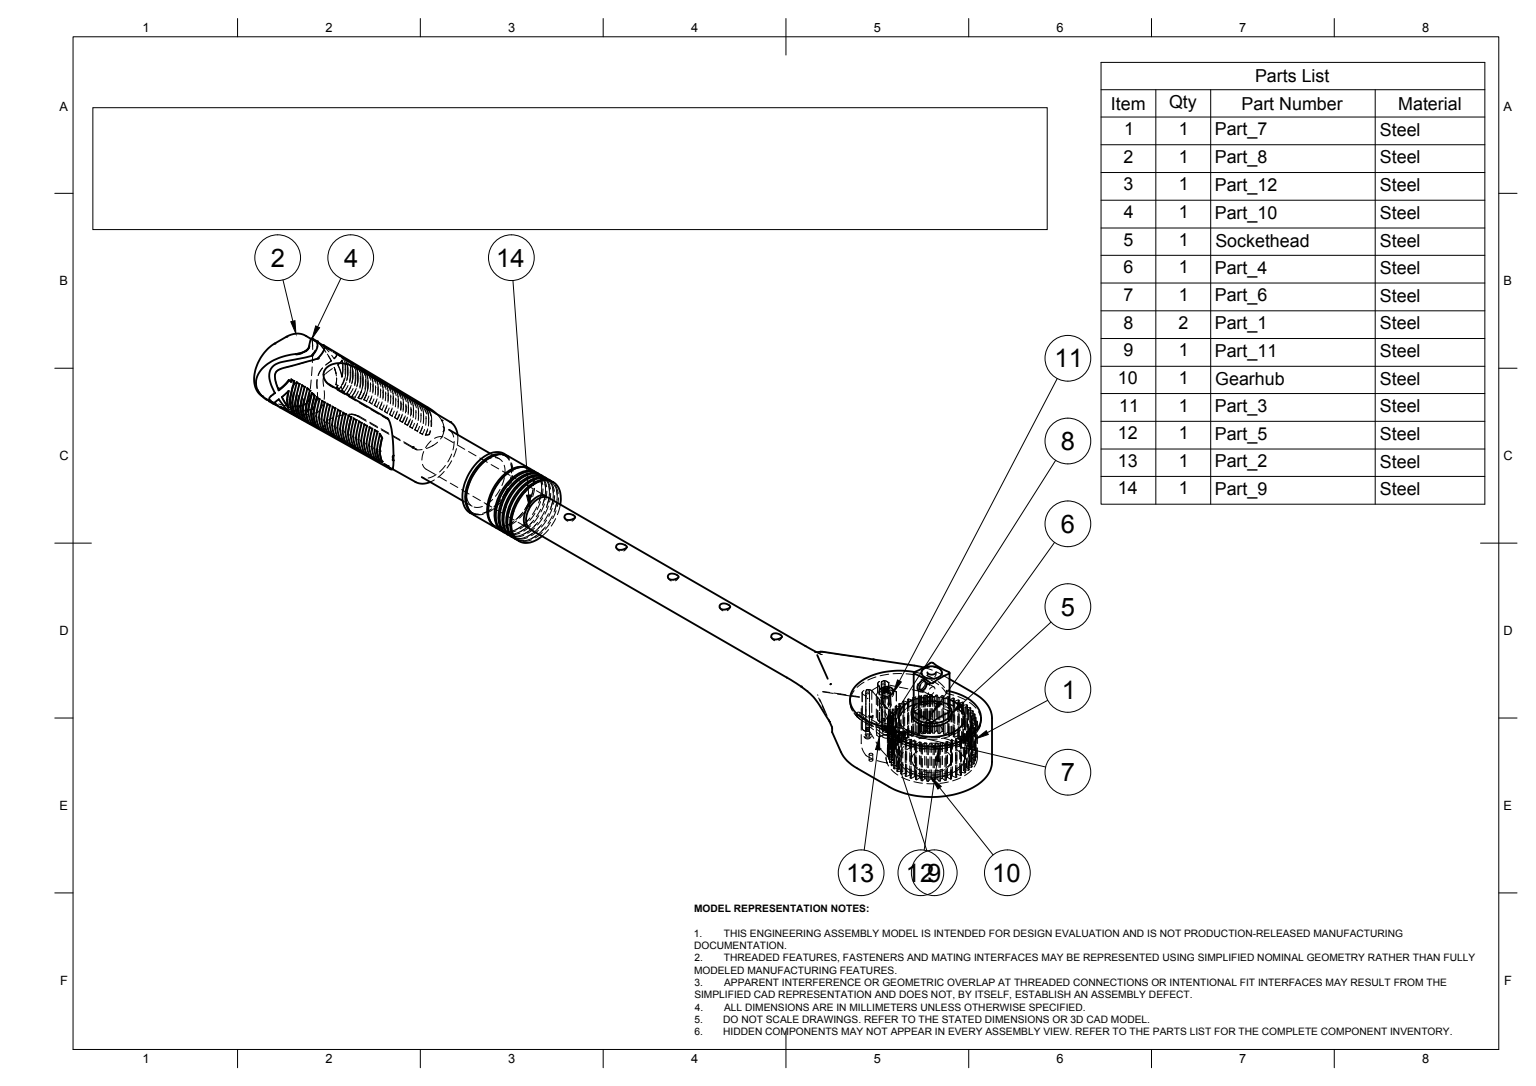
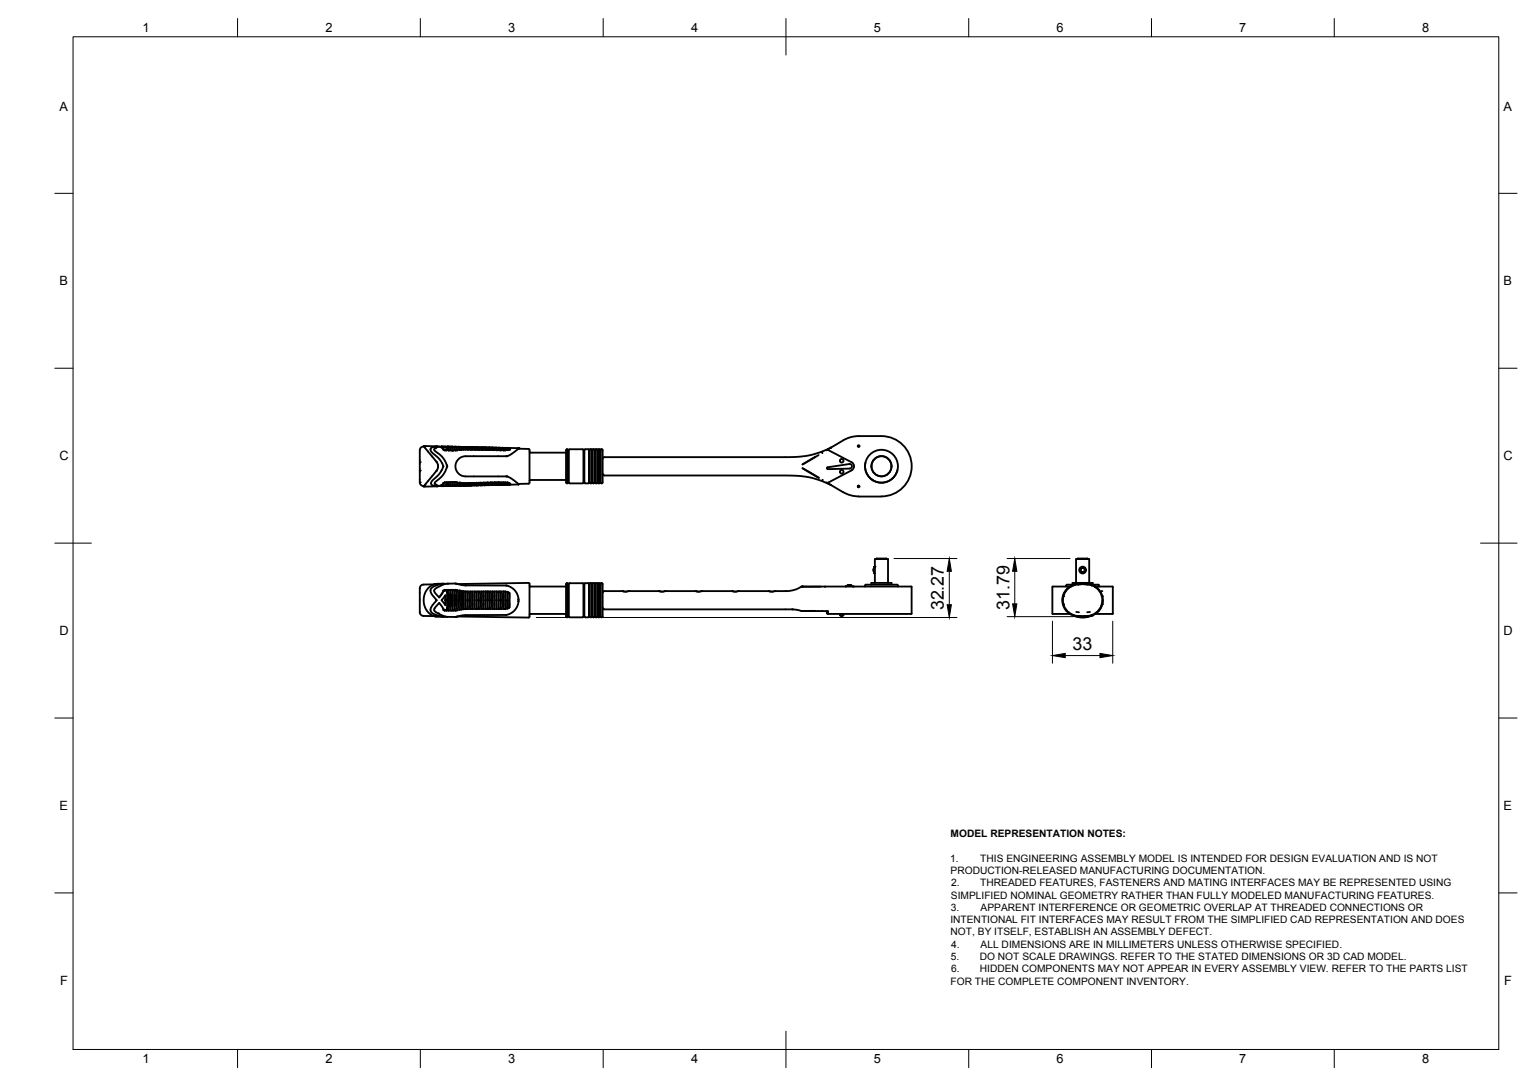
ISO-10303-21;
HEADER;
/* Generated by software containing ST-Developer
 * from STEP Tools, Inc. (www.steptools.com) 
 */

FILE_DESCRIPTION(
/* description */ ('STEP AP242 Edition 2'),
/* implementation_level */ '2;1');

FILE_NAME(
/* name */ 'MAS-615',
/* time_stamp */ '2026-10-06T10:11:12-07:00',
/* author */ (''),
/* organization */ (''),
/* preprocessor_version */ 'ST-DEVELOPER v20.2',
/* originating_system */ 'Autodesk Translation Framework v15.15.0.0',
/* authorisation */ '');

FILE_SCHEMA (('AUTOMOTIVE_DESIGN { 1 0 10303 214 3 1 1 }'));
ENDSEC;

DATA;
#10=MECHANICAL_DESIGN_GEOMETRIC_PRESENTATION_REPRESENTATION('',(#1771,#1772,
#1773,#1774,#1775,#1776,#1777,#1778,#1779,#1780,#1781,#1782,#1783,#1784,
#1785,#1786,#1787,#1788,#1789,#1790,#1791,#1792,#1793,#1794,#1795,#1796,
#1797,#1798,#1799,#1800),#54580);
#11=ITEM_DEFINED_TRANSFORMATION($,$,#17836,#19586);
#12=ITEM_DEFINED_TRANSFORMATION($,$,#18394,#19587);
#13=ITEM_DEFINED_TRANSFORMATION($,$,#18517,#19588);
#14=ITEM_DEFINED_TRANSFORMATION($,$,#18520,#19589);
#15=ITEM_DEFINED_TRANSFORMATION($,$,#18747,#19590);
#16=ITEM_DEFINED_TRANSFORMATION($,$,#18812,#19591);
#17=ITEM_DEFINED_TRANSFORMATION($,$,#18922,#19592);
#18=ITEM_DEFINED_TRANSFORMATION($,$,#19577,#19593);
#19=ITEM_DEFINED_TRANSFORMATION($,$,#19048,#19594);
#20=ITEM_DEFINED_TRANSFORMATION($,$,#19063,#19595);
#21=ITEM_DEFINED_TRANSFORMATION($,$,#19079,#19596);
#22=ITEM_DEFINED_TRANSFORMATION($,$,#19138,#19597);
#23=ITEM_DEFINED_TRANSFORMATION($,$,#19199,#19598);
#24=ITEM_DEFINED_TRANSFORMATION($,$,#19293,#19599);
#25=ITEM_DEFINED_TRANSFORMATION($,$,#19577,#19600);
#26=(
REPRESENTATION_RELATIONSHIP($,$,#54630,#54629)
REPRESENTATION_RELATIONSHIP_WITH_TRANSFORMATION(#11)
SHAPE_REPRESENTATION_RELATIONSHIP()
);
#27=(
REPRESENTATION_RELATIONSHIP($,$,#54631,#54629)
REPRESENTATION_RELATIONSHIP_WITH_TRANSFORMATION(#12)
SHAPE_REPRESENTATION_RELATIONSHIP()
);
#28=(
REPRESENTATION_RELATIONSHIP($,$,#54632,#54629)
REPRESENTATION_RELATIONSHIP_WITH_TRANSFORMATION(#13)
SHAPE_REPRESENTATION_RELATIONSHIP()
);
#29=(
REPRESENTATION_RELATIONSHIP($,$,#54633,#54629)
REPRESENTATION_RELATIONSHIP_WITH_TRANSFORMATION(#14)
SHAPE_REPRESENTATION_RELATIONSHIP()
);
#30=(
REPRESENTATION_RELATIONSHIP($,$,#54634,#54629)
REPRESENTATION_RELATIONSHIP_WITH_TRANSFORMATION(#15)
SHAPE_REPRESENTATION_RELATIONSHIP()
);
#31=(
REPRESENTATION_RELATIONSHIP($,$,#54635,#54629)
REPRESENTATION_RELATIONSHIP_WITH_TRANSFORMATION(#16)
SHAPE_REPRESENTATION_RELATIONSHIP()
);
#32=(
REPRESENTATION_RELATIONSHIP($,$,#54636,#54629)
REPRESENTATION_RELATIONSHIP_WITH_TRANSFORMATION(#17)
SHAPE_REPRESENTATION_RELATIONSHIP()
);
#33=(
REPRESENTATION_RELATIONSHIP($,$,#54643,#54629)
REPRESENTATION_RELATIONSHIP_WITH_TRANSFORMATION(#18)
SHAPE_REPRESENTATION_RELATIONSHIP()
);
#34=(
REPRESENTATION_RELATIONSHIP($,$,#54637,#54629)
REPRESENTATION_RELATIONSHIP_WITH_TRANSFORMATION(#19)
SHAPE_REPRESENTATION_RELATIONSHIP()
);
#35=(
REPRESENTATION_RELATIONSHIP($,$,#54638,#54629)
REPRESENTATION_RELATIONSHIP_WITH_TRANSFORMATION(#20)
SHAPE_REPRESENTATION_RELATIONSHIP()
);
#36=(
REPRESENTATION_RELATIONSHIP($,$,#54639,#54629)
REPRESENTATION_RELATIONSHIP_WITH_TRANSFORMATION(#21)
SHAPE_REPRESENTATION_RELATIONSHIP()
);
#37=(
REPRESENTATION_RELATIONSHIP($,$,#54640,#54629)
REPRESENTATION_RELATIONSHIP_WITH_TRANSFORMATION(#22)
SHAPE_REPRESENTATION_RELATIONSHIP()
);
#38=(
REPRESENTATION_RELATIONSHIP($,$,#54641,#54629)
REPRESENTATION_RELATIONSHIP_WITH_TRANSFORMATION(#23)
SHAPE_REPRESENTATION_RELATIONSHIP()
);
#39=(
REPRESENTATION_RELATIONSHIP($,$,#54642,#54629)
REPRESENTATION_RELATIONSHIP_WITH_TRANSFORMATION(#24)
SHAPE_REPRESENTATION_RELATIONSHIP()
);
#40=(
REPRESENTATION_RELATIONSHIP($,$,#54643,#54629)
REPRESENTATION_RELATIONSHIP_WITH_TRANSFORMATION(#25)
SHAPE_REPRESENTATION_RELATIONSHIP()
);
#41=CONTEXT_DEPENDENT_SHAPE_REPRESENTATION(#26,#54614);
#42=CONTEXT_DEPENDENT_SHAPE_REPRESENTATION(#27,#54615);
#43=CONTEXT_DEPENDENT_SHAPE_REPRESENTATION(#28,#54616);
#44=CONTEXT_DEPENDENT_SHAPE_REPRESENTATION(#29,#54617);
#45=CONTEXT_DEPENDENT_SHAPE_REPRESENTATION(#30,#54618);
#46=CONTEXT_DEPENDENT_SHAPE_REPRESENTATION(#31,#54619);
#47=CONTEXT_DEPENDENT_SHAPE_REPRESENTATION(#32,#54620);
#48=CONTEXT_DEPENDENT_SHAPE_REPRESENTATION(#33,#54621);
#49=CONTEXT_DEPENDENT_SHAPE_REPRESENTATION(#34,#54622);
#50=CONTEXT_DEPENDENT_SHAPE_REPRESENTATION(#35,#54623);
#51=CONTEXT_DEPENDENT_SHAPE_REPRESENTATION(#36,#54624);
#52=CONTEXT_DEPENDENT_SHAPE_REPRESENTATION(#37,#54625);
#53=CONTEXT_DEPENDENT_SHAPE_REPRESENTATION(#38,#54626);
#54=CONTEXT_DEPENDENT_SHAPE_REPRESENTATION(#39,#54627);
#55=CONTEXT_DEPENDENT_SHAPE_REPRESENTATION(#40,#54628);
#56=NEXT_ASSEMBLY_USAGE_OCCURRENCE('Part_7:1','Part_7:1','Part_7:1',#54645,
#54646,'Part_7:1');
#57=NEXT_ASSEMBLY_USAGE_OCCURRENCE('Part_8:1','Part_8:1','Part_8:1',#54645,
#54647,'Part_8:1');
#58=NEXT_ASSEMBLY_USAGE_OCCURRENCE('Part_12:1','Part_12:1','Part_12:1',
#54645,#54648,'Part_12:1');
#59=NEXT_ASSEMBLY_USAGE_OCCURRENCE('Part_10:1','Part_10:1','Part_10:1',
#54645,#54649,'Part_10:1');
#60=NEXT_ASSEMBLY_USAGE_OCCURRENCE('Sockethead:1','Sockethead:1',
'Sockethead:1',#54645,#54650,'Sockethead:1');
#61=NEXT_ASSEMBLY_USAGE_OCCURRENCE('Part_4:1','Part_4:1','Part_4:1',#54645,
#54651,'Part_4:1');
#62=NEXT_ASSEMBLY_USAGE_OCCURRENCE('Part_6:1','Part_6:1','Part_6:1',#54645,
#54652,'Part_6:1');
#63=NEXT_ASSEMBLY_USAGE_OCCURRENCE('Part_1:1','Part_1:1','Part_1:1',#54645,
#54659,'Part_1:1');
#64=NEXT_ASSEMBLY_USAGE_OCCURRENCE('Part_11:1','Part_11:1','Part_11:1',
#54645,#54653,'Part_11:1');
#65=NEXT_ASSEMBLY_USAGE_OCCURRENCE('Gearhub:1','Gearhub:1','Gearhub:1',
#54645,#54654,'Gearhub:1');
#66=NEXT_ASSEMBLY_USAGE_OCCURRENCE('Part_3:1','Part_3:1','Part_3:1',#54645,
#54655,'Part_3:1');
#67=NEXT_ASSEMBLY_USAGE_OCCURRENCE('Part_5:1','Part_5:1','Part_5:1',#54645,
#54656,'Part_5:1');
#68=NEXT_ASSEMBLY_USAGE_OCCURRENCE('Part_2:1','Part_2:1','Part_2:1',#54645,
#54657,'Part_2:1');
#69=NEXT_ASSEMBLY_USAGE_OCCURRENCE('Part_9:1','Part_9:1','Part_9:1',#54645,
#54658,'Part_9:1');
#70=NEXT_ASSEMBLY_USAGE_OCCURRENCE('Part_1:2','Part_1:2','Part_1:2',#54645,
#54659,'Part_1:2');
#71=ELLIPSE('',#18547,0.0043287679400298,0.000195921240702569);
#72=ELLIPSE('',#18845,0.000117970312899575,0.0001);
#73=ELLIPSE('',#18846,0.000120617936713865,0.0001);
#74=ELLIPSE('',#18848,0.000120617936713866,0.0001);
#75=ELLIPSE('',#18850,0.000120617936713866,0.0001);
#76=ELLIPSE('',#18851,0.000120617936713865,0.0001);
#77=ELLIPSE('',#18853,0.000117970312899575,0.0001);
#78=ELLIPSE('',#18855,0.000117970312899575,0.0001);
#79=ELLIPSE('',#18857,0.000117970312899574,0.0001);
#80=ELLIPSE('',#18859,0.000117970312899574,0.0001);
#81=ELLIPSE('',#18861,0.000117970312899575,0.0001);
#82=ELLIPSE('',#18863,0.000120617936713865,0.0001);
#83=ELLIPSE('',#18865,0.000117970312899575,0.0001);
#84=ELLIPSE('',#18867,0.000117970312899575,0.0001);
#85=ELLIPSE('',#18869,0.000120617936713865,0.0001);
#86=ELLIPSE('',#18871,0.000120617936713865,0.0001);
#87=ELLIPSE('',#18873,0.000136567519156022,0.0001);
#88=ELLIPSE('',#18875,0.000136567519156022,0.0001);
#89=ELLIPSE('',#18877,0.000120617936713865,0.0001);
#90=ELLIPSE('',#18879,0.000117970312899574,0.0001);
#91=ELLIPSE('',#18881,0.000100268099705458,0.0001);
#92=ELLIPSE('',#18883,0.000100268099705458,0.0001);
#93=ELLIPSE('',#18885,0.000117970312899574,0.0001);
#94=ELLIPSE('',#18887,0.000117970312899575,0.0001);
#95=ELLIPSE('',#18896,0.000117970312899575,0.0001);
#96=ELLIPSE('',#18898,0.000101375812252276,0.0001);
#97=ELLIPSE('',#18904,0.000101375812252276,0.0001);
#98=ELLIPSE('',#18957,0.000117970312899575,0.0001);
#99=ELLIPSE('',#18958,0.000120617936713865,0.0001);
#100=ELLIPSE('',#18960,0.000120617936713866,0.0001);
#101=ELLIPSE('',#18962,0.000120617936713866,0.0001);
#102=ELLIPSE('',#18963,0.000120617936713865,0.0001);
#103=ELLIPSE('',#18965,0.000117970312899575,0.0001);
#104=ELLIPSE('',#18967,0.000117970312899575,0.0001);
#105=ELLIPSE('',#18969,0.000117970312899574,0.0001);
#106=ELLIPSE('',#18971,0.000117970312899574,0.0001);
#107=ELLIPSE('',#18973,0.000117970312899575,0.0001);
#108=ELLIPSE('',#18975,0.000120617936713865,0.0001);
#109=ELLIPSE('',#18977,0.000117970312899575,0.0001);
#110=ELLIPSE('',#18979,0.000117970312899575,0.0001);
#111=ELLIPSE('',#18981,0.000120617936713865,0.0001);
#112=ELLIPSE('',#18983,0.000120617936713865,0.0001);
#113=ELLIPSE('',#18985,0.000136567519156022,0.0001);
#114=ELLIPSE('',#18987,0.000136567519156022,0.0001);
#115=ELLIPSE('',#18989,0.000120617936713865,0.0001);
#116=ELLIPSE('',#18991,0.000117970312899574,0.0001);
#117=ELLIPSE('',#19000,0.000117970312899574,0.0001);
#118=ELLIPSE('',#19002,0.000117970312899575,0.0001);
#119=ELLIPSE('',#19008,0.000117970312899575,0.0001);
#120=ELLIPSE('',#19218,0.0715418505295819,0.0129149243677278);
#121=ELLIPSE('',#19219,0.0715418505295819,0.0129149243677278);
#122=ELLIPSE('',#19224,0.0715418505290961,0.0129149243676839);
#123=ELLIPSE('',#19225,0.0715418505290961,0.0129149243676839);
#124=ELLIPSE('',#19386,0.00047049920898836,0.0004);
#125=ELLIPSE('',#19388,0.00047049920898836,0.0004);
#126=ELLIPSE('',#19445,0.000286242347628646,0.000206247332886668);
#127=ELLIPSE('',#19470,0.000318385781181688,0.0002);
#128=ELLIPSE('',#19492,0.000318385781181688,0.0002);
#129=ELLIPSE('',#19548,0.00200013961276074,0.00200000211919392);
#130=ELLIPSE('',#19569,0.00200131676890062,0.00200065811979615);
#131=CONICAL_SURFACE('',#18530,0.00265391324380841,1.37712278252772);
#132=CONICAL_SURFACE('',#18588,3.48610109958525E-5,0.141830950521549);
#133=CONICAL_SURFACE('',#18589,3.48394090574724E-5,0.141829837312193);
#134=CONICAL_SURFACE('',#18592,3.48609373749775E-5,0.141830787231043);
#135=CONICAL_SURFACE('',#18599,3.48393253777631E-5,0.141829687868949);
#136=CONICAL_SURFACE('',#18616,0.0026288792428795,1.38153808164484);
#137=CONICAL_SURFACE('',#18636,0.00265359345896356,1.37715118560564);
#138=CONICAL_SURFACE('',#18637,0.00263026865692114,1.38147192931234);
#139=CONICAL_SURFACE('',#18655,0.00614051900660571,0.733182632957209);
#140=CONICAL_SURFACE('',#18656,0.00592688725800199,0.772003379135275);
#141=CONICAL_SURFACE('',#19114,0.001,0.5235987755983);
#142=SPHERICAL_SURFACE('',#18518,0.0012);
#143=SPHERICAL_SURFACE('',#18577,0.0001);
#144=SPHERICAL_SURFACE('',#18591,0.0001);
#145=SPHERICAL_SURFACE('',#18594,0.0001);
#146=SPHERICAL_SURFACE('',#18598,0.0001);
#147=SPHERICAL_SURFACE('',#18605,0.0001);
#148=SPHERICAL_SURFACE('',#18609,0.0001);
#149=SPHERICAL_SURFACE('',#19003,0.0001);
#150=SPHERICAL_SURFACE('',#19005,0.0001);
#151=SPHERICAL_SURFACE('',#19080,0.0032);
#152=SPHERICAL_SURFACE('',#19236,0.0001);
#153=SPHERICAL_SURFACE('',#19238,0.0001);
#154=SPHERICAL_SURFACE('',#19251,0.0001);
#155=SPHERICAL_SURFACE('',#19256,0.0001);
#156=SPHERICAL_SURFACE('',#19270,0.0001);
#157=SPHERICAL_SURFACE('',#19273,0.0001);
#158=SPHERICAL_SURFACE('',#19284,0.0001);
#159=SPHERICAL_SURFACE('',#19286,0.0001);
#160=SPHERICAL_SURFACE('',#19391,0.0015);
#161=SPHERICAL_SURFACE('',#19392,0.0015);
#162=SPHERICAL_SURFACE('',#19393,0.0015);
#163=SPHERICAL_SURFACE('',#19394,0.0015);
#164=SPHERICAL_SURFACE('',#19395,0.0015);
#165=SPHERICAL_SURFACE('',#19475,0.0002);
#166=SPHERICAL_SURFACE('',#19500,0.0002);
#167=SPHERICAL_SURFACE('',#19532,0.0002);
#168=SPHERICAL_SURFACE('',#19537,0.0002);
#169=SPHERICAL_SURFACE('',#19539,0.0002);
#170=SPHERICAL_SURFACE('',#19578,0.00102870127000254);
#171=TOROIDAL_SURFACE('',#18476,0.00656151574957875,0.00199999992126171);
#172=TOROIDAL_SURFACE('',#18477,0.0065615157495791,0.00199999992126177);
#173=TOROIDAL_SURFACE('',#18479,0.0079756477610481,0.0005);
#174=TOROIDAL_SURFACE('',#18481,0.0045,0.0005);
#175=TOROIDAL_SURFACE('',#18483,0.0055,0.0005);
#176=TOROIDAL_SURFACE('',#18485,0.00882888901198444,0.0005);
#177=TOROIDAL_SURFACE('',#18487,0.00882888901198444,0.0005);
#178=TOROIDAL_SURFACE('',#18489,0.00882888901198444,0.0005);
#179=TOROIDAL_SURFACE('',#18491,0.00882888901198444,0.0005);
#180=TOROIDAL_SURFACE('',#18493,0.00882888901198444,0.0005);
#181=TOROIDAL_SURFACE('',#18495,0.00882888901198444,0.0005);
#182=TOROIDAL_SURFACE('',#18497,0.00882888901198444,0.0005);
#183=TOROIDAL_SURFACE('',#18499,0.00882888901198444,0.0005);
#184=TOROIDAL_SURFACE('',#18501,0.00882888901198444,0.0005);
#185=TOROIDAL_SURFACE('',#18503,0.00882888901198444,0.0005);
#186=TOROIDAL_SURFACE('',#18505,0.00882888901198444,0.0005);
#187=TOROIDAL_SURFACE('',#18507,0.00882888901198444,0.0005);
#188=TOROIDAL_SURFACE('',#18509,0.00882888901198444,0.0005);
#189=TOROIDAL_SURFACE('',#18511,0.00882888901198444,0.0005);
#190=TOROIDAL_SURFACE('',#18513,0.00882888901198444,0.0005);
#191=TOROIDAL_SURFACE('',#18515,0.00882888901198444,0.0005);
#192=TOROIDAL_SURFACE('',#18561,43.0172655815845,43.0171612476028);
#193=TOROIDAL_SURFACE('',#18562,43.0192266270189,43.0191222943202);
#194=TOROIDAL_SURFACE('',#18565,0.00931146593211752,9.99931797011151E-5);
#195=TOROIDAL_SURFACE('',#18566,0.00931142924739271,9.99898356076873E-5);
#196=TOROIDAL_SURFACE('',#18569,43.0172619393224,43.0171576053291);
#197=TOROIDAL_SURFACE('',#18572,43.0192273884314,43.0191230557219);
#198=TOROIDAL_SURFACE('',#18575,0.00408904168337188,9.99937992667749E-5);
#199=TOROIDAL_SURFACE('',#18576,0.00408904168282665,9.99937992622037E-5);
#200=TOROIDAL_SURFACE('',#18579,0.00806904972011834,0.0001);
#201=TOROIDAL_SURFACE('',#18596,0.00806904972011834,0.0001);
#202=TOROIDAL_SURFACE('',#18607,0.00806904972011834,0.0001);
#203=TOROIDAL_SURFACE('',#18610,0.00408913544960028,0.000100040268464404);
#204=TOROIDAL_SURFACE('',#18615,0.0040891354500689,0.000100040268460989);
#205=TOROIDAL_SURFACE('',#18659,0.00836123117893049,0.00010366855176599);
#206=TOROIDAL_SURFACE('',#18684,0.00815612470458011,0.000103667398436053);
#207=TOROIDAL_SURFACE('',#18687,0.00871025103595541,0.000103662944645038);
#208=TOROIDAL_SURFACE('',#18688,0.00850695260093233,0.000103538344715324);
#209=TOROIDAL_SURFACE('',#18689,0.00871017740815006,0.000103662875721332);
#210=TOROIDAL_SURFACE('',#18690,0.00836086459677531,0.00010366849218277);
#211=TOROIDAL_SURFACE('',#18717,0.00815633290592581,0.00010366728866353);
#212=TOROIDAL_SURFACE('',#18720,0.00864670349933223,0.000103665652215068);
#213=TOROIDAL_SURFACE('',#18721,0.00850751186664759,0.00010353842958418);
#214=TOROIDAL_SURFACE('',#18722,0.00867809676383051,0.000103667225081647);
#215=TOROIDAL_SURFACE('',#18723,0.000528332315378602,0.000103512489509189);
#216=TOROIDAL_SURFACE('',#18724,0.00917182682012945,9.99999869507318E-5);
#217=TOROIDAL_SURFACE('',#18725,0.0040475617622906,9.99881997863187E-5);
#218=TOROIDAL_SURFACE('',#18727,0.00904061800886142,0.000100004225353136);
#219=TOROIDAL_SURFACE('',#18728,0.00360779826836622,9.99961776029768E-5);
#220=TOROIDAL_SURFACE('',#18729,0.0052330922254768,9.99920638411154E-5);
#221=TOROIDAL_SURFACE('',#18730,0.000732704479508413,0.000103581963632023);
#222=TOROIDAL_SURFACE('',#18731,0.0091590450963941,9.99999843261172E-5);
#223=TOROIDAL_SURFACE('',#18733,0.00915567105502713,9.99999896646458E-5);
#224=TOROIDAL_SURFACE('',#18734,0.00389212279884052,9.99966861379351E-5);
#225=TOROIDAL_SURFACE('',#18735,0.00357438694091518,9.99963100583166E-5);
#226=TOROIDAL_SURFACE('',#18736,0.00915654585560002,9.9999989426787E-5);
#227=TOROIDAL_SURFACE('',#18738,0.009161034600788,9.9999985180343E-5);
#228=TOROIDAL_SURFACE('',#18739,0.000584574123278554,0.000103503607413102);
#229=TOROIDAL_SURFACE('',#18740,0.00392317197798013,9.99876820615925E-5);
#230=TOROIDAL_SURFACE('',#18741,0.00339615673268595,9.99957943856544E-5);
#231=TOROIDAL_SURFACE('',#18742,0.00916833013124114,9.99999895548281E-5);
#232=TOROIDAL_SURFACE('',#18744,0.00475797702577389,9.99904037368119E-5);
#233=TOROIDAL_SURFACE('',#18745,0.00917126548676907,9.99999867155255E-5);
#234=TOROIDAL_SURFACE('',#18746,0.00060192390944549,0.000103561614538704);
#235=TOROIDAL_SURFACE('',#18788,0.00268445714771808,0.0001);
#236=TOROIDAL_SURFACE('',#18804,0.00144581322131978,0.000100021493280238);
#237=TOROIDAL_SURFACE('',#18806,0.00106635989804114,0.0001);
#238=TOROIDAL_SURFACE('',#18808,0.00126635989804114,0.0001);
#239=TOROIDAL_SURFACE('',#18810,0.0045,0.001);
#240=TOROIDAL_SURFACE('',#18899,0.0002,0.0001);
#241=TOROIDAL_SURFACE('',#18901,0.0002,0.0001);
#242=TOROIDAL_SURFACE('',#18907,0.0014,0.0001);
#243=TOROIDAL_SURFACE('',#18909,0.0014,0.0001);
#244=TOROIDAL_SURFACE('',#18913,0.0002,0.0001);
#245=TOROIDAL_SURFACE('',#18915,0.0002,0.0001);
#246=TOROIDAL_SURFACE('',#18918,0.0006,0.0001);
#247=TOROIDAL_SURFACE('',#18920,0.0006,0.0001);
#248=TOROIDAL_SURFACE('',#19023,0.0002,0.0001);
#249=TOROIDAL_SURFACE('',#19025,0.0002,0.0001);
#250=TOROIDAL_SURFACE('',#19027,0.0002,0.0001);
#251=TOROIDAL_SURFACE('',#19029,0.0002,0.0001);
#252=TOROIDAL_SURFACE('',#19033,0.0014,0.0001);
#253=TOROIDAL_SURFACE('',#19035,0.0014,0.0001);
#254=TOROIDAL_SURFACE('',#19039,0.0002,0.0001);
#255=TOROIDAL_SURFACE('',#19041,0.0002,0.0001);
#256=TOROIDAL_SURFACE('',#19044,0.0006,0.0001);
#257=TOROIDAL_SURFACE('',#19046,0.0006,0.0001);
#258=TOROIDAL_SURFACE('',#19075,0.0085,0.0005);
#259=TOROIDAL_SURFACE('',#19077,0.0085,0.0005);
#260=TOROIDAL_SURFACE('',#19136,0.0011,0.0001);
#261=TOROIDAL_SURFACE('',#19179,0.0134,0.0001);
#262=TOROIDAL_SURFACE('',#19180,0.0134,0.0001);
#263=TOROIDAL_SURFACE('',#19181,0.0091,0.0001);
#264=TOROIDAL_SURFACE('',#19183,0.0013,0.0001);
#265=TOROIDAL_SURFACE('',#19185,0.0006,0.0001);
#266=TOROIDAL_SURFACE('',#19187,0.0006,0.0001);
#267=TOROIDAL_SURFACE('',#19189,0.0134,0.0001);
#268=TOROIDAL_SURFACE('',#19190,0.0134,0.0001);
#269=TOROIDAL_SURFACE('',#19191,0.0091,0.0001);
#270=TOROIDAL_SURFACE('',#19193,0.0013,0.0001);
#271=TOROIDAL_SURFACE('',#19195,0.0006,0.0001);
#272=TOROIDAL_SURFACE('',#19197,0.0006,0.0001);
#273=TOROIDAL_SURFACE('',#19243,0.0024677376190381,9.99991913251056E-5);
#274=TOROIDAL_SURFACE('',#19252,0.00160789487802693,0.0001);
#275=TOROIDAL_SURFACE('',#19254,0.00255162305984738,0.0001);
#276=TOROIDAL_SURFACE('',#19258,0.00246775438595658,9.99991912004813E-5);
#277=TOROIDAL_SURFACE('',#19259,0.00246775438598435,9.99991912004831E-5);
#278=TOROIDAL_SURFACE('',#19268,0.00160789487802693,0.0001);
#279=TOROIDAL_SURFACE('',#19275,0.00255162305984738,0.0001);
#280=TOROIDAL_SURFACE('',#19277,0.00246773761894624,9.99991913251039E-5);
#281=TOROIDAL_SURFACE('',#19289,0.0011,0.0001);
#282=TOROIDAL_SURFACE('',#19291,0.0011,0.0001);
#283=TOROIDAL_SURFACE('',#19417,0.0723798046062635,0.0693846505577955);
#284=TOROIDAL_SURFACE('',#19418,0.0725493479148083,0.0695588361081736);
#285=TOROIDAL_SURFACE('',#19419,0.0729629625245639,0.0699799856940105);
#286=TOROIDAL_SURFACE('',#19420,0.0719744531392773,0.0689794249020661);
#287=TOROIDAL_SURFACE('',#19421,0.0127,0.0002);
#288=TOROIDAL_SURFACE('',#19424,0.0004,0.0002);
#289=TOROIDAL_SURFACE('',#19429,0.0134323601801219,0.0002);
#290=TOROIDAL_SURFACE('',#19430,0.0130323601801219,0.0002);
#291=TOROIDAL_SURFACE('',#19435,0.0004,0.0002);
#292=TOROIDAL_SURFACE('',#19437,0.0013,0.0002);
#293=TOROIDAL_SURFACE('',#19438,0.0130323601801219,0.0002);
#294=TOROIDAL_SURFACE('',#19439,0.0013,0.0002);
#295=TOROIDAL_SURFACE('',#19441,0.0004,0.0002);
#296=TOROIDAL_SURFACE('',#19444,0.0130323601801219,0.0002);
#297=TOROIDAL_SURFACE('',#19449,0.0134323601801219,0.0002);
#298=TOROIDAL_SURFACE('',#19451,0.0004,0.0002);
#299=TOROIDAL_SURFACE('',#19453,0.0127,0.0002);
#300=TOROIDAL_SURFACE('',#19456,0.0163,0.0002);
#301=TOROIDAL_SURFACE('',#19461,1.2311209928723,1.23094461923187);
#302=TOROIDAL_SURFACE('',#19471,0.00114036081014246,0.000200479570708582);
#303=TOROIDAL_SURFACE('',#19473,0.0163,0.0002);
#304=TOROIDAL_SURFACE('',#19479,1.19654575499128,1.19636811754444);
#305=TOROIDAL_SURFACE('',#19485,0.0023,0.0002);
#306=TOROIDAL_SURFACE('',#19487,0.0163,0.0002);
#307=TOROIDAL_SURFACE('',#19489,0.0027,0.0002);
#308=TOROIDAL_SURFACE('',#19503,0.0123,0.0002);
#309=TOROIDAL_SURFACE('',#19506,0.0092,0.0002);
#310=TOROIDAL_SURFACE('',#19512,0.0163,0.0002);
#311=TOROIDAL_SURFACE('',#19514,0.00109148741098655,0.000200226016163471);
#312=TOROIDAL_SURFACE('',#19519,0.0163,0.0002);
#313=TOROIDAL_SURFACE('',#19525,0.0163,0.0002);
#314=TOROIDAL_SURFACE('',#19526,0.0137,0.0002);
#315=TOROIDAL_SURFACE('',#19527,0.0137,0.0002);
#316=TOROIDAL_SURFACE('',#19528,0.0092,0.0002);
#317=TOROIDAL_SURFACE('',#19530,0.0012,0.0002);
#318=TOROIDAL_SURFACE('',#19534,0.0127,0.0002);
#319=TOROIDAL_SURFACE('',#19543,0.0123,0.0002);
#320=TOROIDAL_SURFACE('',#19546,0.0127,0.0002);
#321=TOROIDAL_SURFACE('',#19547,0.0021940391762114,0.00199286501744214);
#322=TOROIDAL_SURFACE('',#19575,0.004,0.001);
#323=B_SPLINE_SURFACE_WITH_KNOTS('',3,1,((#25149,#25150),(#25151,#25152),
(#25153,#25154),(#25155,#25156),(#25157,#25158),(#25159,#25160),(#25161,
#25162),(#25163,#25164),(#25165,#25166),(#25167,#25168),(#25169,#25170),
(#25171,#25172),(#25173,#25174),(#25175,#25176),(#25177,#25178),(#25179,
#25180),(#25181,#25182),(#25183,#25184),(#25185,#25186),(#25187,#25188),
(#25189,#25190),(#25191,#25192),(#25193,#25194),(#25195,#25196),(#25197,
#25198),(#25199,#25200),(#25201,#25202),(#25203,#25204),(#25205,#25206),
(#25207,#25208)),.UNSPECIFIED.,.T.,.F.,.F.,(4,1,1,1,1,1,1,1,2,1,1,1,2,1,
1,1,1,1,1,1,2,1,1,1,4),(2,2),(-1.,-0.94727121518274,-0.894542430365479,
-0.841813645548218,-0.789084860730959,-0.736356075913698,-0.683627291096437,
-0.630898506279177,-0.578169721461916,-0.558627291096437,-0.539084860730958,
-0.519542430365479,-0.5,-0.447271215182739,-0.394542430365479,-0.341813645548219,
-0.289084860730958,-0.236356075913698,-0.183627291096437,-0.130898506279177,
-0.078169721461917,-0.0586272910964371,-0.039084860730958,-0.019542430365479,
0.),(0.0270596808612465,0.997611167870436),.UNSPECIFIED.);
#324=B_SPLINE_SURFACE_WITH_KNOTS('',3,1,((#25444,#25445),(#25446,#25447),
(#25448,#25449),(#25450,#25451),(#25452,#25453),(#25454,#25455),(#25456,
#25457),(#25458,#25459),(#25460,#25461),(#25462,#25463),(#25464,#25465),
(#25466,#25467),(#25468,#25469),(#25470,#25471),(#25472,#25473),(#25474,
#25475),(#25476,#25477),(#25478,#25479),(#25480,#25481),(#25482,#25483),
(#25484,#25485),(#25486,#25487),(#25488,#25489),(#25490,#25491),(#25492,
#25493),(#25494,#25495),(#25496,#25497),(#25498,#25499),(#25500,#25501),
(#25502,#25503)),.UNSPECIFIED.,.T.,.F.,.F.,(4,1,1,1,1,1,1,1,2,1,1,1,2,1,
1,1,1,1,1,1,2,1,1,1,4),(2,2),(0.,0.0527287848172604,0.105457569634521,0.158186354451782,
0.210915139269041,0.263643924086302,0.316372708903563,0.369101493720823,
0.421830278538084,0.441372708903563,0.460915139269042,0.480457569634521,
0.5,0.552728784817261,0.605457569634521,0.658186354451781,0.710915139269042,
0.763643924086302,0.816372708903563,0.869101493720823,0.921830278538083,
0.941372708903563,0.960915139269042,0.980457569634521,1.),(0.0270596808612465,
0.997611167870436),.UNSPECIFIED.);
#325=B_SPLINE_SURFACE_WITH_KNOTS('',3,3,((#25845,#25846,#25847,#25848),
(#25849,#25850,#25851,#25852),(#25853,#25854,#25855,#25856),(#25857,#25858,
#25859,#25860),(#25861,#25862,#25863,#25864),(#25865,#25866,#25867,#25868),
(#25869,#25870,#25871,#25872),(#25873,#25874,#25875,#25876),(#25877,#25878,
#25879,#25880),(#25881,#25882,#25883,#25884),(#25885,#25886,#25887,#25888),
(#25889,#25890,#25891,#25892),(#25893,#25894,#25895,#25896),(#25897,#25898,
#25899,#25900),(#25901,#25902,#25903,#25904),(#25905,#25906,#25907,#25908),
(#25909,#25910,#25911,#25912),(#25913,#25914,#25915,#25916),(#25917,#25918,
#25919,#25920),(#25921,#25922,#25923,#25924),(#25925,#25926,#25927,#25928),
(#25929,#25930,#25931,#25932),(#25933,#25934,#25935,#25936),(#25937,#25938,
#25939,#25940),(#25941,#25942,#25943,#25944),(#25945,#25946,#25947,#25948),
(#25949,#25950,#25951,#25952),(#25953,#25954,#25955,#25956),(#25957,#25958,
#25959,#25960),(#25961,#25962,#25963,#25964),(#25965,#25966,#25967,#25968),
(#25969,#25970,#25971,#25972),(#25973,#25974,#25975,#25976),(#25977,#25978,
#25979,#25980),(#25981,#25982,#25983,#25984),(#25985,#25986,#25987,#25988),
(#25989,#25990,#25991,#25992),(#25993,#25994,#25995,#25996),(#25997,#25998,
#25999,#26000)),.UNSPECIFIED.,.T.,.F.,.F.,(4,1,1,1,1,1,1,1,1,1,1,1,1,1,
1,1,1,1,1,1,1,1,1,1,1,1,1,1,1,1,1,1,1,1,1,1,4),(4,4),(-1.,-0.9921875,-0.984375,
-0.96875,-0.9375,-0.921875,-0.90625,-0.875,-0.84375,-0.8125,-0.78125,-0.75,
-0.6875,-0.625,-0.59375,-0.5625,-0.53125,-0.515625,-0.5,-0.4921875,-0.484375,
-0.46875,-0.4375,-0.421875,-0.40625,-0.375,-0.34375,-0.3125,-0.28125,-0.25,
-0.1875,-0.125,-0.09375,-0.0625,-0.03125,-0.015625,0.),(0.0970446199077052,
0.967246564070376),.UNSPECIFIED.);
#326=B_SPLINE_SURFACE_WITH_KNOTS('',3,1,((#26093,#26094),(#26095,#26096),
(#26097,#26098),(#26099,#26100),(#26101,#26102),(#26103,#26104),(#26105,
#26106),(#26107,#26108),(#26109,#26110),(#26111,#26112),(#26113,#26114),
(#26115,#26116),(#26117,#26118),(#26119,#26120),(#26121,#26122),(#26123,
#26124),(#26125,#26126),(#26127,#26128),(#26129,#26130),(#26131,#26132),
(#26133,#26134),(#26135,#26136),(#26137,#26138),(#26139,#26140),(#26141,
#26142),(#26143,#26144),(#26145,#26146),(#26147,#26148),(#26149,#26150),
(#26151,#26152),(#26153,#26154),(#26155,#26156)),.UNSPECIFIED.,.T.,.F.,
 .F.,(4,1,2,1,1,1,1,1,1,1,2,1,1,1,2,1,1,1,1,1,1,1,3,1,4),(2,2),(-0.962123410396902,
-0.943185115595354,-0.924246820793805,-0.871215968194179,-0.818185115594553,
-0.765154262994927,-0.712123410395301,-0.659092557795675,-0.606061705196049,
-0.553030852596423,-0.499999999996798,-0.481061705196237,-0.462123410395676,
-0.443185115595116,-0.424246820794555,-0.371215968195236,-0.318185115595916,
-0.265154262996597,-0.212123410397278,-0.159092557797958,-0.106061705198639,
-0.0530308525993189,0.,0.0189382948015488,0.0378765896030977),(0.785837404066612,
0.964086943478034),.UNSPECIFIED.);
#327=B_SPLINE_SURFACE_WITH_KNOTS('',3,1,((#26801,#26802),(#26803,#26804),
(#26805,#26806),(#26807,#26808),(#26809,#26810),(#26811,#26812),(#26813,
#26814),(#26815,#26816),(#26817,#26818),(#26819,#26820),(#26821,#26822),
(#26823,#26824),(#26825,#26826),(#26827,#26828),(#26829,#26830),(#26831,
#26832),(#26833,#26834),(#26835,#26836),(#26837,#26838),(#26839,#26840),
(#26841,#26842),(#26843,#26844),(#26845,#26846),(#26847,#26848),(#26849,
#26850),(#26851,#26852),(#26853,#26854),(#26855,#26856),(#26857,#26858),
(#26859,#26860),(#26861,#26862),(#26863,#26864),(#26865,#26866)),
 .UNSPECIFIED.,.T.,.F.,.F.,(4,1,1,1,1,3,1,1,1,2,1,1,1,1,1,1,1,2,1,1,1,2,
1,1,1,4),(2,2),(-0.237377771779514,-0.212123410397278,-0.159092557797958,
-0.106061705198639,-0.0530308525993189,0.,0.0189382948015488,0.0378765896030977,
0.0568148844046463,0.0757531792061952,0.128784031805821,0.181814884405447,
0.234845737005073,0.287876589604699,0.340907442204325,0.393938294803951,
0.446969147403577,0.500000000003202,0.518938294803763,0.537876589604324,
0.556814884404884,0.575753179205445,0.628784031804764,0.681814884404084,
0.734845737003403,0.762622228220486),(0.0953842576150604,0.872111738883991),
 .UNSPECIFIED.);
#328=B_SPLINE_SURFACE_WITH_KNOTS('',3,3,((#29129,#29130,#29131,#29132),
(#29133,#29134,#29135,#29136),(#29137,#29138,#29139,#29140),(#29141,#29142,
#29143,#29144),(#29145,#29146,#29147,#29148),(#29149,#29150,#29151,#29152),
(#29153,#29154,#29155,#29156),(#29157,#29158,#29159,#29160),(#29161,#29162,
#29163,#29164),(#29165,#29166,#29167,#29168),(#29169,#29170,#29171,#29172),
(#29173,#29174,#29175,#29176),(#29177,#29178,#29179,#29180),(#29181,#29182,
#29183,#29184),(#29185,#29186,#29187,#29188),(#29189,#29190,#29191,#29192),
(#29193,#29194,#29195,#29196),(#29197,#29198,#29199,#29200),(#29201,#29202,
#29203,#29204),(#29205,#29206,#29207,#29208),(#29209,#29210,#29211,#29212),
(#29213,#29214,#29215,#29216),(#29217,#29218,#29219,#29220),(#29221,#29222,
#29223,#29224),(#29225,#29226,#29227,#29228),(#29229,#29230,#29231,#29232),
(#29233,#29234,#29235,#29236),(#29237,#29238,#29239,#29240),(#29241,#29242,
#29243,#29244),(#29245,#29246,#29247,#29248),(#29249,#29250,#29251,#29252),
(#29253,#29254,#29255,#29256),(#29257,#29258,#29259,#29260),(#29261,#29262,
#29263,#29264),(#29265,#29266,#29267,#29268)),.UNSPECIFIED.,.T.,.F.,.F.,
(4,1,1,1,1,1,1,1,1,1,1,1,1,1,1,1,1,1,1,1,1,1,1,1,1,1,1,1,1,1,1,1,4),(4,
4),(-1.,-0.984375,-0.96875,-0.9375,-0.921875,-0.90625,-0.875,-0.84375,-0.8125,
-0.75,-0.6875,-0.625,-0.59375,-0.5625,-0.53125,-0.515625,-0.5,-0.484375,
-0.46875,-0.4375,-0.421875,-0.40625,-0.375,-0.34375,-0.3125,-0.25,-0.1875,
-0.125,-0.09375,-0.0625,-0.03125,-0.015625,0.),(0.748401658952503,0.903433079647334),
 .UNSPECIFIED.);
#329=B_SPLINE_SURFACE_WITH_KNOTS('',3,3,((#30017,#30018,#30019,#30020),
(#30021,#30022,#30023,#30024),(#30025,#30026,#30027,#30028),(#30029,#30030,
#30031,#30032),(#30033,#30034,#30035,#30036),(#30037,#30038,#30039,#30040),
(#30041,#30042,#30043,#30044),(#30045,#30046,#30047,#30048),(#30049,#30050,
#30051,#30052),(#30053,#30054,#30055,#30056),(#30057,#30058,#30059,#30060),
(#30061,#30062,#30063,#30064),(#30065,#30066,#30067,#30068),(#30069,#30070,
#30071,#30072),(#30073,#30074,#30075,#30076),(#30077,#30078,#30079,#30080),
(#30081,#30082,#30083,#30084),(#30085,#30086,#30087,#30088),(#30089,#30090,
#30091,#30092),(#30093,#30094,#30095,#30096),(#30097,#30098,#30099,#30100),
(#30101,#30102,#30103,#30104),(#30105,#30106,#30107,#30108),(#30109,#30110,
#30111,#30112),(#30113,#30114,#30115,#30116),(#30117,#30118,#30119,#30120),
(#30121,#30122,#30123,#30124),(#30125,#30126,#30127,#30128),(#30129,#30130,
#30131,#30132),(#30133,#30134,#30135,#30136),(#30137,#30138,#30139,#30140),
(#30141,#30142,#30143,#30144),(#30145,#30146,#30147,#30148),(#30149,#30150,
#30151,#30152),(#30153,#30154,#30155,#30156)),.UNSPECIFIED.,.T.,.F.,.F.,
(4,1,1,1,1,1,1,1,1,1,1,1,1,1,1,1,1,1,1,1,1,1,1,1,1,1,1,1,1,1,1,1,4),(4,
4),(1.,1.015625,1.03125,1.0625,1.078125,1.09375,1.125,1.15625,1.1875,1.25,
1.3125,1.375,1.40625,1.4375,1.46875,1.484375,1.5,1.515625,1.53125,1.5625,
1.578125,1.59375,1.625,1.65625,1.6875,1.75,1.8125,1.875,1.90625,1.9375,
1.96875,1.984375,2.),(0.748401658952503,0.903433079647334),
 .UNSPECIFIED.);
#330=B_SPLINE_SURFACE_WITH_KNOTS('',3,1,((#30336,#30337),(#30338,#30339),
(#30340,#30341),(#30342,#30343),(#30344,#30345),(#30346,#30347),(#30348,
#30349),(#30350,#30351),(#30352,#30353),(#30354,#30355),(#30356,#30357),
(#30358,#30359),(#30360,#30361),(#30362,#30363),(#30364,#30365),(#30366,
#30367),(#30368,#30369),(#30370,#30371),(#30372,#30373),(#30374,#30375),
(#30376,#30377),(#30378,#30379),(#30380,#30381),(#30382,#30383),(#30384,
#30385),(#30386,#30387),(#30388,#30389),(#30390,#30391),(#30392,#30393),
(#30394,#30395)),.UNSPECIFIED.,.T.,.F.,.F.,(4,1,1,1,2,1,1,1,1,1,1,1,2,1,
1,1,2,1,1,1,1,1,1,1,4),(2,2),(1.,1.01893829480155,1.0378765896031,1.05681488440465,
1.0757531792062,1.12878403180582,1.18181488440545,1.23484573700507,1.2878765896047,
1.34090744220433,1.39393829480395,1.44696914740358,1.5000000000032,1.51893829480376,
1.53787658960432,1.55681488440488,1.57575317920544,1.62878403180476,1.68181488440408,
1.7348457370034,1.78787658960272,1.84090744220204,1.89393829480136,1.94696914740068,
2.),(0.0953842576150604,0.872111738883991),.UNSPECIFIED.);
#331=B_SPLINE_SURFACE_WITH_KNOTS('',3,1,((#34950,#34951),(#34952,#34953),
(#34954,#34955),(#34956,#34957),(#34958,#34959),(#34960,#34961),(#34962,
#34963),(#34964,#34965),(#34966,#34967),(#34968,#34969),(#34970,#34971),
(#34972,#34973),(#34974,#34975),(#34976,#34977),(#34978,#34979),(#34980,
#34981),(#34982,#34983),(#34984,#34985),(#34986,#34987),(#34988,#34989),
(#34990,#34991),(#34992,#34993),(#34994,#34995),(#34996,#34997),(#34998,
#34999),(#35000,#35001),(#35002,#35003),(#35004,#35005),(#35006,#35007),
(#35008,#35009)),.UNSPECIFIED.,.T.,.F.,.F.,(4,1,1,1,2,1,1,1,1,1,1,1,2,1,
1,1,2,1,1,1,1,1,1,1,4),(2,2),(1.,1.01893829480155,1.0378765896031,1.05681488440465,
1.0757531792062,1.12878403180582,1.18181488440545,1.23484573700507,1.2878765896047,
1.34090744220433,1.39393829480395,1.44696914740358,1.5000000000032,1.51893829480376,
1.53787658960432,1.55681488440488,1.57575317920544,1.62878403180476,1.68181488440408,
1.7348457370034,1.78787658960272,1.84090744220204,1.89393829480136,1.94696914740068,
2.),(0.785837404066612,0.964086943478034),.UNSPECIFIED.);
#332=B_SPLINE_SURFACE_WITH_KNOTS('',1,3,((#35025,#35026,#35027,#35028,#35029,
#35030,#35031,#35032,#35033,#35034,#35035,#35036,#35037,#35038,#35039,#35040,
#35041,#35042,#35043,#35044),(#35045,#35046,#35047,#35048,#35049,#35050,
#35051,#35052,#35053,#35054,#35055,#35056,#35057,#35058,#35059,#35060,#35061,
#35062,#35063,#35064),(#35065,#35066,#35067,#35068,#35069,#35070,#35071,
#35072,#35073,#35074,#35075,#35076,#35077,#35078,#35079,#35080,#35081,#35082,
#35083,#35084)),.UNSPECIFIED.,.F.,.F.,.F.,(2,1,2),(4,2,2,2,2,2,2,2,2,4),
(0.,1.,1.005),(0.999268187708551,0.99938964839267,0.999511718705164,0.999633789017659,
0.999694824173906,0.999755859330153,0.999877929642648,0.999908447220771,
0.999938964798895,0.999999999955142),.UNSPECIFIED.);
#333=B_SPLINE_SURFACE_WITH_KNOTS('',3,3,((#35229,#35230,#35231,#35232),
(#35233,#35234,#35235,#35236),(#35237,#35238,#35239,#35240),(#35241,#35242,
#35243,#35244),(#35245,#35246,#35247,#35248),(#35249,#35250,#35251,#35252),
(#35253,#35254,#35255,#35256),(#35257,#35258,#35259,#35260),(#35261,#35262,
#35263,#35264),(#35265,#35266,#35267,#35268),(#35269,#35270,#35271,#35272),
(#35273,#35274,#35275,#35276),(#35277,#35278,#35279,#35280),(#35281,#35282,
#35283,#35284),(#35285,#35286,#35287,#35288),(#35289,#35290,#35291,#35292),
(#35293,#35294,#35295,#35296),(#35297,#35298,#35299,#35300),(#35301,#35302,
#35303,#35304),(#35305,#35306,#35307,#35308),(#35309,#35310,#35311,#35312),
(#35313,#35314,#35315,#35316),(#35317,#35318,#35319,#35320),(#35321,#35322,
#35323,#35324),(#35325,#35326,#35327,#35328),(#35329,#35330,#35331,#35332),
(#35333,#35334,#35335,#35336),(#35337,#35338,#35339,#35340),(#35341,#35342,
#35343,#35344),(#35345,#35346,#35347,#35348),(#35349,#35350,#35351,#35352),
(#35353,#35354,#35355,#35356),(#35357,#35358,#35359,#35360),(#35361,#35362,
#35363,#35364),(#35365,#35366,#35367,#35368),(#35369,#35370,#35371,#35372),
(#35373,#35374,#35375,#35376),(#35377,#35378,#35379,#35380),(#35381,#35382,
#35383,#35384)),.UNSPECIFIED.,.T.,.F.,.F.,(4,1,1,1,1,1,1,1,1,1,1,1,1,1,
1,1,1,1,1,1,1,1,1,1,1,1,1,1,1,1,1,1,1,1,1,1,4),(4,4),(0.,0.0078125,0.015625,
0.03125,0.0625,0.078125,0.09375,0.125,0.15625,0.1875,0.21875,0.25,0.3125,
0.375,0.40625,0.4375,0.46875,0.484375,0.5,0.5078125,0.515625,0.53125,0.5625,
0.578125,0.59375,0.625,0.65625,0.6875,0.71875,0.75,0.8125,0.875,0.90625,
0.9375,0.96875,0.984375,1.),(0.0970446199077052,0.967246564070376),
 .UNSPECIFIED.);
#334=B_SPLINE_SURFACE_WITH_KNOTS('',3,3,((#37152,#37153,#37154,#37155),
(#37156,#37157,#37158,#37159),(#37160,#37161,#37162,#37163),(#37164,#37165,
#37166,#37167),(#37168,#37169,#37170,#37171),(#37172,#37173,#37174,#37175),
(#37176,#37177,#37178,#37179),(#37180,#37181,#37182,#37183),(#37184,#37185,
#37186,#37187),(#37188,#37189,#37190,#37191),(#37192,#37193,#37194,#37195),
(#37196,#37197,#37198,#37199),(#37200,#37201,#37202,#37203),(#37204,#37205,
#37206,#37207),(#37208,#37209,#37210,#37211),(#37212,#37213,#37214,#37215),
(#37216,#37217,#37218,#37219),(#37220,#37221,#37222,#37223),(#37224,#37225,
#37226,#37227),(#37228,#37229,#37230,#37231),(#37232,#37233,#37234,#37235),
(#37236,#37237,#37238,#37239),(#37240,#37241,#37242,#37243),(#37244,#37245,
#37246,#37247),(#37248,#37249,#37250,#37251),(#37252,#37253,#37254,#37255),
(#37256,#37257,#37258,#37259),(#37260,#37261,#37262,#37263),(#37264,#37265,
#37266,#37267),(#37268,#37269,#37270,#37271),(#37272,#37273,#37274,#37275),
(#37276,#37277,#37278,#37279),(#37280,#37281,#37282,#37283),(#37284,#37285,
#37286,#37287),(#37288,#37289,#37290,#37291)),.UNSPECIFIED.,.T.,.F.,.F.,
(4,1,1,1,1,1,1,1,1,1,1,1,1,1,1,1,1,1,1,1,1,1,1,1,1,1,1,1,1,1,1,1,4),(4,
4),(0.,0.015625,0.03125,0.0625,0.078125,0.09375,0.125,0.15625,0.1875,0.25,
0.3125,0.375,0.40625,0.4375,0.46875,0.484375,0.5,0.515625,0.53125,0.5625,
0.578125,0.59375,0.625,0.65625,0.6875,0.75,0.8125,0.875,0.90625,0.9375,
0.96875,0.984375,1.),(0.748401658952503,0.903433079647334),
 .UNSPECIFIED.);
#335=B_SPLINE_SURFACE_WITH_KNOTS('',3,3,((#44797,#44798,#44799,#44800,#44801),
(#44802,#44803,#44804,#44805,#44806),(#44807,#44808,#44809,#44810,#44811),
(#44812,#44813,#44814,#44815,#44816),(#44817,#44818,#44819,#44820,#44821),
(#44822,#44823,#44824,#44825,#44826),(#44827,#44828,#44829,#44830,#44831),
(#44832,#44833,#44834,#44835,#44836),(#44837,#44838,#44839,#44840,#44841)),
 .UNSPECIFIED.,.F.,.F.,.F.,(4,1,1,1,1,1,4),(4,1,4),(0.00214678110273797,
0.00328311417485291,0.00393151580676355,0.00522831907058484,0.00652512233440613,
0.00717352396631677,0.00830134515056596),(-0.00760700162757571,0.496196499186212,
1.0043667759093),.UNSPECIFIED.);
#336=B_SPLINE_SURFACE_WITH_KNOTS('',3,3,((#44958,#44959,#44960,#44961,#44962),
(#44963,#44964,#44965,#44966,#44967),(#44968,#44969,#44970,#44971,#44972),
(#44973,#44974,#44975,#44976,#44977),(#44978,#44979,#44980,#44981,#44982),
(#44983,#44984,#44985,#44986,#44987),(#44988,#44989,#44990,#44991,#44992),
(#44993,#44994,#44995,#44996,#44997),(#44998,#44999,#45000,#45001,#45002)),
 .UNSPECIFIED.,.F.,.F.,.F.,(4,1,1,1,1,1,4),(4,1,4),(0.0021509040335451,
0.00328755319845632,0.00393613508633228,0.0052332988620842,0.00653046263783612,
0.00717904452571208,0.0083071902285716),(-0.00767667710147584,0.496161661449262,
1.00435471660804),.UNSPECIFIED.);
#337=B_SPLINE_SURFACE_WITH_KNOTS('',3,3,((#50042,#50043,#50044,#50045),
(#50046,#50047,#50048,#50049),(#50050,#50051,#50052,#50053),(#50054,#50055,
#50056,#50057),(#50058,#50059,#50060,#50061),(#50062,#50063,#50064,#50065),
(#50066,#50067,#50068,#50069)),.UNSPECIFIED.,.F.,.F.,.F.,(4,1,1,1,4),(4,
4),(0.581678330580955,0.66570223965942,0.749726148737884,0.833750057816349,
0.917773966894813),(0.,0.272096154167828),.UNSPECIFIED.);
#338=B_SPLINE_SURFACE_WITH_KNOTS('',3,3,((#50328,#50329,#50330,#50331),
(#50332,#50333,#50334,#50335),(#50336,#50337,#50338,#50339),(#50340,#50341,
#50342,#50343),(#50344,#50345,#50346,#50347),(#50348,#50349,#50350,#50351),
(#50352,#50353,#50354,#50355)),.UNSPECIFIED.,.F.,.F.,.F.,(4,1,1,1,4),(4,
4),(0.082398587787618,0.16607539724211,0.249752206696602,0.333429016151093,
0.417105825605585),(0.,0.340678729399104),.UNSPECIFIED.);
#339=B_SPLINE_SURFACE_WITH_KNOTS('',3,3,((#50620,#50621,#50622,#50623),
(#50624,#50625,#50626,#50627),(#50628,#50629,#50630,#50631),(#50632,#50633,
#50634,#50635),(#50636,#50637,#50638,#50639),(#50640,#50641,#50642,#50643),
(#50644,#50645,#50646,#50647),(#50648,#50649,#50650,#50651),(#50652,#50653,
#50654,#50655),(#50656,#50657,#50658,#50659)),.UNSPECIFIED.,.F.,.F.,.F.,
(4,3,1,1,1,4),(4,4),(0.88386669972742,0.917773966894813,0.93833047517111,
0.958886983447406,0.979443491723703,1.),(0.,1.),.UNSPECIFIED.);
#340=B_SPLINE_SURFACE_WITH_KNOTS('',3,3,((#50859,#50860,#50861,#50862),
(#50863,#50864,#50865,#50866),(#50867,#50868,#50869,#50870),(#50871,#50872,
#50873,#50874),(#50875,#50876,#50877,#50878),(#50879,#50880,#50881,#50882),
(#50883,#50884,#50885,#50886),(#50887,#50888,#50889,#50890),(#50891,#50892,
#50893,#50894),(#50895,#50896,#50897,#50898),(#50899,#50900,#50901,#50902),
(#50903,#50904,#50905,#50906),(#50907,#50908,#50909,#50910),(#50911,#50912,
#50913,#50914),(#50915,#50916,#50917,#50918),(#50919,#50920,#50921,#50922),
(#50923,#50924,#50925,#50926),(#50927,#50928,#50929,#50930)),
 .UNSPECIFIED.,.F.,.F.,.F.,(4,3,1,1,1,2,1,1,1,3,4),(4,4),(0.414454525410024,
0.417105825605585,0.437698866011632,0.45829190641768,0.478884946823728,
0.499477987229775,0.52002807306757,0.540578158905365,0.56112824474316,0.581678330580955,
0.616449456714453),(0.,1.),.UNSPECIFIED.);
#341=B_SPLINE_SURFACE_WITH_KNOTS('',3,3,((#51085,#51086,#51087,#51088),
(#51089,#51090,#51091,#51092),(#51093,#51094,#51095,#51096),(#51097,#51098,
#51099,#51100),(#51101,#51102,#51103,#51104),(#51105,#51106,#51107,#51108),
(#51109,#51110,#51111,#51112),(#51113,#51114,#51115,#51116),(#51117,#51118,
#51119,#51120),(#51121,#51122,#51123,#51124)),.UNSPECIFIED.,.F.,.F.,.F.,
(4,1,1,1,3,4),(4,4),(0.,0.0205996469469045,0.041199293893809,0.0617989408407135,
0.082398587787618,0.082892979314345),(0.,1.),.UNSPECIFIED.);
#342=B_SPLINE_SURFACE_WITH_KNOTS('',3,3,((#53343,#53344,#53345,#53346),
(#53347,#53348,#53349,#53350),(#53351,#53352,#53353,#53354),(#53355,#53356,
#53357,#53358),(#53359,#53360,#53361,#53362),(#53363,#53364,#53365,#53366),
(#53367,#53368,#53369,#53370),(#53371,#53372,#53373,#53374),(#53375,#53376,
#53377,#53378),(#53379,#53380,#53381,#53382),(#53383,#53384,#53385,#53386)),
 .UNSPECIFIED.,.F.,.F.,.F.,(4,1,1,1,1,1,1,1,4),(4,4),(-0.00100716856165045,
0.00254911418953192,0.00509822837906388,0.00764734256859584,0.0101964567581278,
0.0127455709476598,0.0152946851371917,0.0178437993267237,0.0213314374719094),
(0.,1.00749523383058),.UNSPECIFIED.);
#343=B_SPLINE_CURVE_WITH_KNOTS('',3,(#24904,#24905,#24906,#24907,#24908,
#24909,#24910,#24911,#24912,#24913,#24914,#24915,#24916,#24917,#24918,#24919,
#24920,#24921,#24922,#24923,#24924,#24925,#24926,#24927,#24928,#24929,#24930,
#24931,#24932,#24933,#24934,#24935,#24936,#24937,#24938,#24939,#24940,#24941,
#24942,#24943,#24944,#24945,#24946,#24947,#24948,#24949,#24950,#24951,#24952,
#24953,#24954,#24955,#24956,#24957,#24958,#24959,#24960,#24961,#24962,#24963,
#24964,#24965,#24966,#24967,#24968,#24969,#24970,#24971,#24972,#24973,#24974,
#24975,#24976,#24977,#24978,#24979,#24980,#24981,#24982,#24983,#24984,#24985,
#24986,#24987,#24988,#24989,#24990,#24991,#24992,#24993,#24994,#24995,#24996,
#24997,#24998,#24999,#25000,#25001,#25002,#25003,#25004,#25005,#25006,#25007,
#25008,#25009,#25010,#25011,#25012,#25013,#25014,#25015,#25016,#25017,#25018,
#25019,#25020,#25021,#25022,#25023,#25024,#25025,#25026,#25027,#25028,#25029,
#25030,#25031,#25032,#25033,#25034,#25035,#25036,#25037,#25038,#25039,#25040,
#25041,#25042,#25043,#25044,#25045),.UNSPECIFIED.,.F.,.F.,(4,3,3,3,3,3,
3,3,3,3,3,3,3,3,3,3,3,3,3,3,3,3,3,3,3,3,3,3,3,3,3,3,3,3,3,3,3,3,3,3,3,3,
3,3,3,3,3,4),(1.65573441350565E-7,0.00176667375437257,0.00259221926243185,
0.00265001063155886,0.00353334750874515,0.00441668438593144,0.00612523623771844,
0.0070666950174903,0.00965970053988215,0.0106000425262354,0.0114833794034217,
0.0131911273471506,0.0141333900349806,0.0150167269121669,0.0167215202745876,
0.0176667375437257,0.018550074420912,0.0202567299474385,0.0212000850524709,
0.0220834219296572,0.0237972002706092,0.024733432561216,0.0265001063155886,
0.0273265094643739,0.0273834431927749,0.0282667800699612,0.0291501169471475,
0.0308585741103488,0.0318001275787063,0.0326834644558926,0.0343965954050026,
0.0353334750874515,0.0379347075752174,0.0388668225961966,0.0397501594733829,
0.0414708448549527,0.0424001701049418,0.0432835069821281,0.0450045160112871,
0.0459335176136869,0.0468168544908732,0.0485354593167441,0.0494668651224321,
0.0503502019996184,0.052066506161832,0.0530002126311772,0.0538835495083635,
0.0555994356637866),.UNSPECIFIED.);
#344=B_SPLINE_CURVE_WITH_KNOTS('',3,(#25051,#25052,#25053,#25054,#25055,
#25056,#25057,#25058,#25059,#25060,#25061,#25062,#25063,#25064,#25065,#25066,
#25067,#25068,#25069,#25070,#25071,#25072,#25073,#25074,#25075,#25076,#25077,
#25078,#25079,#25080,#25081,#25082,#25083,#25084,#25085,#25086,#25087,#25088,
#25089,#25090,#25091,#25092,#25093,#25094,#25095,#25096,#25097,#25098,#25099,
#25100,#25101,#25102,#25103,#25104,#25105,#25106,#25107,#25108,#25109,#25110,
#25111,#25112,#25113,#25114,#25115,#25116,#25117),.UNSPECIFIED.,.F.,.F.,
(4,3,3,3,3,3,3,3,3,3,3,3,3,3,3,3,3,3,3,3,3,3,4),(0.0193063570369876,0.0197413378854143,
0.0225007291837996,0.0234952979646733,0.0262508507144329,0.0272500609140882,
0.0300009722450662,0.0309993547899246,0.0337510937756994,0.0347455027219703,
0.0375012153063327,0.0385033658381765,0.041251336836966,0.0422556599874251,
0.0450014583675992,0.0460030914440076,0.0487515798982325,0.0497511536421023,
0.0525017014288658,0.053501189887995,0.0562518229594991,0.057250590934481,
0.0600019444901323),.UNSPECIFIED.);
#345=B_SPLINE_CURVE_WITH_KNOTS('',3,(#25118,#25119,#25120,#25121,#25122,
#25123,#25124,#25125,#25126,#25127,#25128,#25129,#25130,#25131,#25132,#25133,
#25134,#25135,#25136,#25137,#25138,#25139,#25140,#25141,#25142,#25143,#25144,
#25145,#25146,#25147,#25148),.UNSPECIFIED.,.F.,.F.,(4,3,3,3,3,3,3,3,3,3,
4),(0.000991839717425502,0.00375012153063327,0.00474188317058086,0.00750024306126654,
0.00848950942012792,0.0112503645918998,0.0122372989824959,0.0150004861225331,
0.0159882081557064,0.0187506076531663,0.0193063570369876),.UNSPECIFIED.);
#346=B_SPLINE_CURVE_WITH_KNOTS('',1,(#25210,#25211),.UNSPECIFIED.,.F.,.F.,
(2,2),(-0.991582441935872,-0.0329929514257554),.UNSPECIFIED.);
#347=B_SPLINE_CURVE_WITH_KNOTS('',1,(#25213,#25214),.UNSPECIFIED.,.F.,.F.,
(2,2),(-0.991765438998876,-0.0337011078849239),.UNSPECIFIED.);
#348=B_SPLINE_CURVE_WITH_KNOTS('',3,(#25216,#25217,#25218,#25219,#25220,
#25221,#25222,#25223),.UNSPECIFIED.,.F.,.F.,(4,1,1,1,1,4),(0.,0.0625,0.125,
0.15625,0.1875,0.214595707386903),.UNSPECIFIED.);
#349=B_SPLINE_CURVE_WITH_KNOTS('',3,(#25225,#25226,#25227,#25228,#25229,
#25230,#25231,#25232,#25233,#25234,#25235,#25236,#25237,#25238,#25239,#25240,
#25241,#25242,#25243),.UNSPECIFIED.,.F.,.F.,(4,3,3,3,3,3,4),(1.18815451677939E-5,
0.00305752378009468,0.257254477967242,0.499999999995986,0.742745522020828,
0.996942476194294,0.99998811883621),.UNSPECIFIED.);
#350=B_SPLINE_CURVE_WITH_KNOTS('',3,(#25245,#25246,#25247,#25248,#25249,
#25250,#25251,#25252,#25253,#25254,#25255,#25256,#25257,#25258,#25259,#25260,
#25261,#25262,#25263,#25264,#25265,#25266,#25267,#25268,#25269,#25270,#25271,
#25272,#25273,#25274,#25275,#25276,#25277,#25278,#25279),.UNSPECIFIED.,
 .F.,.F.,(4,1,1,1,1,1,1,1,1,1,1,1,1,1,1,1,1,1,1,1,1,1,1,1,1,1,1,1,1,1,1,
1,4),(0.,0.0625,0.125,0.15625,0.1875,0.21875,0.234375,0.2421875,0.25,0.2578125,
0.265625,0.28125,0.3125,0.34375,0.375,0.4375,0.5,0.5625,0.625,0.65625,0.6875,
0.71875,0.734375,0.7421875,0.75,0.7578125,0.765625,0.78125,0.8125,0.84375,
0.875,0.9375,1.),.UNSPECIFIED.);
#351=B_SPLINE_CURVE_WITH_KNOTS('',3,(#25280,#25281,#25282,#25283,#25284,
#25285,#25286,#25287,#25288,#25289,#25290,#25291,#25292,#25293,#25294,#25295),
 .UNSPECIFIED.,.F.,.F.,(4,3,3,3,3,4),(0.00305752354988625,0.25725447786239,
0.499999999961484,0.742745522020858,0.996942476194068,0.999988118836217),
 .UNSPECIFIED.);
#352=B_SPLINE_CURVE_WITH_KNOTS('',3,(#25505,#25506,#25507,#25508),
 .UNSPECIFIED.,.F.,.F.,(4,4),(1.18815450203416E-5,0.00305752354988625),
 .UNSPECIFIED.);
#353=B_SPLINE_CURVE_WITH_KNOTS('',3,(#25509,#25510,#25511,#25512,#25513,
#25514,#25515,#25516,#25517,#25518,#25519,#25520,#25521,#25522,#25523,#25524,
#25525,#25526,#25527,#25528,#25529,#25530,#25531,#25532,#25533,#25534,#25535,
#25536,#25537,#25538,#25539),.UNSPECIFIED.,.F.,.F.,(4,1,1,1,1,1,1,1,1,1,
1,1,1,1,1,1,1,1,1,1,1,1,1,1,1,1,1,1,4),(0.214595707386903,0.21875,0.234375,
0.2421875,0.25,0.2578125,0.265625,0.28125,0.3125,0.34375,0.375,0.4375,0.5,
0.5625,0.625,0.65625,0.6875,0.71875,0.734375,0.7421875,0.75,0.7578125,0.765625,
0.78125,0.8125,0.84375,0.875,0.9375,1.),.UNSPECIFIED.);
#354=B_SPLINE_CURVE_WITH_KNOTS('',3,(#25540,#25541,#25542,#25543),
 .UNSPECIFIED.,.F.,.F.,(4,4),(0.,0.000991839717425502),.UNSPECIFIED.);
#355=B_SPLINE_CURVE_WITH_KNOTS('',3,(#25546,#25547,#25548,#25549),
 .UNSPECIFIED.,.F.,.F.,(4,4),(0.,1.65573441350565E-7),.UNSPECIFIED.);
#356=B_SPLINE_CURVE_WITH_KNOTS('',3,(#25550,#25551,#25552,#25553),
 .UNSPECIFIED.,.F.,.F.,(4,4),(0.0555994356637866,0.0565335601399224),
 .UNSPECIFIED.);
#357=B_SPLINE_CURVE_WITH_KNOTS('',3,(#25562,#25563,#25564,#25565,#25566,
#25567,#25568,#25569,#25570,#25571,#25572,#25573,#25574,#25575,#25576,#25577,
#25578,#25579,#25580,#25581,#25582,#25583,#25584,#25585,#25586),
 .UNSPECIFIED.,.F.,.F.,(4,3,3,3,3,3,3,3,4),(0.,0.144356336537315,0.25,0.395552475785214,
0.5,0.64383331940147,0.75,0.898848831223356,1.),.UNSPECIFIED.);
#358=B_SPLINE_CURVE_WITH_KNOTS('',3,(#25588,#25589,#25590,#25591,#25592,
#25593,#25594,#25595,#25596,#25597,#25598,#25599,#25600,#25601,#25602,#25603,
#25604,#25605,#25606,#25607,#25608,#25609,#25610,#25611,#25612,#25613,#25614,
#25615,#25616,#25617,#25618,#25619,#25620,#25621,#25622,#25623,#25624),
 .UNSPECIFIED.,.F.,.F.,(4,3,3,3,3,3,3,3,3,3,3,3,4),(0.,0.125,0.1875,0.25,
0.3125,0.375,0.5,0.625,0.6875,0.75,0.8125,0.875,1.),.UNSPECIFIED.);
#359=B_SPLINE_CURVE_WITH_KNOTS('',3,(#25626,#25627,#25628,#25629,#25630,
#25631,#25632,#25633,#25634,#25635,#25636,#25637,#25638,#25639,#25640,#25641,
#25642,#25643,#25644,#25645,#25646,#25647,#25648,#25649,#25650),
 .UNSPECIFIED.,.F.,.F.,(4,3,3,3,3,3,3,3,4),(0.,0.144356336542805,0.25,0.395552475791052,
0.5,0.643833319408362,0.75,0.898848831228882,1.),.UNSPECIFIED.);
#360=B_SPLINE_CURVE_WITH_KNOTS('',3,(#25651,#25652,#25653,#25654,#25655,
#25656,#25657,#25658,#25659,#25660,#25661,#25662,#25663,#25664,#25665,#25666,
#25667,#25668,#25669,#25670,#25671,#25672,#25673,#25674,#25675,#25676,#25677,
#25678,#25679,#25680,#25681,#25682,#25683,#25684,#25685,#25686,#25687),
 .UNSPECIFIED.,.F.,.F.,(4,3,3,3,3,3,3,3,3,3,3,3,4),(0.,0.125,0.1875,0.25,
0.3125,0.375,0.5,0.625,0.6875,0.75,0.8125,0.875,1.),.UNSPECIFIED.);
#361=B_SPLINE_CURVE_WITH_KNOTS('',3,(#25689,#25690,#25691,#25692,#25693,
#25694,#25695,#25696,#25697,#25698,#25699,#25700,#25701),.UNSPECIFIED.,
 .F.,.F.,(4,3,3,3,4),(0.,0.393665259181331,0.5,0.894848401742748,0.999999577588646),
 .UNSPECIFIED.);
#362=B_SPLINE_CURVE_WITH_KNOTS('',3,(#25702,#25703,#25704,#25705,#25706,
#25707,#25708,#25709,#25710,#25711,#25712,#25713,#25714),.UNSPECIFIED.,
 .F.,.F.,(4,3,3,3,4),(4.22403003312878E-7,0.394848747914453,0.5,0.89366522956997,
1.),.UNSPECIFIED.);
#363=B_SPLINE_CURVE_WITH_KNOTS('',3,(#25716,#25717,#25718,#25719,#25720,
#25721,#25722,#25723,#25724,#25725,#25726,#25727,#25728),.UNSPECIFIED.,
 .F.,.F.,(4,3,3,3,4),(0.,0.39366525918135,0.5,0.894848401747474,0.999999577588569),
 .UNSPECIFIED.);
#364=B_SPLINE_CURVE_WITH_KNOTS('',3,(#25730,#25731,#25732,#25733,#25734,
#25735,#25736,#25737,#25738,#25739,#25740,#25741,#25742),.UNSPECIFIED.,
 .F.,.F.,(4,3,3,3,4),(4.22402912852314E-7,0.394848747910699,0.5,0.893665229570505,
1.),.UNSPECIFIED.);
#365=B_SPLINE_CURVE_WITH_KNOTS('',3,(#26003,#26004,#26005,#26006),
 .UNSPECIFIED.,.F.,.F.,(4,4),(0.668250521172189,0.843615509259931),
 .UNSPECIFIED.);
#366=B_SPLINE_CURVE_WITH_KNOTS('',3,(#26008,#26009,#26010,#26011,#26012,
#26013,#26014,#26015,#26016,#26017,#26018,#26019,#26020,#26021,#26022,#26023,
#26024,#26025,#26026),.UNSPECIFIED.,.F.,.F.,(4,3,3,3,3,3,4),(0.0111833063008374,
0.0121008630969431,0.0122880406507484,0.0132009415603016,0.0135642406067081,
0.0154010984870185,0.0176012552434354),.UNSPECIFIED.);
#367=B_SPLINE_CURVE_WITH_KNOTS('',3,(#26028,#26029,#26030,#26031,#26032,
#26033,#26034,#26035,#26036,#26037,#26038,#26039,#26040,#26041,#26042,#26043,
#26044,#26045,#26046,#26047,#26048,#26049,#26050,#26051,#26052,#26053,#26054,
#26055),.UNSPECIFIED.,.F.,.F.,(4,3,3,3,3,3,3,3,3,4),(1.06517613933674E-8,
0.0625,0.125,0.15625,0.1875,0.25,0.375,0.5,0.75,0.99999998854857),
 .UNSPECIFIED.);
#368=B_SPLINE_CURVE_WITH_KNOTS('',3,(#26057,#26058,#26059,#26060,#26061,
#26062,#26063),.UNSPECIFIED.,.F.,.F.,(4,1,1,1,4),(2.92983445734476E-17,
0.00266695458268161,0.00533390916536319,0.00800086374804478,0.0106678183307264),
 .UNSPECIFIED.);
#369=B_SPLINE_CURVE_WITH_KNOTS('',3,(#26065,#26066,#26067,#26068),
 .UNSPECIFIED.,.F.,.F.,(4,4),(0.102324395314902,0.960851822466372),
 .UNSPECIFIED.);
#370=B_SPLINE_CURVE_WITH_KNOTS('',3,(#26070,#26071,#26072,#26073,#26074,
#26075,#26076,#26077,#26078,#26079,#26080,#26081,#26082,#26083,#26084,#26085,
#26086,#26087,#26088,#26089,#26090,#26091),.UNSPECIFIED.,.F.,.F.,(4,3,3,
3,3,3,3,4),(0.0158713903754465,0.0168306242499723,0.0187006936110803,0.0205707629721883,
0.0224303222343527,0.0224408323332963,0.0261809710555123,0.0299211047587188),
 .UNSPECIFIED.);
#371=B_SPLINE_CURVE_WITH_KNOTS('',1,(#26159,#26160),.UNSPECIFIED.,.F.,.F.,
(2,2),(-0.843561641779046,-0.803664345351663),.UNSPECIFIED.);
#372=B_SPLINE_CURVE_WITH_KNOTS('',3,(#26162,#26163,#26164,#26165),
 .UNSPECIFIED.,.F.,.F.,(4,4),(0.,0.0677982128913682),.UNSPECIFIED.);
#373=B_SPLINE_CURVE_WITH_KNOTS('',3,(#26167,#26168,#26169,#26170,#26171,
#26172,#26173,#26174,#26175,#26176,#26177,#26178,#26179,#26180,#26181,#26182,
#26183,#26184,#26185,#26186,#26187,#26188,#26189,#26190,#26191,#26192,#26193,
#26194,#26195,#26196,#26197,#26198,#26199,#26200,#26201,#26202,#26203,#26204,
#26205,#26206,#26207,#26208,#26209,#26210,#26211,#26212,#26213,#26214,#26215,
#26216,#26217,#26218,#26219,#26220,#26221,#26222,#26223,#26224,#26225,#26226,
#26227,#26228,#26229,#26230,#26231,#26232,#26233,#26234,#26235,#26236,#26237,
#26238,#26239,#26240,#26241,#26242,#26243,#26244,#26245,#26246,#26247,#26248,
#26249,#26250,#26251,#26252,#26253,#26254,#26255,#26256,#26257,#26258,#26259,
#26260,#26261,#26262,#26263,#26264,#26265,#26266,#26267,#26268,#26269,#26270,
#26271,#26272,#26273,#26274,#26275,#26276,#26277,#26278,#26279,#26280,#26281,
#26282,#26283,#26284,#26285,#26286,#26287,#26288,#26289,#26290,#26291,#26292,
#26293,#26294,#26295,#26296,#26297,#26298,#26299,#26300,#26301,#26302,#26303,
#26304,#26305,#26306,#26307,#26308,#26309,#26310,#26311,#26312,#26313,#26314,
#26315,#26316,#26317,#26318,#26319,#26320,#26321,#26322,#26323,#26324,#26325,
#26326,#26327,#26328,#26329,#26330,#26331,#26332,#26333,#26334,#26335,#26336,
#26337,#26338,#26339,#26340,#26341,#26342,#26343,#26344,#26345,#26346,#26347,
#26348,#26349,#26350),.UNSPECIFIED.,.F.,.F.,(4,3,3,3,3,3,3,3,3,3,3,3,3,
3,3,3,3,3,3,3,3,3,3,3,3,3,3,3,3,3,3,3,3,3,3,3,3,3,3,3,3,3,3,3,3,3,3,3,3,
3,3,3,3,3,3,3,3,3,3,3,3,4),(2.23112281381123E-7,0.03125,0.046875,0.0546875,
0.0625,0.0703125,0.078125,0.09375,0.109375,0.125,0.128101322996236,0.140625,
0.15625,0.171875,0.1875,0.203125,0.21875,0.234375,0.25,0.261882944458568,
0.265625,0.28125,0.3125,0.34375,0.359375,0.375,0.385783882951856,0.390625,
0.40625,0.4375,0.5,0.50039038538168,0.5625,0.59375,0.609375,0.614591279201434,
0.625,0.640625,0.65625,0.6875,0.71875,0.734375,0.73855596574661,0.75,0.765625,
0.78125,0.796875,0.8125,0.828125,0.84375,0.859375,0.872372445270951,0.875,
0.890625,0.90625,0.921875,0.9296875,0.9375,0.9453125,0.953125,0.96875,0.999999779165919),
 .UNSPECIFIED.);
#374=B_SPLINE_CURVE_WITH_KNOTS('',3,(#26352,#26353,#26354,#26355,#26356),
 .UNSPECIFIED.,.F.,.F.,(4,1,4),(0.,0.5,1.),.UNSPECIFIED.);
#375=B_SPLINE_CURVE_WITH_KNOTS('',3,(#26358,#26359,#26360,#26361,#26362,
#26363,#26364,#26365,#26366,#26367,#26368,#26369,#26370,#26371,#26372,#26373,
#26374,#26375,#26376,#26377,#26378,#26379,#26380,#26381,#26382,#26383,#26384,
#26385,#26386,#26387,#26388,#26389,#26390,#26391,#26392,#26393,#26394,#26395,
#26396,#26397,#26398,#26399,#26400,#26401,#26402,#26403,#26404,#26405,#26406,
#26407,#26408,#26409,#26410,#26411,#26412,#26413,#26414,#26415,#26416,#26417,
#26418,#26419,#26420,#26421,#26422,#26423,#26424,#26425,#26426,#26427,#26428,
#26429,#26430,#26431,#26432,#26433,#26434,#26435,#26436,#26437,#26438,#26439,
#26440,#26441,#26442,#26443,#26444,#26445,#26446,#26447,#26448,#26449,#26450,
#26451,#26452,#26453,#26454,#26455,#26456,#26457,#26458,#26459,#26460,#26461,
#26462,#26463,#26464,#26465,#26466,#26467,#26468,#26469,#26470,#26471,#26472,
#26473,#26474,#26475,#26476,#26477,#26478,#26479,#26480,#26481,#26482,#26483,
#26484,#26485,#26486,#26487,#26488,#26489,#26490,#26491,#26492,#26493,#26494,
#26495,#26496,#26497,#26498,#26499,#26500,#26501,#26502,#26503,#26504,#26505,
#26506,#26507,#26508,#26509,#26510,#26511,#26512,#26513,#26514,#26515,#26516,
#26517,#26518,#26519,#26520,#26521,#26522,#26523,#26524,#26525,#26526,#26527,
#26528,#26529,#26530,#26531,#26532,#26533,#26534,#26535,#26536,#26537,#26538,
#26539,#26540,#26541),.UNSPECIFIED.,.F.,.F.,(4,3,3,3,3,3,3,3,3,3,3,3,3,
3,3,3,3,3,3,3,3,3,3,3,3,3,3,3,3,3,3,3,3,3,3,3,3,3,3,3,3,3,3,3,3,3,3,3,3,
3,3,3,3,3,3,3,3,3,3,3,3,4),(2.23106010072049E-7,0.03125,0.046875,0.0546875,
0.0625,0.0703125,0.078125,0.09375,0.109375,0.125,0.128101110916128,0.140625,
0.15625,0.171875,0.1875,0.203125,0.21875,0.234375,0.25,0.261882369249052,
0.265625,0.28125,0.3125,0.34375,0.359375,0.375,0.385783798958653,0.390625,
0.40625,0.4375,0.5,0.500390522344446,0.5625,0.59375,0.609375,0.614591477860909,
0.625,0.640625,0.65625,0.6875,0.71875,0.734375,0.738556592284746,0.75,0.765625,
0.78125,0.796875,0.8125,0.828125,0.84375,0.859375,0.872372659350468,0.875,
0.890625,0.90625,0.921875,0.9296875,0.9375,0.9453125,0.953125,0.96875,0.999999779172077),
 .UNSPECIFIED.);
#376=B_SPLINE_CURVE_WITH_KNOTS('',3,(#26543,#26544,#26545,#26546),
 .UNSPECIFIED.,.F.,.F.,(4,4),(0.499948130219197,1.),.UNSPECIFIED.);
#377=B_SPLINE_CURVE_WITH_KNOTS('',1,(#26548,#26549),.UNSPECIFIED.,.F.,.F.,
(2,2),(-0.831634677873798,-0.786894219517676),.UNSPECIFIED.);
#378=B_SPLINE_CURVE_WITH_KNOTS('',3,(#26551,#26552,#26553,#26554,#26555,
#26556,#26557,#26558,#26559,#26560,#26561,#26562,#26563,#26564,#26565,#26566,
#26567,#26568,#26569,#26570,#26571,#26572,#26573,#26574,#26575,#26576,#26577,
#26578,#26579,#26580,#26581,#26582,#26583,#26584,#26585,#26586,#26587,#26588,
#26589),.UNSPECIFIED.,.F.,.F.,(4,1,1,1,1,1,1,1,1,1,1,1,1,1,1,1,1,1,1,1,
1,1,1,1,1,1,1,1,1,1,1,1,1,1,1,1,4),(0.,0.015625,0.03125,0.046875,0.0625,
0.09375,0.125,0.15625,0.1875,0.25,0.28125,0.296875,0.3125,0.328125,0.34375,
0.359375,0.3671875,0.37109375,0.375,0.37890625,0.3828125,0.390625,0.3984375,
0.40625,0.4140625,0.421875,0.4296875,0.4375,0.4453125,0.453125,0.46875,
0.484375,0.5,0.515625,0.53125,0.5625,0.625),.UNSPECIFIED.);
#379=B_SPLINE_CURVE_WITH_KNOTS('',3,(#26591,#26592,#26593,#26594,#26595,
#26596,#26597,#26598,#26599,#26600,#26601,#26602,#26603,#26604,#26605,#26606,
#26607,#26608,#26609,#26610,#26611,#26612),.UNSPECIFIED.,.F.,.F.,(4,1,1,
1,1,1,1,1,1,1,1,1,1,1,1,1,1,1,1,4),(0.625,0.6875,0.71875,0.75,0.78125,0.796875,
0.8125,0.828125,0.84375,0.859375,0.875,0.890625,0.90625,0.921875,0.9296875,
0.9375,0.9453125,0.953125,0.96875,1.),.UNSPECIFIED.);
#380=B_SPLINE_CURVE_WITH_KNOTS('',3,(#26614,#26615,#26616,#26617,#26618,
#26619,#26620,#26621,#26622,#26623,#26624,#26625,#26626,#26627,#26628,#26629,
#26630,#26631,#26632,#26633,#26634,#26635,#26636,#26637,#26638,#26639,#26640,
#26641,#26642,#26643,#26644,#26645,#26646,#26647,#26648,#26649,#26650,#26651,
#26652,#26653,#26654,#26655,#26656,#26657,#26658,#26659,#26660,#26661,#26662,
#26663,#26664,#26665,#26666,#26667,#26668,#26669,#26670,#26671,#26672,#26673,
#26674,#26675,#26676,#26677),.UNSPECIFIED.,.F.,.F.,(4,1,1,1,1,1,1,1,1,1,
1,1,1,1,1,1,1,1,1,1,1,1,1,1,1,1,1,1,1,1,1,1,1,1,1,1,1,1,1,1,1,1,1,1,1,1,
1,1,1,1,1,1,1,1,1,1,1,1,1,1,1,4),(1.77187976368624E-6,0.03125,0.046875,
0.0546875,0.0625,0.0703125,0.078125,0.09375,0.109375,0.125,0.140625,0.15625,
0.171875,0.1875,0.203125,0.21875,0.234375,0.25,0.265625,0.28125,0.3125,
0.375,0.40625,0.4375,0.46875,0.484375,0.5,0.515625,0.53125,0.546875,0.5546875,
0.5625,0.5703125,0.578125,0.59375,0.6015625,0.609375,0.6171875,0.62109375,
0.625,0.62890625,0.6328125,0.640625,0.65625,0.671875,0.6875,0.703125,0.71875,
0.75,0.8125,0.84375,0.859375,0.875,0.90625,0.921875,0.9375,0.953125,0.9609375,
0.96875,0.9765625,0.984375,0.999999998713145),.UNSPECIFIED.);
#381=B_SPLINE_CURVE_WITH_KNOTS('',3,(#26679,#26680,#26681,#26682,#26683,
#26684,#26685,#26686,#26687,#26688,#26689,#26690),.UNSPECIFIED.,.F.,.F.,
(4,1,1,1,1,1,1,1,1,4),(0.,0.015625,0.0234375,0.03125,0.0390625,0.046875,
0.0625,0.078125,0.09375,0.124710011167853),.UNSPECIFIED.);
#382=B_SPLINE_CURVE_WITH_KNOTS('',3,(#26692,#26693,#26694,#26695,#26696,
#26697,#26698,#26699,#26700,#26701,#26702,#26703,#26704,#26705,#26706,#26707,
#26708,#26709,#26710,#26711,#26712,#26713,#26714,#26715,#26716,#26717,#26718,
#26719,#26720,#26721,#26722,#26723,#26724,#26725,#26726,#26727,#26728,#26729,
#26730,#26731),.UNSPECIFIED.,.F.,.F.,(4,1,1,1,1,1,1,1,1,1,1,1,1,1,1,1,1,
1,1,1,1,1,1,1,1,1,1,1,1,1,1,1,1,1,1,1,1,4),(0.124710011167853,0.125,0.15625,
0.1875,0.21875,0.25,0.28125,0.296875,0.3125,0.328125,0.34375,0.359375,0.3671875,
0.375,0.3828125,0.390625,0.40625,0.4140625,0.421875,0.4296875,0.43359375,
0.4375,0.44140625,0.4453125,0.453125,0.4609375,0.46875,0.484375,0.5,0.515625,
0.53125,0.5625,0.59375,0.625,0.6875,0.71875,0.75,0.756387532860041),
 .UNSPECIFIED.);
#383=B_SPLINE_CURVE_WITH_KNOTS('',3,(#26733,#26734,#26735,#26736,#26737,
#26738,#26739,#26740,#26741,#26742,#26743,#26744,#26745,#26746,#26747,#26748,
#26749,#26750,#26751),.UNSPECIFIED.,.F.,.F.,(4,1,1,1,1,1,1,1,1,1,1,1,1,
1,1,1,4),(0.756387532860041,0.78125,0.796875,0.8125,0.828125,0.84375,0.859375,
0.875,0.890625,0.90625,0.921875,0.9296875,0.9375,0.9453125,0.953125,0.96875,
1.),.UNSPECIFIED.);
#384=B_SPLINE_CURVE_WITH_KNOTS('',3,(#26752,#26753,#26754,#26755,#26756,
#26757,#26758,#26759,#26760,#26761,#26762,#26763,#26764,#26765,#26766,#26767,
#26768,#26769,#26770,#26771,#26772,#26773,#26774,#26775,#26776,#26777,#26778,
#26779,#26780,#26781,#26782,#26783,#26784,#26785,#26786,#26787,#26788,#26789,
#26790,#26791,#26792,#26793,#26794,#26795,#26796,#26797,#26798,#26799,#26800),
 .UNSPECIFIED.,.F.,.F.,(4,1,1,1,1,1,1,1,1,1,1,1,1,1,1,1,1,1,1,1,1,1,1,1,
1,1,1,1,1,1,1,1,1,1,1,1,1,1,1,1,1,1,1,1,1,1,4),(5.26782351439448E-6,0.03125,
0.0625,0.09375,0.109375,0.125,0.140625,0.15625,0.171875,0.1875,0.203125,
0.21875,0.25,0.28125,0.3125,0.375,0.40625,0.4375,0.46875,0.484375,0.5,0.515625,
0.5234375,0.53125,0.5390625,0.546875,0.5546875,0.55859375,0.5625,0.56640625,
0.5703125,0.578125,0.5859375,0.59375,0.609375,0.6171875,0.625,0.6328125,
0.640625,0.65625,0.671875,0.6875,0.703125,0.71875,0.75,0.8125,0.867768400737492),
 .UNSPECIFIED.);
#385=B_SPLINE_CURVE_WITH_KNOTS('',1,(#26869,#26870),.UNSPECIFIED.,.F.,.F.,
(2,2),(-0.762686810518316,-0.668179912465779),.UNSPECIFIED.);
#386=B_SPLINE_CURVE_WITH_KNOTS('',3,(#26872,#26873,#26874,#26875,#26876,
#26877,#26878,#26879,#26880,#26881,#26882,#26883,#26884,#26885,#26886,#26887,
#26888,#26889,#26890,#26891,#26892,#26893,#26894,#26895,#26896,#26897,#26898,
#26899,#26900,#26901,#26902,#26903,#26904,#26905,#26906,#26907,#26908,#26909,
#26910,#26911,#26912,#26913),.UNSPECIFIED.,.F.,.F.,(4,1,1,1,1,1,1,1,1,1,
1,1,1,1,1,1,1,1,1,1,1,1,1,1,1,1,1,1,1,1,1,1,1,1,1,1,1,1,1,4),(0.142413158676735,
0.1875,0.25,0.3125,0.34375,0.375,0.40625,0.4375,0.46875,0.484375,0.5,0.515625,
0.53125,0.5625,0.578125,0.59375,0.609375,0.625,0.640625,0.65625,0.671875,
0.6875,0.703125,0.71875,0.75,0.765625,0.78125,0.796875,0.8125,0.828125,
0.84375,0.859375,0.875,0.890625,0.90625,0.921875,0.9375,0.953125,0.96875,
1.),.UNSPECIFIED.);
#387=B_SPLINE_CURVE_WITH_KNOTS('',3,(#26915,#26916,#26917,#26918,#26919,
#26920,#26921,#26922,#26923,#26924,#26925,#26926,#26927,#26928,#26929,#26930,
#26931,#26932,#26933,#26934,#26935,#26936,#26937,#26938,#26939,#26940,#26941,
#26942),.UNSPECIFIED.,.F.,.F.,(4,3,3,3,3,3,3,3,3,4),(0.,0.0625,0.125,0.1875,
0.25,0.3125,0.375,0.4375,0.475532550545482,0.483433722321772),
 .UNSPECIFIED.);
#388=B_SPLINE_CURVE_WITH_KNOTS('',3,(#26944,#26945,#26946,#26947,#26948,
#26949,#26950,#26951,#26952,#26953,#26954,#26955,#26956,#26957,#26958,#26959,
#26960,#26961,#26962,#26963,#26964,#26965,#26966,#26967,#26968,#26969,#26970,
#26971,#26972,#26973,#26974,#26975,#26976,#26977),.UNSPECIFIED.,.F.,.F.,
(4,3,3,3,3,3,3,3,3,3,3,4),(0.483433722321772,0.5,0.5625,0.625,0.6875,0.75,
0.8125,0.84375,0.875,0.90625,0.9375,0.999990394166022),.UNSPECIFIED.);
#389=B_SPLINE_CURVE_WITH_KNOTS('',3,(#26979,#26980,#26981,#26982,#26983,
#26984,#26985,#26986,#26987,#26988,#26989,#26990,#26991,#26992,#26993,#26994,
#26995,#26996,#26997,#26998,#26999,#27000,#27001,#27002,#27003),
 .UNSPECIFIED.,.F.,.F.,(4,3,3,3,3,3,3,3,4),(3.51665398735729E-9,0.125,0.25,
0.375,0.5,0.5625,0.625,0.75,0.99894251312119),.UNSPECIFIED.);
#390=B_SPLINE_CURVE_WITH_KNOTS('',3,(#27009,#27010,#27011,#27012,#27013,
#27014,#27015,#27016,#27017,#27018),.UNSPECIFIED.,.F.,.F.,(4,3,3,4),(0.,
0.25,0.5,1.),.UNSPECIFIED.);
#391=B_SPLINE_CURVE_WITH_KNOTS('',3,(#27020,#27021,#27022,#27023,#27024,
#27025,#27026),.UNSPECIFIED.,.F.,.F.,(4,3,4),(0.0269518367147259,0.5,1.),
 .UNSPECIFIED.);
#392=B_SPLINE_CURVE_WITH_KNOTS('',3,(#27028,#27029,#27030,#27031),
 .UNSPECIFIED.,.F.,.F.,(4,4),(0.,0.0269518367147259),.UNSPECIFIED.);
#393=B_SPLINE_CURVE_WITH_KNOTS('',3,(#27033,#27034,#27035,#27036,#27037,
#27038,#27039,#27040,#27041,#27042,#27043,#27044,#27045,#27046,#27047,#27048,
#27049,#27050,#27051,#27052,#27053,#27054,#27055,#27056,#27057,#27058,#27059,
#27060),.UNSPECIFIED.,.F.,.F.,(4,3,3,3,3,3,3,3,3,4),(0.,0.25,0.375,0.5,
0.5625,0.625,0.6875,0.75,0.875,1.),.UNSPECIFIED.);
#394=B_SPLINE_CURVE_WITH_KNOTS('',3,(#27062,#27063,#27064,#27065,#27066,
#27067,#27068,#27069,#27070,#27071,#27072,#27073,#27074),.UNSPECIFIED.,
 .F.,.F.,(4,3,3,3,4),(0.,0.125,0.25,0.270263701077272,0.364903448065341),
 .UNSPECIFIED.);
#395=B_SPLINE_CURVE_WITH_KNOTS('',3,(#27076,#27077,#27078,#27079,#27080,
#27081,#27082,#27083,#27084,#27085,#27086,#27087,#27088,#27089,#27090,#27091,
#27092,#27093,#27094,#27095,#27096,#27097),.UNSPECIFIED.,.F.,.F.,(4,3,3,
3,3,3,3,4),(0.364903448065341,0.5,0.625,0.6875,0.75,0.8125,0.875,1.),
 .UNSPECIFIED.);
#396=B_SPLINE_CURVE_WITH_KNOTS('',3,(#27099,#27100,#27101,#27102,#27103,
#27104,#27105,#27106,#27107,#27108,#27109,#27110,#27111,#27112,#27113,#27114),
 .UNSPECIFIED.,.F.,.F.,(4,3,3,3,3,4),(8.50485119671489E-5,0.125,0.1875,
0.25,0.3125,0.339613136872108),.UNSPECIFIED.);
#397=B_SPLINE_CURVE_WITH_KNOTS('',1,(#27116,#27117),.UNSPECIFIED.,.F.,.F.,
(2,2),(-0.747935545358406,-0.734608691980728),.UNSPECIFIED.);
#398=B_SPLINE_CURVE_WITH_KNOTS('',3,(#27119,#27120,#27121,#27122,#27123,
#27124,#27125,#27126,#27127,#27128),.UNSPECIFIED.,.F.,.F.,(4,1,1,1,1,1,
1,4),(0.742143863244383,0.75,0.8125,0.84375,0.875,0.90625,0.9375,1.),
 .UNSPECIFIED.);
#399=B_SPLINE_CURVE_WITH_KNOTS('',3,(#27130,#27131,#27132,#27133,#27134,
#27135,#27136,#27137,#27138,#27139,#27140),.UNSPECIFIED.,.F.,.F.,(4,1,1,
1,1,1,1,1,4),(2.19745662600075E-7,0.0625,0.09375,0.125,0.15625,0.1875,0.25,
0.375,0.499885453205276),.UNSPECIFIED.);
#400=B_SPLINE_CURVE_WITH_KNOTS('',3,(#27142,#27143,#27144,#27145,#27146,
#27147,#27148,#27149,#27150,#27151,#27152,#27153),.UNSPECIFIED.,.F.,.F.,
(4,1,1,1,1,1,1,1,1,4),(0.5,0.625,0.6875,0.75,0.8125,0.84375,0.875,0.90625,
0.9375,0.999977328601928),.UNSPECIFIED.);
#401=B_SPLINE_CURVE_WITH_KNOTS('',3,(#27157,#27158,#27159,#27160,#27161,
#27162,#27163,#27164,#27165,#27166,#27167,#27168),.UNSPECIFIED.,.F.,.F.,
(4,1,1,1,1,1,1,1,1,4),(0.,0.0625,0.09375,0.125,0.15625,0.1875,0.25,0.3125,
0.375,0.5),.UNSPECIFIED.);
#402=B_SPLINE_CURVE_WITH_KNOTS('',3,(#27170,#27171,#27172,#27173,#27174,
#27175,#27176,#27177,#27178,#27179,#27180),.UNSPECIFIED.,.F.,.F.,(4,1,1,
1,1,1,1,1,4),(0.5,0.625,0.75,0.8125,0.84375,0.875,0.90625,0.9375,1.),
 .UNSPECIFIED.);
#403=B_SPLINE_CURVE_WITH_KNOTS('',3,(#27182,#27183,#27184,#27185,#27186,
#27187,#27188,#27189,#27190,#27191),.UNSPECIFIED.,.F.,.F.,(4,1,1,1,1,1,
1,4),(7.21673521508086E-6,0.0625,0.09375,0.125,0.15625,0.1875,0.25,0.257506245398161),
 .UNSPECIFIED.);
#404=B_SPLINE_CURVE_WITH_KNOTS('',1,(#27193,#27194),.UNSPECIFIED.,.F.,.F.,
(2,2),(-0.714609893047583,-0.701287175823169),.UNSPECIFIED.);
#405=B_SPLINE_CURVE_WITH_KNOTS('',3,(#27196,#27197,#27198,#27199,#27200,
#27201,#27202,#27203,#27204,#27205),.UNSPECIFIED.,.F.,.F.,(4,1,1,1,1,1,
1,4),(0.742719765959379,0.75,0.8125,0.84375,0.875,0.90625,0.9375,1.),
 .UNSPECIFIED.);
#406=B_SPLINE_CURVE_WITH_KNOTS('',3,(#27207,#27208,#27209,#27210,#27211,
#27212,#27213,#27214,#27215,#27216,#27217),.UNSPECIFIED.,.F.,.F.,(4,1,1,
1,1,1,1,1,4),(2.44735148634498E-7,0.0625,0.09375,0.125,0.15625,0.1875,0.25,
0.375,0.499888365983082),.UNSPECIFIED.);
#407=B_SPLINE_CURVE_WITH_KNOTS('',3,(#27219,#27220,#27221,#27222,#27223,
#27224,#27225,#27226,#27227,#27228,#27229,#27230),.UNSPECIFIED.,.F.,.F.,
(4,1,1,1,1,1,1,1,1,4),(0.5,0.625,0.6875,0.75,0.8125,0.84375,0.875,0.90625,
0.9375,1.),.UNSPECIFIED.);
#408=B_SPLINE_CURVE_WITH_KNOTS('',3,(#27234,#27235,#27236,#27237,#27238,
#27239,#27240,#27241,#27242,#27243,#27244,#27245),.UNSPECIFIED.,.F.,.F.,
(4,1,1,1,1,1,1,1,1,4),(0.,0.0625,0.09375,0.125,0.15625,0.1875,0.25,0.3125,
0.375,0.5),.UNSPECIFIED.);
#409=B_SPLINE_CURVE_WITH_KNOTS('',3,(#27247,#27248,#27249,#27250,#27251,
#27252,#27253,#27254,#27255,#27256,#27257),.UNSPECIFIED.,.F.,.F.,(4,1,1,
1,1,1,1,1,4),(0.5,0.625,0.75,0.8125,0.84375,0.875,0.90625,0.9375,1.),
 .UNSPECIFIED.);
#410=B_SPLINE_CURVE_WITH_KNOTS('',3,(#27259,#27260,#27261,#27262,#27263,
#27264,#27265,#27266,#27267,#27268),.UNSPECIFIED.,.F.,.F.,(4,1,1,1,1,1,
1,4),(6.46805633295331E-6,0.0625,0.09375,0.125,0.15625,0.1875,0.25,0.256944255797255),
 .UNSPECIFIED.);
#411=B_SPLINE_CURVE_WITH_KNOTS('',1,(#27270,#27271),.UNSPECIFIED.,.F.,.F.,
(2,2),(-0.681288387796028,-0.667963314640389),.UNSPECIFIED.);
#412=B_SPLINE_CURVE_WITH_KNOTS('',3,(#27273,#27274,#27275,#27276,#27277,
#27278,#27279,#27280,#27281,#27282),.UNSPECIFIED.,.F.,.F.,(4,1,1,1,1,1,
1,4),(0.743178274051315,0.75,0.8125,0.84375,0.875,0.90625,0.9375,1.),
 .UNSPECIFIED.);
#413=B_SPLINE_CURVE_WITH_KNOTS('',3,(#27284,#27285,#27286,#27287,#27288,
#27289,#27290,#27291,#27292,#27293,#27294),.UNSPECIFIED.,.F.,.F.,(4,1,1,
1,1,1,1,1,4),(1.8821041512382E-7,0.0625,0.09375,0.125,0.15625,0.1875,0.25,
0.375,0.499902076873613),.UNSPECIFIED.);
#414=B_SPLINE_CURVE_WITH_KNOTS('',3,(#27296,#27297,#27298,#27299,#27300,
#27301,#27302,#27303,#27304,#27305,#27306,#27307),.UNSPECIFIED.,.F.,.F.,
(4,1,1,1,1,1,1,1,1,4),(0.5,0.625,0.6875,0.75,0.8125,0.84375,0.875,0.90625,
0.9375,1.),.UNSPECIFIED.);
#415=B_SPLINE_CURVE_WITH_KNOTS('',3,(#27309,#27310,#27311,#27312,#27313,
#27314,#27315,#27316,#27317,#27318,#27319,#27320,#27321,#27322,#27323,#27324,
#27325,#27326,#27327,#27328,#27329,#27330,#27331,#27332,#27333,#27334,#27335,
#27336,#27337,#27338,#27339),.UNSPECIFIED.,.F.,.F.,(4,3,3,3,3,3,3,3,3,3,
4),(0.000195514036727322,0.0625,0.125,0.1875,0.25,0.375,0.5,0.625,0.75,
0.875,0.999997646068875),.UNSPECIFIED.);
#416=B_SPLINE_CURVE_WITH_KNOTS('',3,(#27341,#27342,#27343,#27344,#27345,
#27346,#27347,#27348,#27349,#27350,#27351,#27352,#27353),.UNSPECIFIED.,
 .F.,.F.,(4,1,1,1,1,1,1,1,1,1,4),(0.,0.0625,0.09375,0.125,0.15625,0.1875,
0.25,0.3125,0.375,0.5,0.500672802403104),.UNSPECIFIED.);
#417=B_SPLINE_CURVE_WITH_KNOTS('',3,(#27355,#27356,#27357,#27358,#27359,
#27360,#27361,#27362,#27363,#27364,#27365),.UNSPECIFIED.,.F.,.F.,(4,1,1,
1,1,1,1,1,4),(0.500672802403104,0.625,0.75,0.8125,0.84375,0.875,0.90625,
0.9375,0.999999779246756),.UNSPECIFIED.);
#418=B_SPLINE_CURVE_WITH_KNOTS('',3,(#27367,#27368,#27369,#27370,#27371,
#27372,#27373,#27374,#27375,#27376),.UNSPECIFIED.,.F.,.F.,(4,1,1,1,1,1,
1,4),(0.,0.0625,0.09375,0.125,0.15625,0.1875,0.25,0.271066582727647),
 .UNSPECIFIED.);
#419=B_SPLINE_CURVE_WITH_KNOTS('',1,(#27378,#27379),.UNSPECIFIED.,.F.,.F.,
(2,2),(-0.647962203600483,-0.634635368538325),.UNSPECIFIED.);
#420=B_SPLINE_CURVE_WITH_KNOTS('',3,(#27381,#27382,#27383,#27384,#27385,
#27386,#27387,#27388,#27389,#27390),.UNSPECIFIED.,.F.,.F.,(4,1,1,1,1,1,
1,4),(0.71355566892686,0.75,0.8125,0.84375,0.875,0.90625,0.9375,1.),
 .UNSPECIFIED.);
#421=B_SPLINE_CURVE_WITH_KNOTS('',3,(#27392,#27393,#27394,#27395),
 .UNSPECIFIED.,.F.,.F.,(4,4),(0.951039109725656,0.999996744713042),
 .UNSPECIFIED.);
#422=B_SPLINE_CURVE_WITH_KNOTS('',3,(#27397,#27398,#27399,#27400,#27401,
#27402,#27403,#27404,#27405,#27406,#27407,#27408,#27409,#27410,#27411,#27412,
#27413,#27414,#27415,#27416,#27417,#27418,#27419,#27420,#27421,#27422,#27423,
#27424),.UNSPECIFIED.,.F.,.F.,(4,3,3,3,3,3,3,3,3,4),(0.584078652551858,
0.59375,0.625,0.6875,0.71875,0.75,0.78125,0.8125,0.875,0.951039109725656),
 .UNSPECIFIED.);
#423=B_SPLINE_CURVE_WITH_KNOTS('',3,(#27426,#27427,#27428,#27429,#27430,
#27431,#27432,#27433,#27434,#27435,#27436,#27437,#27438,#27439,#27440,#27441,
#27442,#27443,#27444,#27445,#27446,#27447,#27448,#27449,#27450,#27451,#27452,
#27453,#27454,#27455,#27456,#27457,#27458,#27459,#27460,#27461,#27462,#27463,
#27464,#27465,#27466,#27467,#27468,#27469,#27470,#27471,#27472,#27473,#27474),
 .UNSPECIFIED.,.F.,.F.,(4,3,3,3,3,3,3,3,3,3,3,3,3,3,3,3,4),(0.125,0.15625,
0.1875,0.21875,0.25,0.3125,0.375,0.40625,0.434649092523259,0.4375,0.46875,
0.484375,0.5,0.515625,0.53125,0.5625,0.584078652551858),.UNSPECIFIED.);
#424=B_SPLINE_CURVE_WITH_KNOTS('',3,(#27476,#27477,#27478,#27479,#27480,
#27481,#27482),.UNSPECIFIED.,.F.,.F.,(4,3,4),(1.0214071444072E-5,0.0625,
0.125),.UNSPECIFIED.);
#425=B_SPLINE_CURVE_WITH_KNOTS('',3,(#27484,#27485,#27486,#27487,#27488,
#27489,#27490,#27491),.UNSPECIFIED.,.F.,.F.,(4,1,1,1,1,4),(7.73334121881107E-5,
0.0625,0.125,0.25,0.375,0.499602040488809),.UNSPECIFIED.);
#426=B_SPLINE_CURVE_WITH_KNOTS('',3,(#27493,#27494,#27495,#27496,#27497,
#27498,#27499),.UNSPECIFIED.,.F.,.F.,(4,1,1,1,4),(0.5,0.625,0.75,0.875,
0.999994675291189),.UNSPECIFIED.);
#427=B_SPLINE_CURVE_WITH_KNOTS('',3,(#27501,#27502,#27503,#27504,#27505,
#27506,#27507,#27508,#27509,#27510,#27511,#27512,#27513,#27514,#27515,#27516,
#27517,#27518,#27519,#27520,#27521,#27522,#27523,#27524,#27525,#27526,#27527,
#27528),.UNSPECIFIED.,.F.,.F.,(4,3,3,3,3,3,3,3,3,4),(0.,0.0625,0.09375,
0.125,0.15625,0.1875,0.25,0.375,0.5,0.500630475285163),.UNSPECIFIED.);
#428=B_SPLINE_CURVE_WITH_KNOTS('',3,(#27530,#27531,#27532,#27533,#27534,
#27535,#27536,#27537,#27538,#27539,#27540,#27541,#27542,#27543,#27544,#27545,
#27546,#27547,#27548,#27549,#27550,#27551,#27552,#27553,#27554),
 .UNSPECIFIED.,.F.,.F.,(4,3,3,3,3,3,3,3,4),(0.500630475285163,0.625,0.6875,
0.71875,0.75,0.78125,0.8125,0.875,0.999999745637335),.UNSPECIFIED.);
#429=B_SPLINE_CURVE_WITH_KNOTS('',3,(#27556,#27557,#27558,#27559,#27560,
#27561,#27562,#27563,#27564,#27565,#27566,#27567,#27568,#27569,#27570,#27571,
#27572,#27573,#27574),.UNSPECIFIED.,.F.,.F.,(4,3,3,3,3,3,4),(0.,0.125,0.1875,
0.21875,0.25,0.28125,0.295540353636982),.UNSPECIFIED.);
#430=B_SPLINE_CURVE_WITH_KNOTS('',1,(#27576,#27577),.UNSPECIFIED.,.F.,.F.,
(2,2),(-0.614701012907286,-0.601354554659112),.UNSPECIFIED.);
#431=B_SPLINE_CURVE_WITH_KNOTS('',3,(#27579,#27580,#27581,#27582,#27583,
#27584,#27585,#27586,#27587,#27588,#27589,#27590,#27591,#27592,#27593,#27594,
#27595,#27596,#27597),.UNSPECIFIED.,.F.,.F.,(4,3,3,3,3,3,4),(0.699974107082008,
0.71875,0.75,0.78125,0.8125,0.875,0.999999882359552),.UNSPECIFIED.);
#432=B_SPLINE_CURVE_WITH_KNOTS('',3,(#27599,#27600,#27601,#27602,#27603,
#27604,#27605,#27606,#27607,#27608,#27609,#27610,#27611,#27612,#27613,#27614,
#27615,#27616,#27617,#27618,#27619,#27620,#27621,#27622,#27623),
 .UNSPECIFIED.,.F.,.F.,(4,3,3,3,3,3,3,3,4),(0.,0.125,0.1875,0.21875,0.25,
0.28125,0.3125,0.375,0.5),.UNSPECIFIED.);
#433=B_SPLINE_CURVE_WITH_KNOTS('',3,(#27625,#27626,#27627,#27628,#27629,
#27630,#27631,#27632,#27633,#27634,#27635,#27636,#27637,#27638,#27639,#27640,
#27641,#27642,#27643,#27644,#27645,#27646,#27647,#27648,#27649,#27650,#27651,
#27652),.UNSPECIFIED.,.F.,.F.,(4,3,3,3,3,3,3,3,3,4),(0.5,0.625,0.636099191630217,
0.75,0.8125,0.84375,0.875,0.90625,0.9375,1.),.UNSPECIFIED.);
#434=B_SPLINE_CURVE_WITH_KNOTS('',3,(#27656,#27657,#27658,#27659,#27660,
#27661,#27662,#27663,#27664,#27665,#27666,#27667,#27668,#27669,#27670,#27671,
#27672,#27673,#27674),.UNSPECIFIED.,.F.,.F.,(4,1,1,1,1,1,1,1,1,1,1,1,1,
1,1,1,4),(0.,0.0625,0.09375,0.125,0.15625,0.1875,0.25,0.375,0.5,0.625,0.6875,
0.71875,0.75,0.78125,0.8125,0.875,0.9999997812994),.UNSPECIFIED.);
#435=B_SPLINE_CURVE_WITH_KNOTS('',3,(#27676,#27677,#27678,#27679,#27680,
#27681,#27682,#27683,#27684),.UNSPECIFIED.,.F.,.F.,(4,1,1,1,1,1,4),(0.,
0.125,0.1875,0.21875,0.25,0.28125,0.302671489156909),.UNSPECIFIED.);
#436=B_SPLINE_CURVE_WITH_KNOTS('',1,(#27686,#27687),.UNSPECIFIED.,.F.,.F.,
(2,2),(-0.581356766185651,-0.567943718980148),.UNSPECIFIED.);
#437=B_SPLINE_CURVE_WITH_KNOTS('',3,(#27689,#27690,#27691,#27692,#27693,
#27694,#27695,#27696,#27697,#27698,#27699,#27700,#27701,#27702,#27703,#27704,
#27705,#27706,#27707,#27708,#27709,#27710),.UNSPECIFIED.,.F.,.F.,(4,3,3,
3,3,3,3,4),(0.690961556714303,0.75,0.8125,0.84375,0.875,0.90625,0.9375,
1.),.UNSPECIFIED.);
#438=B_SPLINE_CURVE_WITH_KNOTS('',3,(#27712,#27713,#27714,#27715,#27716,
#27717,#27718,#27719,#27720,#27721,#27722,#27723,#27724,#27725,#27726,#27727,
#27728,#27729,#27730,#27731,#27732,#27733,#27734,#27735,#27736,#27737,#27738,
#27739,#27740,#27741,#27742,#27743,#27744,#27745,#27746,#27747,#27748,#27749,
#27750,#27751,#27752,#27753,#27754,#27755,#27756,#27757,#27758,#27759,#27760,
#27761,#27762,#27763,#27764,#27765,#27766,#27767,#27768,#27769),
 .UNSPECIFIED.,.F.,.F.,(4,3,3,3,3,3,3,3,3,3,3,3,3,3,3,3,3,3,3,4),(8.74756603760378E-8,
0.0625,0.09375,0.125,0.15625,0.1875,0.25,0.3125,0.375,0.5,0.625,0.653701494884754,
0.6875,0.75,0.8125,0.84375,0.875,0.90625,0.9375,0.999999836811042),
 .UNSPECIFIED.);
#439=B_SPLINE_CURVE_WITH_KNOTS('',3,(#27773,#27774,#27775,#27776,#27777,
#27778,#27779,#27780,#27781,#27782,#27783,#27784,#27785,#27786,#27787,#27788,
#27789,#27790,#27791,#27792,#27793),.UNSPECIFIED.,.F.,.F.,(4,1,1,1,1,1,
1,1,1,1,1,1,1,1,1,1,1,1,4),(2.76904502469975E-7,0.0625,0.09375,0.125,0.15625,
0.1875,0.25,0.3125,0.375,0.5,0.625,0.6875,0.75,0.8125,0.84375,0.875,0.90625,
0.9375,0.999999617215634),.UNSPECIFIED.);
#440=B_SPLINE_CURVE_WITH_KNOTS('',3,(#27795,#27796,#27797,#27798,#27799,
#27800,#27801,#27802,#27803,#27804),.UNSPECIFIED.,.F.,.F.,(4,1,1,1,1,1,
1,4),(0.,0.0625,0.09375,0.125,0.15625,0.1875,0.25,0.308404661026527),
 .UNSPECIFIED.);
#441=B_SPLINE_CURVE_WITH_KNOTS('',1,(#27806,#27807),.UNSPECIFIED.,.F.,.F.,
(2,2),(-0.547952025403732,-0.534632217745046),.UNSPECIFIED.);
#442=B_SPLINE_CURVE_WITH_KNOTS('',3,(#27809,#27810,#27811,#27812,#27813,
#27814,#27815,#27816,#27817,#27818,#27819,#27820,#27821,#27822,#27823,#27824,
#27825,#27826,#27827,#27828,#27829,#27830),.UNSPECIFIED.,.F.,.F.,(4,3,3,
3,3,3,3,4),(0.691764098829342,0.75,0.8125,0.84375,0.875,0.90625,0.9375,
1.),.UNSPECIFIED.);
#443=B_SPLINE_CURVE_WITH_KNOTS('',3,(#27832,#27833,#27834,#27835,#27836,
#27837,#27838,#27839,#27840,#27841,#27842,#27843,#27844,#27845,#27846,#27847,
#27848,#27849,#27850,#27851,#27852,#27853,#27854,#27855,#27856,#27857,#27858,
#27859,#27860,#27861,#27862,#27863,#27864,#27865,#27866,#27867,#27868,#27869,
#27870,#27871,#27872,#27873,#27874,#27875,#27876,#27877,#27878,#27879,#27880,
#27881,#27882,#27883,#27884,#27885,#27886,#27887,#27888,#27889),
 .UNSPECIFIED.,.F.,.F.,(4,3,3,3,3,3,3,3,3,3,3,3,3,3,3,3,3,3,3,4),(6.60130104707959E-8,
0.0625,0.09375,0.125,0.15625,0.1875,0.25,0.3125,0.375,0.5,0.625,0.651822706730315,
0.6875,0.75,0.8125,0.84375,0.875,0.90625,0.9375,0.999999831175229),
 .UNSPECIFIED.);
#444=B_SPLINE_CURVE_WITH_KNOTS('',3,(#27893,#27894,#27895,#27896,#27897,
#27898,#27899,#27900,#27901,#27902,#27903,#27904,#27905,#27906,#27907,#27908,
#27909,#27910,#27911,#27912,#27913),.UNSPECIFIED.,.F.,.F.,(4,1,1,1,1,1,
1,1,1,1,1,1,1,1,1,1,1,1,4),(2.85246569633639E-7,0.0625,0.09375,0.125,0.15625,
0.1875,0.25,0.3125,0.375,0.5,0.625,0.6875,0.75,0.8125,0.84375,0.875,0.90625,
0.9375,0.999999654885251),.UNSPECIFIED.);
#445=B_SPLINE_CURVE_WITH_KNOTS('',3,(#27915,#27916,#27917,#27918,#27919,
#27920,#27921,#27922,#27923,#27924),.UNSPECIFIED.,.F.,.F.,(4,1,1,1,1,1,
1,4),(0.,0.0625,0.09375,0.125,0.15625,0.1875,0.25,0.307485444826301),
 .UNSPECIFIED.);
#446=B_SPLINE_CURVE_WITH_KNOTS('',1,(#27926,#27927),.UNSPECIFIED.,.F.,.F.,
(2,2),(-0.514641034236103,-0.501321659607129),.UNSPECIFIED.);
#447=B_SPLINE_CURVE_WITH_KNOTS('',3,(#27929,#27930,#27931,#27932,#27933,
#27934,#27935,#27936,#27937,#27938),.UNSPECIFIED.,.F.,.F.,(4,1,1,1,1,1,
1,4),(0.692733007429323,0.75,0.8125,0.84375,0.875,0.90625,0.9375,1.),
 .UNSPECIFIED.);
#448=B_SPLINE_CURVE_WITH_KNOTS('',3,(#27940,#27941,#27942,#27943,#27944,
#27945,#27946,#27947,#27948,#27949,#27950,#27951,#27952,#27953,#27954,#27955,
#27956,#27957,#27958,#27959,#27960,#27961,#27962,#27963,#27964,#27965,#27966,
#27967,#27968,#27969,#27970,#27971,#27972,#27973,#27974,#27975,#27976,#27977,
#27978,#27979,#27980,#27981,#27982,#27983,#27984,#27985,#27986,#27987,#27988,
#27989,#27990,#27991,#27992,#27993,#27994,#27995,#27996,#27997),
 .UNSPECIFIED.,.F.,.F.,(4,3,3,3,3,3,3,3,3,3,3,3,3,3,3,3,3,3,3,4),(3.79295315668372E-8,
0.0625,0.09375,0.125,0.15625,0.1875,0.25,0.3125,0.375,0.5,0.625,0.64975298249665,
0.6875,0.75,0.8125,0.84375,0.875,0.90625,0.9375,0.999999823692408),
 .UNSPECIFIED.);
#449=B_SPLINE_CURVE_WITH_KNOTS('',3,(#28001,#28002,#28003,#28004,#28005,
#28006,#28007,#28008,#28009,#28010,#28011,#28012,#28013,#28014,#28015,#28016,
#28017,#28018,#28019,#28020,#28021),.UNSPECIFIED.,.F.,.F.,(4,1,1,1,1,1,
1,1,1,1,1,1,1,1,1,1,1,1,4),(2.85268618544073E-7,0.0625,0.09375,0.125,0.15625,
0.1875,0.25,0.3125,0.375,0.5,0.625,0.6875,0.75,0.8125,0.84375,0.875,0.90625,
0.9375,0.999999714317637),.UNSPECIFIED.);
#450=B_SPLINE_CURVE_WITH_KNOTS('',3,(#28023,#28024,#28025,#28026,#28027,
#28028,#28029,#28030,#28031,#28032),.UNSPECIFIED.,.F.,.F.,(4,1,1,1,1,1,
1,4),(0.,0.0625,0.09375,0.125,0.15625,0.1875,0.25,0.306675627321796),
 .UNSPECIFIED.);
#451=B_SPLINE_CURVE_WITH_KNOTS('',1,(#28034,#28035),.UNSPECIFIED.,.F.,.F.,
(2,2),(-0.481330907823224,-0.468014532967897),.UNSPECIFIED.);
#452=B_SPLINE_CURVE_WITH_KNOTS('',3,(#28037,#28038,#28039,#28040,#28041,
#28042,#28043,#28044,#28045,#28046),.UNSPECIFIED.,.F.,.F.,(4,1,1,1,1,1,
1,4),(0.693739351488113,0.75,0.8125,0.84375,0.875,0.90625,0.9375,1.),
 .UNSPECIFIED.);
#453=B_SPLINE_CURVE_WITH_KNOTS('',3,(#28048,#28049,#28050,#28051,#28052,
#28053,#28054,#28055,#28056,#28057,#28058,#28059,#28060,#28061,#28062,#28063,
#28064,#28065,#28066,#28067,#28068,#28069,#28070,#28071,#28072,#28073,#28074,
#28075,#28076,#28077,#28078,#28079,#28080,#28081,#28082,#28083,#28084,#28085,
#28086,#28087,#28088,#28089,#28090,#28091,#28092,#28093,#28094,#28095,#28096,
#28097,#28098,#28099,#28100,#28101,#28102,#28103,#28104,#28105),
 .UNSPECIFIED.,.F.,.F.,(4,3,3,3,3,3,3,3,3,3,3,3,3,3,3,3,3,3,3,4),(2.59941942783721E-8,
0.0625,0.09375,0.125,0.15625,0.1875,0.25,0.3125,0.375,0.5,0.625,0.647786928436969,
0.6875,0.75,0.8125,0.84375,0.875,0.90625,0.9375,0.999999815530093),
 .UNSPECIFIED.);
#454=B_SPLINE_CURVE_WITH_KNOTS('',3,(#28109,#28110,#28111,#28112,#28113,
#28114,#28115,#28116,#28117,#28118,#28119,#28120,#28121,#28122,#28123,#28124,
#28125,#28126,#28127,#28128,#28129),.UNSPECIFIED.,.F.,.F.,(4,1,1,1,1,1,
1,1,1,1,1,1,1,1,1,1,1,1,4),(2.82907565420154E-7,0.0625,0.09375,0.125,0.15625,
0.1875,0.25,0.3125,0.375,0.5,0.625,0.6875,0.75,0.8125,0.84375,0.875,0.90625,
0.9375,0.99999978184527),.UNSPECIFIED.);
#455=B_SPLINE_CURVE_WITH_KNOTS('',3,(#28131,#28132,#28133,#28134,#28135,
#28136,#28137,#28138,#28139,#28140),.UNSPECIFIED.,.F.,.F.,(4,1,1,1,1,1,
1,4),(0.,0.0625,0.09375,0.125,0.15625,0.1875,0.25,0.305513267453618),
 .UNSPECIFIED.);
#456=B_SPLINE_CURVE_WITH_KNOTS('',1,(#28142,#28143),.UNSPECIFIED.,.F.,.F.,
(2,2),(-0.448026172671341,-0.434710029955949),.UNSPECIFIED.);
#457=B_SPLINE_CURVE_WITH_KNOTS('',3,(#28145,#28146,#28147,#28148,#28149,
#28150,#28151,#28152,#28153,#28154),.UNSPECIFIED.,.F.,.F.,(4,1,1,1,1,1,
1,4),(0.69476673108169,0.75,0.8125,0.84375,0.875,0.90625,0.9375,1.),
 .UNSPECIFIED.);
#458=B_SPLINE_CURVE_WITH_KNOTS('',3,(#28156,#28157,#28158,#28159,#28160,
#28161,#28162,#28163,#28164,#28165,#28166,#28167,#28168,#28169,#28170,#28171,
#28172,#28173,#28174,#28175,#28176),.UNSPECIFIED.,.F.,.F.,(4,1,1,1,1,1,
1,1,1,1,1,1,1,1,1,1,1,1,4),(1.10928375193975E-8,0.0625,0.09375,0.125,0.15625,
0.1875,0.25,0.3125,0.375,0.5,0.625,0.6875,0.75,0.8125,0.84375,0.875,0.90625,
0.9375,0.999999806606368),.UNSPECIFIED.);
#459=B_SPLINE_CURVE_WITH_KNOTS('',3,(#28180,#28181,#28182,#28183,#28184,
#28185,#28186,#28187,#28188,#28189,#28190,#28191,#28192,#28193,#28194,#28195,
#28196,#28197,#28198,#28199,#28200),.UNSPECIFIED.,.F.,.F.,(4,1,1,1,1,1,
1,1,1,1,1,1,1,1,1,1,1,1,4),(2.78980747991976E-7,0.0625,0.09375,0.125,0.15625,
0.1875,0.25,0.3125,0.375,0.5,0.625,0.6875,0.75,0.8125,0.84375,0.875,0.90625,
0.9375,0.99999982218199),.UNSPECIFIED.);
#460=B_SPLINE_CURVE_WITH_KNOTS('',3,(#28202,#28203,#28204,#28205,#28206,
#28207,#28208,#28209,#28210,#28211),.UNSPECIFIED.,.F.,.F.,(4,1,1,1,1,1,
1,4),(0.,0.0625,0.09375,0.125,0.15625,0.1875,0.25,0.304441335563685),
 .UNSPECIFIED.);
#461=B_SPLINE_CURVE_WITH_KNOTS('',1,(#28213,#28214),.UNSPECIFIED.,.F.,.F.,
(2,2),(-0.414721936888564,-0.401409886337017),.UNSPECIFIED.);
#462=B_SPLINE_CURVE_WITH_KNOTS('',3,(#28216,#28217,#28218,#28219,#28220,
#28221,#28222,#28223,#28224,#28225,#28226,#28227,#28228,#28229,#28230,#28231),
 .UNSPECIFIED.,.F.,.F.,(4,3,3,3,3,4),(0.694959544378405,0.75,0.8125,0.84375,
0.875,0.999999985529887),.UNSPECIFIED.);
#463=B_SPLINE_CURVE_WITH_KNOTS('',3,(#28233,#28234,#28235,#28236,#28237,
#28238,#28239,#28240,#28241,#28242,#28243,#28244,#28245,#28246,#28247,#28248,
#28249,#28250,#28251,#28252,#28253),.UNSPECIFIED.,.F.,.F.,(4,1,1,1,1,1,
1,1,1,1,1,1,1,1,1,1,1,1,4),(0.,0.0625,0.09375,0.125,0.15625,0.1875,0.25,
0.3125,0.375,0.5,0.625,0.6875,0.75,0.8125,0.84375,0.875,0.90625,0.9375,
0.99999979724297),.UNSPECIFIED.);
#464=B_SPLINE_CURVE_WITH_KNOTS('',3,(#28257,#28258,#28259,#28260,#28261,
#28262),.UNSPECIFIED.,.F.,.F.,(4,2,4),(-0.386843013885963,-0.22816224008248,
-0.000106862707127469),.UNSPECIFIED.);
#465=B_SPLINE_CURVE_WITH_KNOTS('',3,(#28264,#28265,#28266,#28267,#28268,
#28269,#28270,#28271,#28272),.UNSPECIFIED.,.F.,.F.,(4,1,1,1,1,1,4),(0.,
0.125,0.1875,0.21875,0.25,0.28125,0.302853998408664),.UNSPECIFIED.);
#466=B_SPLINE_CURVE_WITH_KNOTS('',1,(#28274,#28275),.UNSPECIFIED.,.F.,.F.,
(2,2),(-0.38141833719901,-0.368114143248423),.UNSPECIFIED.);
#467=B_SPLINE_CURVE_WITH_KNOTS('',3,(#28277,#28278,#28279,#28280,#28281,
#28282,#28283,#28284,#28285,#28286,#28287,#28288,#28289,#28290,#28291,#28292,
#28293,#28294,#28295),.UNSPECIFIED.,.F.,.F.,(4,3,3,3,3,3,4),(0.697655525115426,
0.71875,0.75,0.78125,0.8125,0.875,1.),.UNSPECIFIED.);
#468=B_SPLINE_CURVE_WITH_KNOTS('',3,(#28297,#28298,#28299,#28300,#28301,
#28302,#28303,#28304,#28305,#28306,#28307,#28308,#28309,#28310,#28311,#28312,
#28313,#28314,#28315,#28316,#28317,#28318,#28319,#28320,#28321,#28322,#28323,
#28324,#28325,#28326,#28327,#28328,#28329,#28330,#28331,#28332,#28333,#28334,
#28335,#28336,#28337,#28338,#28339,#28340,#28341,#28342,#28343,#28344,#28345,
#28346,#28347,#28348),.UNSPECIFIED.,.F.,.F.,(4,3,3,3,3,3,3,3,3,3,3,3,3,
3,3,3,3,4),(3.40252582782886E-8,0.125,0.1875,0.21875,0.25,0.28125,0.3125,
0.375,0.5,0.625,0.641085058040362,0.75,0.8125,0.84375,0.875,0.90625,0.9375,
0.999999822300934),.UNSPECIFIED.);
#469=B_SPLINE_CURVE_WITH_KNOTS('',3,(#28352,#28353,#28354,#28355,#28356,
#28357,#28358,#28359,#28360,#28361,#28362,#28363,#28364,#28365,#28366,#28367,
#28368,#28369,#28370,#28371,#28372,#28373,#28374,#28375,#28376,#28377,#28378,
#28379,#28380,#28381,#28382,#28383,#28384,#28385,#28386,#28387,#28388,#28389,
#28390,#28391,#28392,#28393,#28394,#28395,#28396,#28397,#28398,#28399,#28400,
#28401,#28402,#28403),.UNSPECIFIED.,.F.,.F.,(4,3,3,3,3,3,3,3,3,3,3,3,3,
3,3,3,3,4),(0.,0.0625,0.09375,0.125,0.15625,0.1875,0.25,0.360119793928473,
0.375,0.5,0.625,0.6875,0.71875,0.75,0.78125,0.8125,0.875,1.),
 .UNSPECIFIED.);
#470=B_SPLINE_CURVE_WITH_KNOTS('',3,(#28405,#28406,#28407,#28408,#28409,
#28410,#28411,#28412,#28413),.UNSPECIFIED.,.F.,.F.,(4,1,1,1,1,1,4),(0.,
0.125,0.1875,0.21875,0.25,0.28125,0.301839172550323),.UNSPECIFIED.);
#471=B_SPLINE_CURVE_WITH_KNOTS('',1,(#28415,#28416),.UNSPECIFIED.,.F.,.F.,
(2,2),(-0.348122442733603,-0.334802618107589),.UNSPECIFIED.);
#472=B_SPLINE_CURVE_WITH_KNOTS('',3,(#28418,#28419,#28420,#28421,#28422,
#28423,#28424,#28425,#28426,#28427,#28428,#28429,#28430,#28431,#28432,#28433,
#28434,#28435,#28436),.UNSPECIFIED.,.F.,.F.,(4,3,3,3,3,3,4),(0.698643471576761,
0.71875,0.75,0.78125,0.8125,0.875,1.),.UNSPECIFIED.);
#473=B_SPLINE_CURVE_WITH_KNOTS('',3,(#28438,#28439,#28440,#28441,#28442,
#28443,#28444,#28445,#28446,#28447,#28448,#28449,#28450,#28451,#28452,#28453,
#28454,#28455,#28456,#28457,#28458,#28459,#28460,#28461,#28462,#28463,#28464,
#28465,#28466,#28467,#28468,#28469,#28470,#28471,#28472,#28473,#28474,#28475,
#28476,#28477,#28478,#28479,#28480,#28481,#28482,#28483,#28484,#28485,#28486,
#28487,#28488,#28489),.UNSPECIFIED.,.F.,.F.,(4,3,3,3,3,3,3,3,3,3,3,3,3,
3,3,3,3,4),(6.90927897239085E-8,0.125,0.1875,0.21875,0.25,0.28125,0.3125,
0.375,0.5,0.625,0.639344739454029,0.75,0.8125,0.84375,0.875,0.90625,0.9375,
0.999999825004712),.UNSPECIFIED.);
#474=B_SPLINE_CURVE_WITH_KNOTS('',3,(#28493,#28494,#28495,#28496,#28497,
#28498,#28499,#28500,#28501,#28502,#28503,#28504,#28505,#28506,#28507,#28508,
#28509,#28510,#28511,#28512,#28513,#28514,#28515,#28516,#28517,#28518,#28519,
#28520,#28521,#28522,#28523,#28524,#28525,#28526,#28527,#28528,#28529,#28530,
#28531,#28532,#28533,#28534,#28535,#28536,#28537,#28538,#28539,#28540,#28541,
#28542,#28543,#28544),.UNSPECIFIED.,.F.,.F.,(4,3,3,3,3,3,3,3,3,3,3,3,3,
3,3,3,3,4),(1.74218079178612E-7,0.0625,0.09375,0.125,0.15625,0.1875,0.25,
0.361910921352633,0.375,0.5,0.625,0.6875,0.71875,0.75,0.78125,0.8125,0.875,
1.),.UNSPECIFIED.);
#475=B_SPLINE_CURVE_WITH_KNOTS('',3,(#28546,#28547,#28548,#28549,#28550,
#28551,#28552,#28553,#28554),.UNSPECIFIED.,.F.,.F.,(4,1,1,1,1,1,4),(0.,
0.125,0.1875,0.21875,0.25,0.28125,0.300810905459472),.UNSPECIFIED.);
#476=B_SPLINE_CURVE_WITH_KNOTS('',1,(#28556,#28557),.UNSPECIFIED.,.F.,.F.,
(2,2),(-0.314810126318466,-0.30149018112365),.UNSPECIFIED.);
#477=B_SPLINE_CURVE_WITH_KNOTS('',3,(#28559,#28560,#28561,#28562,#28563,
#28564,#28565,#28566,#28567,#28568,#28569,#28570,#28571,#28572,#28573,#28574,
#28575,#28576,#28577),.UNSPECIFIED.,.F.,.F.,(4,3,3,3,3,3,4),(0.699678783356034,
0.71875,0.75,0.78125,0.8125,0.875,1.),.UNSPECIFIED.);
#478=B_SPLINE_CURVE_WITH_KNOTS('',3,(#28579,#28580,#28581,#28582,#28583,
#28584,#28585,#28586,#28587,#28588,#28589,#28590,#28591,#28592,#28593,#28594,
#28595,#28596,#28597,#28598,#28599,#28600,#28601,#28602,#28603,#28604,#28605,
#28606,#28607,#28608,#28609,#28610,#28611,#28612,#28613,#28614,#28615,#28616,
#28617,#28618,#28619,#28620,#28621,#28622,#28623,#28624,#28625,#28626,#28627,
#28628,#28629,#28630),.UNSPECIFIED.,.F.,.F.,(4,3,3,3,3,3,3,3,3,3,3,3,3,
3,3,3,3,4),(7.65381569237967E-8,0.125,0.1875,0.21875,0.25,0.28125,0.3125,
0.375,0.5,0.625,0.637564576525894,0.75,0.8125,0.84375,0.875,0.90625,0.9375,
0.999999824573213),.UNSPECIFIED.);
#479=B_SPLINE_CURVE_WITH_KNOTS('',3,(#28634,#28635,#28636,#28637,#28638,
#28639,#28640,#28641,#28642,#28643,#28644,#28645,#28646,#28647,#28648,#28649,
#28650,#28651,#28652),.UNSPECIFIED.,.F.,.F.,(4,1,1,1,1,1,1,1,1,1,1,1,1,
1,1,1,4),(2.68538809727287E-7,0.0625,0.09375,0.125,0.15625,0.1875,0.25,
0.375,0.5,0.625,0.6875,0.71875,0.75,0.78125,0.8125,0.875,1.),
 .UNSPECIFIED.);
#480=B_SPLINE_CURVE_WITH_KNOTS('',3,(#28654,#28655,#28656,#28657,#28658,
#28659,#28660,#28661,#28662),.UNSPECIFIED.,.F.,.F.,(4,1,1,1,1,1,4),(1.72862727219145E-8,
0.125,0.1875,0.21875,0.25,0.28125,0.299787333569703),.UNSPECIFIED.);
#481=B_SPLINE_CURVE_WITH_KNOTS('',1,(#28664,#28665),.UNSPECIFIED.,.F.,.F.,
(2,2),(-0.281497700229318,-0.268175969207313),.UNSPECIFIED.);
#482=B_SPLINE_CURVE_WITH_KNOTS('',3,(#28667,#28668,#28669,#28670,#28671,
#28672,#28673,#28674,#28675,#28676,#28677,#28678,#28679,#28680,#28681,#28682,
#28683,#28684,#28685),.UNSPECIFIED.,.F.,.F.,(4,3,3,3,3,3,4),(0.700679367798627,
0.71875,0.75,0.78125,0.8125,0.875,0.999999976169426),.UNSPECIFIED.);
#483=B_SPLINE_CURVE_WITH_KNOTS('',3,(#28687,#28688,#28689,#28690,#28691,
#28692,#28693,#28694,#28695,#28696,#28697,#28698,#28699,#28700,#28701,#28702,
#28703,#28704,#28705,#28706,#28707,#28708,#28709,#28710,#28711,#28712,#28713,
#28714,#28715,#28716,#28717,#28718,#28719,#28720,#28721,#28722,#28723,#28724,
#28725,#28726,#28727,#28728,#28729,#28730,#28731,#28732,#28733,#28734,#28735,
#28736,#28737,#28738),.UNSPECIFIED.,.F.,.F.,(4,3,3,3,3,3,3,3,3,3,3,3,3,
3,3,3,3,4),(0.,0.125,0.1875,0.21875,0.25,0.28125,0.3125,0.375,0.5,0.625,
0.635605727697318,0.75,0.8125,0.84375,0.875,0.90625,0.9375,0.999999821937738),
 .UNSPECIFIED.);
#484=B_SPLINE_CURVE_WITH_KNOTS('',3,(#28742,#28743,#28744,#28745,#28746,
#28747,#28748,#28749,#28750,#28751,#28752,#28753,#28754,#28755,#28756,#28757,
#28758,#28759,#28760),.UNSPECIFIED.,.F.,.F.,(4,1,1,1,1,1,1,1,1,1,1,1,1,
1,1,1,4),(0.,0.0625,0.09375,0.125,0.15625,0.1875,0.25,0.375,0.5,0.625,0.6875,
0.71875,0.75,0.78125,0.8125,0.875,1.),.UNSPECIFIED.);
#485=B_SPLINE_CURVE_WITH_KNOTS('',3,(#28762,#28763,#28764,#28765,#28766,
#28767,#28768,#28769,#28770),.UNSPECIFIED.,.F.,.F.,(4,1,1,1,1,1,4),(4.65545680163139E-9,
0.125,0.1875,0.21875,0.25,0.28125,0.298831604432797),.UNSPECIFIED.);
#486=B_SPLINE_CURVE_WITH_KNOTS('',1,(#28772,#28773),.UNSPECIFIED.,.F.,.F.,
(2,2),(-0.24818047819294,-0.234857897987038),.UNSPECIFIED.);
#487=B_SPLINE_CURVE_WITH_KNOTS('',3,(#28775,#28776,#28777,#28778,#28779,
#28780,#28781,#28782,#28783,#28784,#28785,#28786,#28787,#28788,#28789,#28790,
#28791,#28792,#28793),.UNSPECIFIED.,.F.,.F.,(4,3,3,3,3,3,4),(0.701590233395244,
0.71875,0.75,0.78125,0.8125,0.875,0.99999997963134),.UNSPECIFIED.);
#488=B_SPLINE_CURVE_WITH_KNOTS('',3,(#28795,#28796,#28797,#28798,#28799,
#28800,#28801,#28802,#28803,#28804,#28805,#28806,#28807,#28808,#28809,#28810,
#28811,#28812,#28813,#28814,#28815,#28816,#28817,#28818,#28819,#28820,#28821,
#28822,#28823,#28824,#28825,#28826,#28827,#28828,#28829,#28830,#28831,#28832,
#28833,#28834,#28835,#28836,#28837,#28838,#28839,#28840,#28841,#28842,#28843,
#28844,#28845,#28846),.UNSPECIFIED.,.F.,.F.,(4,3,3,3,3,3,3,3,3,3,3,3,3,
3,3,3,3,4),(0.,0.125,0.1875,0.21875,0.25,0.28125,0.3125,0.375,0.5,0.625,
0.633652818087256,0.75,0.8125,0.84375,0.875,0.90625,0.9375,0.99999982127163),
 .UNSPECIFIED.);
#489=B_SPLINE_CURVE_WITH_KNOTS('',3,(#28850,#28851,#28852,#28853,#28854,
#28855,#28856,#28857,#28858,#28859,#28860,#28861,#28862,#28863,#28864,#28865,
#28866,#28867,#28868),.UNSPECIFIED.,.F.,.F.,(4,1,1,1,1,1,1,1,1,1,1,1,1,
1,1,1,4),(2.60020861133173E-7,0.0625,0.09375,0.125,0.15625,0.1875,0.25,
0.375,0.5,0.625,0.6875,0.71875,0.75,0.78125,0.8125,0.875,0.999999902697824),
 .UNSPECIFIED.);
#490=B_SPLINE_CURVE_WITH_KNOTS('',3,(#28870,#28871,#28872,#28873,#28874,
#28875,#28876,#28877,#28878),.UNSPECIFIED.,.F.,.F.,(4,1,1,1,1,1,4),(0.,
0.125,0.1875,0.21875,0.25,0.28125,0.298021461655708),.UNSPECIFIED.);
#491=B_SPLINE_CURVE_WITH_KNOTS('',1,(#28880,#28881),.UNSPECIFIED.,.F.,.F.,
(2,2),(-0.214862684454297,-0.201578551331348),.UNSPECIFIED.);
#492=B_SPLINE_CURVE_WITH_KNOTS('',3,(#28883,#28884,#28885,#28886,#28887,
#28888,#28889,#28890,#28891,#28892,#28893,#28894,#28895,#28896,#28897,#28898,
#28899,#28900,#28901),.UNSPECIFIED.,.F.,.F.,(4,3,3,3,3,3,4),(0.0574863041974119,
0.125,0.1875,0.21875,0.25,0.28125,0.293194800091934),.UNSPECIFIED.);
#493=B_SPLINE_CURVE_WITH_KNOTS('',3,(#28903,#28904,#28905,#28906),
 .UNSPECIFIED.,.F.,.F.,(4,4),(6.86640626528075E-6,0.0574863041974119),
 .UNSPECIFIED.);
#494=B_SPLINE_CURVE_WITH_KNOTS('',3,(#28908,#28909,#28910,#28911,#28912,
#28913,#28914,#28915,#28916,#28917,#28918,#28919,#28920,#28921,#28922,#28923,
#28924,#28925,#28926,#28927,#28928,#28929,#28930,#28931,#28932,#28933,#28934,
#28935,#28936,#28937,#28938,#28939,#28940,#28941,#28942,#28943,#28944,#28945,
#28946,#28947,#28948,#28949,#28950,#28951,#28952,#28953,#28954,#28955,#28956,
#28957,#28958,#28959),.UNSPECIFIED.,.F.,.F.,(4,3,3,3,3,3,3,3,3,3,3,3,3,
3,3,3,3,4),(0.,0.125,0.1875,0.21875,0.25,0.28125,0.3125,0.375,0.5,0.625,
0.66804399378711,0.75,0.8125,0.84375,0.875,0.90625,0.9375,0.999999677104164),
 .UNSPECIFIED.);
#495=B_SPLINE_CURVE_WITH_KNOTS('',3,(#28961,#28962,#28963,#28964,#28965,
#28966,#28967,#28968,#28969),.UNSPECIFIED.,.F.,.F.,(4,1,1,1,1,1,4),(0.,
0.125,0.1875,0.25,0.3125,0.375,0.499188038144574),.UNSPECIFIED.);
#496=B_SPLINE_CURVE_WITH_KNOTS('',3,(#28971,#28972,#28973,#28974,#28975,
#28976,#28977,#28978,#28979),.UNSPECIFIED.,.F.,.F.,(4,1,1,1,1,1,4),(0.499188038144574,
0.5,0.625,0.75,0.875,0.9375,0.998196008235996),.UNSPECIFIED.);
#497=B_SPLINE_CURVE_WITH_KNOTS('',3,(#28981,#28982,#28983,#28984,#28985,
#28986,#28987,#28988,#28989,#28990,#28991,#28992,#28993,#28994,#28995,#28996,
#28997,#28998,#28999,#29000,#29001,#29002,#29003,#29004,#29005,#29006,#29007,
#29008,#29009,#29010,#29011,#29012,#29013,#29014,#29015,#29016,#29017,#29018,
#29019,#29020,#29021,#29022,#29023,#29024,#29025,#29026,#29027,#29028,#29029),
 .UNSPECIFIED.,.F.,.F.,(4,3,3,3,3,3,3,3,3,3,3,3,3,3,3,3,4),(0.,0.125,0.1875,
0.21875,0.25,0.28125,0.3125,0.375,0.4375,0.5,0.5625,0.625,0.6875,0.75,0.809462341510482,
0.875,1.),.UNSPECIFIED.);
#498=B_SPLINE_CURVE_WITH_KNOTS('',3,(#29031,#29032,#29033,#29034,#29035,
#29036,#29037,#29038,#29039,#29040,#29041,#29042,#29043,#29044,#29045,#29046,
#29047,#29048,#29049,#29050,#29051,#29052),.UNSPECIFIED.,.F.,.F.,(4,3,3,
3,3,3,3,4),(0.626108993264048,0.6875,0.71875,0.75,0.78125,0.8125,0.875,
0.999993195039302),.UNSPECIFIED.);
#499=B_SPLINE_CURVE_WITH_KNOTS('',1,(#29054,#29055),.UNSPECIFIED.,.F.,.F.,
(2,2),(-0.181505671215862,-0.1040158100396),.UNSPECIFIED.);
#500=B_SPLINE_CURVE_WITH_KNOTS('',3,(#29057,#29058,#29059,#29060),
 .UNSPECIFIED.,.F.,.F.,(4,4),(0.915239918615735,1.),.UNSPECIFIED.);
#501=B_SPLINE_CURVE_WITH_KNOTS('',3,(#29062,#29063,#29064,#29065),
 .UNSPECIFIED.,.F.,.F.,(4,4),(0.75,1.),.UNSPECIFIED.);
#502=B_SPLINE_CURVE_WITH_KNOTS('',3,(#29067,#29068,#29069,#29070,#29071,
#29072,#29073,#29074,#29075,#29076,#29077,#29078,#29079),.UNSPECIFIED.,
 .F.,.F.,(4,3,3,3,4),(6.7281280280231E-5,0.25,0.375,0.5,0.75),
 .UNSPECIFIED.);
#503=B_SPLINE_CURVE_WITH_KNOTS('',3,(#29081,#29082,#29083,#29084),
 .UNSPECIFIED.,.F.,.F.,(4,4),(0.380644930253737,0.999995028027359),
 .UNSPECIFIED.);
#504=B_SPLINE_CURVE_WITH_KNOTS('',3,(#29086,#29087,#29088,#29089),
 .UNSPECIFIED.,.F.,.F.,(4,4),(0.,0.380644930253737),.UNSPECIFIED.);
#505=B_SPLINE_CURVE_WITH_KNOTS('',3,(#29091,#29092,#29093,#29094,#29095,
#29096,#29097,#29098,#29099,#29100,#29101,#29102,#29103,#29104,#29105,#29106,
#29107),.UNSPECIFIED.,.F.,.F.,(4,1,1,1,1,1,1,1,1,1,1,1,1,1,4),(0.,0.125,
0.1875,0.25,0.3125,0.375,0.4375,0.5,0.625,0.6875,0.75,0.8125,0.875,0.9375,
0.999999571178552),.UNSPECIFIED.);
#506=B_SPLINE_CURVE_WITH_KNOTS('',3,(#29109,#29110,#29111,#29112),
 .UNSPECIFIED.,.F.,.F.,(4,4),(0.,1.),.UNSPECIFIED.);
#507=B_SPLINE_CURVE_WITH_KNOTS('',3,(#29113,#29114,#29115,#29116,#29117,
#29118,#29119,#29120,#29121,#29122,#29123,#29124,#29125,#29126,#29127,#29128),
 .UNSPECIFIED.,.F.,.F.,(4,3,3,3,3,4),(0.,0.0575860235571798,0.125,0.25,
0.3125,0.364118167489102),.UNSPECIFIED.);
#508=B_SPLINE_CURVE_WITH_KNOTS('',3,(#29271,#29272,#29273,#29274),
 .UNSPECIFIED.,.F.,.F.,(4,4),(-0.801761649289337,-0.764530975504951),
 .UNSPECIFIED.);
#509=B_SPLINE_CURVE_WITH_KNOTS('',3,(#29276,#29277,#29278,#29279,#29280,
#29281,#29282,#29283,#29284,#29285,#29286,#29287,#29288,#29289,#29290,#29291,
#29292,#29293,#29294,#29295,#29296,#29297,#29298,#29299,#29300,#29301,#29302,
#29303,#29304,#29305,#29306,#29307,#29308,#29309,#29310,#29311,#29312,#29313,
#29314,#29315,#29316,#29317,#29318,#29319,#29320,#29321,#29322,#29323,#29324,
#29325,#29326,#29327,#29328,#29329,#29330),.UNSPECIFIED.,.F.,.F.,(4,3,3,
3,3,3,3,3,3,3,3,3,3,3,3,3,3,3,4),(3.7275728618467E-8,0.00213268712132415,
0.00241015582328363,0.00361523373492544,0.00482031164656725,0.00602538955820906,
0.00666926365661724,0.00723046746985087,0.00843554538149267,0.00883404960601883,
0.00964062329313448,0.0108457012047763,0.0115672277245366,0.0120507791164181,
0.0143099259775042,0.0144609349397017,0.0155427936599299,0.0156660128513435,
0.0167172049195214),.UNSPECIFIED.);
#510=B_SPLINE_CURVE_WITH_KNOTS('',3,(#29332,#29333,#29334,#29335,#29336,
#29337,#29338,#29339,#29340,#29341,#29342,#29343,#29344,#29345,#29346,#29347,
#29348,#29349),.UNSPECIFIED.,.F.,.F.,(4,2,2,2,2,2,2,2,4),(0.,0.125,0.25,
0.375,0.5,0.625,0.75,0.875,1.),.UNSPECIFIED.);
#511=B_SPLINE_CURVE_WITH_KNOTS('',3,(#29351,#29352,#29353,#29354,#29355,
#29356,#29357,#29358,#29359,#29360,#29361,#29362,#29363,#29364,#29365,#29366,
#29367,#29368,#29369,#29370,#29371,#29372,#29373,#29374,#29375,#29376,#29377,
#29378,#29379,#29380,#29381,#29382,#29383,#29384,#29385,#29386,#29387,#29388,
#29389,#29390,#29391,#29392,#29393,#29394,#29395,#29396,#29397,#29398,#29399,
#29400,#29401,#29402,#29403,#29404,#29405,#29406,#29407,#29408,#29409,#29410,
#29411,#29412,#29413,#29414,#29415,#29416,#29417,#29418,#29419,#29420),
 .UNSPECIFIED.,.F.,.F.,(4,3,3,3,3,3,3,3,3,3,3,3,3,3,3,3,3,3,3,3,3,3,3,4),
(1.08058869667645E-7,0.000426646628827551,0.00122648046975059,0.00145211381056247,
0.0024529609387835,0.00255429073838069,0.00367944140781642,0.00374167552846414,
0.00490592187684933,0.0050104433434355,0.00735888281491516,0.0079238714718458,
0.00858536328394808,0.00981184375298099,0.010715819001823,0.0110383242220139,
0.0122648046910468,0.0128618444900144,0.0134912851600797,0.0147177656291127,
0.0159442460981456,0.0171707265671785,0.0174912668652558,0.0196236713267414),
 .UNSPECIFIED.);
#512=B_SPLINE_CURVE_WITH_KNOTS('',3,(#29422,#29423,#29424,#29425,#29426,
#29427,#29428,#29429,#29430,#29431,#29432,#29433,#29434,#29435,#29436,#29437,
#29438,#29439,#29440,#29441,#29442,#29443,#29444,#29445,#29446,#29447,#29448,
#29449,#29450,#29451,#29452,#29453,#29454,#29455,#29456,#29457,#29458,#29459,
#29460,#29461),.UNSPECIFIED.,.F.,.F.,(4,3,3,3,3,3,3,3,3,3,3,3,3,4),(0.0138309084487971,
0.0141209324226746,0.0144279092144626,0.0147348860062506,0.0147783505908347,
0.0153488395898266,0.0158093047775086,0.0158956420001989,0.0159765831464712,
0.0160205263564273,0.0171907003405545,0.0172599467341181,0.0178046539241305,
0.019646491834798),.UNSPECIFIED.);
#513=B_SPLINE_CURVE_WITH_KNOTS('',3,(#29463,#29464,#29465,#29466),
 .UNSPECIFIED.,.F.,.F.,(4,4),(-0.900360708476172,-0.86499516359624),
 .UNSPECIFIED.);
#514=B_SPLINE_CURVE_WITH_KNOTS('',3,(#29468,#29469,#29470,#29471,#29472,
#29473,#29474),.UNSPECIFIED.,.F.,.F.,(4,1,1,1,4),(3.72393009463586E-10,
0.00112032596633615,0.00224065181164156,0.00336097765694698,0.00404745390640756),
 .UNSPECIFIED.);
#515=B_SPLINE_CURVE_WITH_KNOTS('',3,(#29476,#29477,#29478,#29479,#29480,
#29481,#29482,#29483,#29484,#29485,#29486,#29487,#29488,#29489,#29490,#29491,
#29492,#29493,#29494,#29495,#29496,#29497,#29498,#29499,#29500,#29501,#29502,
#29503,#29504,#29505,#29506,#29507,#29508,#29509),.UNSPECIFIED.,.F.,.F.,
(4,3,3,3,3,3,3,3,3,3,3,4),(1.56135529065312E-9,0.000149014693064497,0.000707813936974023,
0.00112691336990617,0.00118870219951449,0.00128407565725572,0.0023842116687026,
0.00241586779852081,0.00298026419553942,0.00357631672237625,0.00364795327462914,
0.00380005432105398),.UNSPECIFIED.);
#516=B_SPLINE_CURVE_WITH_KNOTS('',3,(#29511,#29512,#29513,#29514),
 .UNSPECIFIED.,.F.,.F.,(4,4),(-0.788485824448602,-0.75173722881735),
 .UNSPECIFIED.);
#517=B_SPLINE_CURVE_WITH_KNOTS('',3,(#29516,#29517,#29518,#29519,#29520,
#29521,#29522,#29523,#29524,#29525),.UNSPECIFIED.,.F.,.F.,(4,3,3,4),(3.52393154467455E-8,
0.00220719129062706,0.00226386756700581,0.00462327622956672),
 .UNSPECIFIED.);
#518=B_SPLINE_CURVE_WITH_KNOTS('',3,(#29527,#29528,#29529,#29530,#29531,
#29532,#29533,#29534,#29535,#29536),.UNSPECIFIED.,.F.,.F.,(4,3,3,4),(7.932060984575E-15,
0.00157881831260296,0.00235387237808879,0.00470771557316006),
 .UNSPECIFIED.);
#519=B_SPLINE_CURVE_WITH_KNOTS('',3,(#29538,#29539,#29540,#29541,#29542,
#29543,#29544,#29545),.UNSPECIFIED.,.F.,.F.,(4,2,2,4),(7.02291898378891E-6,
0.0451293601147105,0.0692682469770136,0.0896084138988641),.UNSPECIFIED.);
#520=B_SPLINE_CURVE_WITH_KNOTS('',3,(#29547,#29548,#29549,#29550,#29551,
#29552),.UNSPECIFIED.,.F.,.F.,(4,2,4),(0.00040201242378087,0.0139583175638981,
0.0275208583776574),.UNSPECIFIED.);
#521=B_SPLINE_CURVE_WITH_KNOTS('',3,(#29554,#29555,#29556,#29557,#29558,
#29559),.UNSPECIFIED.,.F.,.F.,(4,2,4),(6.53624102621552E-6,0.0289149570250049,
0.0574752936489782),.UNSPECIFIED.);
#522=B_SPLINE_CURVE_WITH_KNOTS('',3,(#29561,#29562,#29563,#29564,#29565,
#29566),.UNSPECIFIED.,.F.,.F.,(4,2,4),(-0.100164676307967,-0.0501603860011391,
-0.000310269947608522),.UNSPECIFIED.);
#523=B_SPLINE_CURVE_WITH_KNOTS('',3,(#29568,#29569,#29570,#29571,#29572,
#29573),.UNSPECIFIED.,.F.,.F.,(4,2,4),(0.000156968191344601,0.0294034008226515,
0.0586209359117642),.UNSPECIFIED.);
#524=B_SPLINE_CURVE_WITH_KNOTS('',3,(#29575,#29576,#29577,#29578,#29579,
#29580),.UNSPECIFIED.,.F.,.F.,(4,2,4),(5.32014841871761E-5,0.0390048636397492,
0.0777949467112503),.UNSPECIFIED.);
#525=B_SPLINE_CURVE_WITH_KNOTS('',3,(#29582,#29583,#29584,#29585,#29586,
#29587,#29588,#29589,#29590,#29591,#29592,#29593,#29594),.UNSPECIFIED.,
 .F.,.F.,(4,3,3,3,4),(8.67361737988404E-19,7.42016414987991E-5,0.00236271426147704,
0.00354407139221556,0.00472542852295408),.UNSPECIFIED.);
#526=B_SPLINE_CURVE_WITH_KNOTS('',3,(#29596,#29597,#29598,#29599,#29600,
#29601,#29602,#29603,#29604,#29605,#29606,#29607,#29608,#29609,#29610,#29611,
#29612,#29613,#29614,#29615,#29616,#29617,#29618,#29619,#29620,#29621,#29622,
#29623,#29624,#29625,#29626,#29627,#29628,#29629,#29630,#29631,#29632,#29633,
#29634,#29635,#29636,#29637,#29638,#29639,#29640,#29641,#29642,#29643,#29644,
#29645,#29646,#29647,#29648,#29649,#29650,#29651,#29652,#29653,#29654,#29655,
#29656,#29657,#29658,#29659,#29660,#29661,#29662,#29663,#29664,#29665,#29666,
#29667,#29668),.UNSPECIFIED.,.F.,.F.,(4,3,3,3,3,3,3,3,3,3,3,3,3,3,3,3,3,
3,3,3,3,3,3,3,4),(0.,7.75161947677991E-5,0.00111757680617575,0.00223515361235151,
0.00335273041852726,0.00391151882161514,0.00447030722470301,0.00499947827886225,
0.00502909562779089,0.00558788403087876,0.00670546083705452,0.00745503820642138,
0.00782303764323027,0.00894061444940602,0.0104502859150961,0.0111757680617575,
0.0130679753464858,0.013410921674109,0.0142514928999412,0.0145284984802848,
0.0153723205684816,0.0156460752864605,0.0164339145851788,0.0174532669379536,
0.017881228898812),.UNSPECIFIED.);
#527=B_SPLINE_CURVE_WITH_KNOTS('',3,(#29670,#29671,#29672,#29673,#29674,
#29675,#29676,#29677,#29678,#29679,#29680,#29681,#29682,#29683,#29684,#29685,
#29686,#29687,#29688,#29689,#29690,#29691,#29692,#29693,#29694,#29695,#29696,
#29697,#29698,#29699,#29700,#29701,#29702,#29703,#29704,#29705,#29706,#29707,
#29708,#29709,#29710,#29711,#29712,#29713,#29714,#29715,#29716,#29717,#29718,
#29719,#29720,#29721,#29722,#29723,#29724,#29725,#29726,#29727,#29728,#29729,
#29730,#29731,#29732,#29733),.UNSPECIFIED.,.F.,.F.,(4,3,3,3,3,3,3,3,3,3,
3,3,3,3,3,3,3,3,3,3,3,4),(0.,0.00158828845524716,0.0021893200599713,0.00264594734442174,
0.00328398008995695,0.00375597387774578,0.0043786401199426,0.00615520482571866,
0.0065679601799139,0.0087572802398852,0.0088668805883462,0.00985194026987085,
0.0109466002998565,0.011634371002562,0.0120412603298422,0.012588590344835,
0.0131359203598278,0.0142305803898135,0.0153252404197991,0.016220768789973,
0.0164199004497848,0.0175145604797704),.UNSPECIFIED.);
#528=B_SPLINE_CURVE_WITH_KNOTS('',3,(#29735,#29736,#29737,#29738,#29739,
#29740,#29741,#29742,#29743,#29744,#29745,#29746,#29747,#29748,#29749,#29750,
#29751,#29752,#29753,#29754,#29755,#29756,#29757,#29758,#29759,#29760,#29761,
#29762,#29763,#29764,#29765,#29766,#29767,#29768,#29769,#29770,#29771),
 .UNSPECIFIED.,.F.,.F.,(4,3,3,3,3,3,3,3,3,3,3,3,4),(0.,0.000297867429863575,
0.000744668574658938,0.000968069147056619,0.00110064938673372,0.0011914697194543,
0.00178720457918146,0.00193613829411324,0.00234224251489775,0.00238293943890861,
0.00297867429863576,0.00359302587272938,0.00476587887781721),
 .UNSPECIFIED.);
#529=B_SPLINE_CURVE_WITH_KNOTS('',3,(#29773,#29774,#29775,#29776,#29777,
#29778),.UNSPECIFIED.,.F.,.F.,(4,2,4),(0.000112668959181985,0.0394878781786619,
0.0787740170229608),.UNSPECIFIED.);
#530=B_SPLINE_CURVE_WITH_KNOTS('',3,(#29782,#29783,#29784,#29785,#29786,
#29787),.UNSPECIFIED.,.F.,.F.,(4,2,4),(4.69002654761246E-6,0.050001342311006,
0.0999913387878795),.UNSPECIFIED.);
#531=B_SPLINE_CURVE_WITH_KNOTS('',3,(#29791,#29792,#29793,#29794,#29795,
#29796),.UNSPECIFIED.,.F.,.F.,(4,2,4),(0.000695999025172847,0.013935683082129,
0.0269158957041709),.UNSPECIFIED.);
#532=B_SPLINE_CURVE_WITH_KNOTS('',3,(#29798,#29799,#29800,#29801,#29802,
#29803,#29804,#29805),.UNSPECIFIED.,.F.,.F.,(4,2,2,4),(4.60554727665049E-5,
0.0201218316749581,0.0440109401186668,0.0887346835144923),.UNSPECIFIED.);
#533=B_SPLINE_CURVE_WITH_KNOTS('',3,(#29807,#29808,#29809,#29810,#29811,
#29812,#29813),.UNSPECIFIED.,.F.,.F.,(4,3,4),(3.18003771205116E-15,0.0023582377455569,
0.00470691707255086),.UNSPECIFIED.);
#534=B_SPLINE_CURVE_WITH_KNOTS('',3,(#29815,#29816,#29817,#29818,#29819,
#29820,#29821,#29822,#29823,#29824),.UNSPECIFIED.,.F.,.F.,(4,3,3,4),(3.44289573972157E-8,
0.00232495486867497,0.00307076742172914,0.00464990715460391),
 .UNSPECIFIED.);
#535=B_SPLINE_CURVE_WITH_KNOTS('',3,(#29826,#29827,#29828,#29829,#29830,
#29831,#29832,#29833),.UNSPECIFIED.,.F.,.F.,(4,2,2,4),(6.42183317534942E-6,
0.04781967269061,0.0732367945616579,0.0950553531959799),.UNSPECIFIED.);
#536=B_SPLINE_CURVE_WITH_KNOTS('',3,(#29835,#29836,#29837,#29838,#29839,
#29840),.UNSPECIFIED.,.F.,.F.,(4,2,4),(0.000374884371361637,0.0150232472508783,
0.0297168549388432),.UNSPECIFIED.);
#537=B_SPLINE_CURVE_WITH_KNOTS('',3,(#29842,#29843,#29844,#29845,#29846,
#29847),.UNSPECIFIED.,.F.,.F.,(4,2,4),(6.13317120454564E-6,0.0290789797557169,
0.0578659870050568),.UNSPECIFIED.);
#538=B_SPLINE_CURVE_WITH_KNOTS('',3,(#29849,#29850,#29851,#29852,#29853,
#29854),.UNSPECIFIED.,.F.,.F.,(4,2,4),(1.00018224971625E-5,0.0500087821938493,
0.10001293618161),.UNSPECIFIED.);
#539=B_SPLINE_CURVE_WITH_KNOTS('',3,(#29856,#29857,#29858,#29859,#29860,
#29861),.UNSPECIFIED.,.F.,.F.,(4,2,4),(7.53330920655929E-6,0.0293896381172448,
0.0587097736963051),.UNSPECIFIED.);
#540=B_SPLINE_CURVE_WITH_KNOTS('',3,(#29863,#29864,#29865,#29866,#29867,
#29868),.UNSPECIFIED.,.F.,.F.,(4,2,4),(8.20230271009787E-5,0.0377809065926269,
0.0755399468969054),.UNSPECIFIED.);
#541=B_SPLINE_CURVE_WITH_KNOTS('',3,(#29870,#29871,#29872,#29873,#29874,
#29875),.UNSPECIFIED.,.F.,.F.,(4,1,1,4),(0.,0.00119697920627212,0.00239395841254424,
0.00478791682508848),.UNSPECIFIED.);
#542=B_SPLINE_CURVE_WITH_KNOTS('',3,(#29876,#29877,#29878,#29879,#29880,
#29881,#29882,#29883,#29884,#29885,#29886,#29887,#29888,#29889,#29890,#29891),
 .UNSPECIFIED.,.F.,.F.,(4,1,1,1,1,1,1,1,1,1,1,1,1,4),(0.00248265578786311,
0.00329931417081839,0.00439908556096978,0.00659862834127257,0.00879817112157535,
0.00989794251172675,0.0109977139018781,0.0120974852920295,0.0126473709871052,
0.0131972566821809,0.0142970280723323,0.0153967994624837,0.0164965708526351,
0.0175963422427865),.UNSPECIFIED.);
#543=B_SPLINE_CURVE_WITH_KNOTS('',3,(#29894,#29895,#29896,#29897,#29898,
#29899),.UNSPECIFIED.,.F.,.F.,(4,2,4),(-0.351103621180421,-0.184658836618039,
-0.000144336259837594),.UNSPECIFIED.);
#544=B_SPLINE_CURVE_WITH_KNOTS('',3,(#29901,#29902,#29903,#29904,#29905,
#29906,#29907,#29908),.UNSPECIFIED.,.F.,.F.,(4,2,2,4),(0.00013573500535706,
0.152913187988002,0.221936523531357,0.281794792544631),.UNSPECIFIED.);
#545=B_SPLINE_CURVE_WITH_KNOTS('',3,(#29910,#29911,#29912,#29913,#29914,
#29915,#29916,#29917),.UNSPECIFIED.,.F.,.F.,(4,2,2,4),(8.16139213976878E-5,
0.0601010912620195,0.129621118816494,0.284198839020368),.UNSPECIFIED.);
#546=B_SPLINE_CURVE_WITH_KNOTS('',3,(#29918,#29919,#29920,#29921,#29922,
#29923,#29924,#29925,#29926,#29927,#29928,#29929,#29930,#29931,#29932,#29933,
#29934,#29935,#29936,#29937,#29938,#29939,#29940,#29941,#29942,#29943,#29944,
#29945,#29946,#29947,#29948,#29949,#29950,#29951,#29952,#29953,#29954,#29955,
#29956,#29957,#29958,#29959,#29960,#29961,#29962,#29963,#29964,#29965,#29966,
#29967,#29968,#29969,#29970,#29971,#29972,#29973,#29974,#29975,#29976,#29977,
#29978,#29979,#29980,#29981,#29982,#29983,#29984),.UNSPECIFIED.,.F.,.F.,
(4,3,3,3,3,3,3,3,3,3,3,3,3,3,3,3,3,3,3,3,3,3,4),(0.,0.000109920237579343,
0.00061591770973852,0.000934322019424417,0.000985847130789734,0.00103415192269472,
0.00119683823187687,0.00172622571154797,0.00175872380126949,0.0019699967952482,
0.00219840475158686,0.00236328510795588,0.00243542026386732,0.0025030469725343,
0.00272120378944146,0.00286687736586743,0.00301024728753664,0.00304119051135285,
0.00326384744503781,0.00339064752378839,0.00345404756316369,0.00348574758285133,
0.00351744760253898),.UNSPECIFIED.);
#547=B_SPLINE_CURVE_WITH_KNOTS('',3,(#29987,#29988,#29989,#29990,#29991,
#29992,#29993,#29994),.UNSPECIFIED.,.F.,.F.,(4,2,2,4),(0.,0.0594485370103995,
0.128200922849087,0.28027816230381),.UNSPECIFIED.);
#548=B_SPLINE_CURVE_WITH_KNOTS('',3,(#29996,#29997,#29998,#29999,#30000,
#30001),.UNSPECIFIED.,.F.,.F.,(4,2,4),(-0.353460855213146,-0.168401493160792,
0.),.UNSPECIFIED.);
#549=B_SPLINE_CURVE_WITH_KNOTS('',3,(#30003,#30004,#30005,#30006,#30007,
#30008),.UNSPECIFIED.,.F.,.F.,(4,2,4),(-0.35246001194512,-0.169875343850794,
-8.95159592229078E-7),.UNSPECIFIED.);
#550=B_SPLINE_CURVE_WITH_KNOTS('',3,(#30009,#30010,#30011,#30012,#30013,
#30014,#30015,#30016),.UNSPECIFIED.,.F.,.F.,(4,2,2,4),(0.000136900112796742,
0.156887006623476,0.227547774409115,0.288714197538024),.UNSPECIFIED.);
#551=B_SPLINE_CURVE_WITH_KNOTS('',3,(#30158,#30159,#30160,#30161,#30162),
 .UNSPECIFIED.,.F.,.F.,(4,1,4),(3.64204572566108E-13,0.00219954278066699,
0.00248265578786311),.UNSPECIFIED.);
#552=B_SPLINE_CURVE_WITH_KNOTS('',3,(#30163,#30164,#30165,#30166,#30167,
#30168,#30169,#30170,#30171,#30172,#30173,#30174,#30175,#30176),
 .UNSPECIFIED.,.F.,.F.,(4,1,1,1,1,1,1,1,1,1,1,4),(0.00404745390640756,0.00448130350225239,
0.0050414664249051,0.00560162934755781,0.00672195519286322,0.00784228103816864,
0.00896260688347405,0.0112032585740849,0.0134439102646957,0.0145642361100011,
0.0156845619553065,0.0179252136459174),.UNSPECIFIED.);
#553=B_SPLINE_CURVE_WITH_KNOTS('',3,(#30178,#30179,#30180,#30181,#30182,
#30183,#30184,#30185,#30186,#30187,#30188,#30189,#30190,#30191,#30192,#30193,
#30194,#30195,#30196,#30197,#30198,#30199,#30200,#30201,#30202,#30203,#30204,
#30205,#30206,#30207,#30208,#30209,#30210,#30211,#30212,#30213,#30214,#30215,
#30216,#30217,#30218,#30219,#30220,#30221,#30222,#30223,#30224,#30225,#30226,
#30227,#30228,#30229,#30230,#30231,#30232,#30233,#30234,#30235,#30236,#30237,
#30238,#30239,#30240,#30241,#30242,#30243,#30244,#30245,#30246,#30247,#30248,
#30249,#30250,#30251,#30252,#30253,#30254,#30255,#30256,#30257,#30258,#30259,
#30260,#30261,#30262,#30263,#30264,#30265,#30266,#30267,#30268,#30269,#30270,
#30271,#30272,#30273,#30274,#30275,#30276,#30277,#30278,#30279,#30280,#30281,
#30282,#30283,#30284,#30285,#30286),.UNSPECIFIED.,.F.,.F.,(4,3,3,3,3,3,
3,3,3,3,3,3,3,3,3,3,3,3,3,3,3,3,3,3,3,3,3,3,3,3,3,3,3,3,3,3,4),(4.26881478763691E-13,
0.000306976792214876,0.00112686428044965,0.00122790716757886,0.00138139556347286,
0.00191860494910184,0.00218720964191634,0.00238136727005047,0.00245581433473083,
0.0036439705098947,0.0036837215018828,0.00429767508545879,0.00489317856768551,
0.00491162866903478,0.00613953583618676,0.00675348941976274,0.00736744300333873,
0.00739256586998839,0.00798139658691471,0.0085953501704907,0.00863787380293649,
0.00920930375406668,0.00982325733764267,0.00986608700714022,0.0104372109212186,
0.0110511645047946,0.0110965072788747,0.0113581412965826,0.0118186064842646,
0.0122790716719466,0.0123256390264983,0.0128930252555226,0.0132000020473106,
0.0133534904432046,0.0135069788390986,0.0135490258016012,0.0138309084487971),
 .UNSPECIFIED.);
#554=B_SPLINE_CURVE_WITH_KNOTS('',3,(#30287,#30288,#30289,#30290,#30291,
#30292,#30293,#30294,#30295,#30296,#30297,#30298,#30299,#30300,#30301,#30302),
 .UNSPECIFIED.,.F.,.F.,(4,3,3,3,3,4),(0.0167172049195214,0.0168710907629853,
0.0178203760382903,0.0180761686746271,0.0188523687683586,0.019281246586269),
 .UNSPECIFIED.);
#555=B_SPLINE_CURVE_WITH_KNOTS('',3,(#30306,#30307,#30308,#30309,#30310,
#30311),.UNSPECIFIED.,.F.,.F.,(4,2,4),(-1.66978451121418,-1.49281136073648,
-1.33992830231631),.UNSPECIFIED.);
#556=B_SPLINE_CURVE_WITH_KNOTS('',3,(#30313,#30314,#30315,#30316,#30317,
#30318,#30319,#30320,#30321,#30322,#30323,#30324),.UNSPECIFIED.,.F.,.F.,
(4,1,1,1,1,1,1,1,1,4),(0.,0.25,0.375,0.5,0.625,0.6875,0.75,0.8125,0.875,
1.),.UNSPECIFIED.);
#557=B_SPLINE_CURVE_WITH_KNOTS('',3,(#30326,#30327,#30328,#30329),
 .UNSPECIFIED.,.F.,.F.,(4,4),(2.50930273678697,2.78682786773594),
 .UNSPECIFIED.);
#558=B_SPLINE_CURVE_WITH_KNOTS('',3,(#30330,#30331,#30332,#30333,#30334,
#30335),.UNSPECIFIED.,.F.,.F.,(4,2,4),(2.77504169139609,2.7756154298488,
3.04976295261124),.UNSPECIFIED.);
#559=B_SPLINE_CURVE_WITH_KNOTS('',3,(#30397,#30398,#30399,#30400,#30401,
#30402,#30403,#30404,#30405,#30406,#30407,#30408,#30409,#30410,#30411,#30412,
#30413,#30414,#30415,#30416,#30417,#30418,#30419,#30420,#30421,#30422,#30423,
#30424,#30425,#30426,#30427,#30428,#30429,#30430),.UNSPECIFIED.,.F.,.F.,
(4,3,3,3,3,3,3,3,3,3,3,4),(0.364118167489102,0.375,0.434093352847254,0.5,
0.56610957647016,0.625,0.635973158026349,0.6875,0.75,0.875,0.942536907276119,
1.),.UNSPECIFIED.);
#560=B_SPLINE_CURVE_WITH_KNOTS('',3,(#30432,#30433,#30434,#30435),
 .UNSPECIFIED.,.F.,.F.,(4,4),(0.,1.),.UNSPECIFIED.);
#561=B_SPLINE_CURVE_WITH_KNOTS('',3,(#30437,#30438,#30439,#30440,#30441,
#30442,#30443,#30444,#30445,#30446,#30447,#30448,#30449,#30450,#30451,#30452,
#30453),.UNSPECIFIED.,.F.,.F.,(4,1,1,1,1,1,1,1,1,1,1,1,1,1,4),(3.19570811666715E-7,
0.0625,0.125,0.1875,0.25,0.3125,0.375,0.5,0.5625,0.625,0.6875,0.75,0.8125,
0.875,1.),.UNSPECIFIED.);
#562=B_SPLINE_CURVE_WITH_KNOTS('',3,(#30455,#30456,#30457,#30458),
 .UNSPECIFIED.,.F.,.F.,(4,4),(0.75,1.),.UNSPECIFIED.);
#563=B_SPLINE_CURVE_WITH_KNOTS('',3,(#30460,#30461,#30462,#30463,#30464,
#30465,#30466,#30467,#30468,#30469,#30470,#30471,#30472),.UNSPECIFIED.,
 .F.,.F.,(4,3,3,3,4),(6.9291577602274E-5,0.25,0.375,0.5,0.75),
 .UNSPECIFIED.);
#564=B_SPLINE_CURVE_WITH_KNOTS('',3,(#30474,#30475,#30476,#30477),
 .UNSPECIFIED.,.F.,.F.,(4,4),(0.380639039903466,0.999995038571591),
 .UNSPECIFIED.);
#565=B_SPLINE_CURVE_WITH_KNOTS('',3,(#30479,#30480,#30481,#30482),
 .UNSPECIFIED.,.F.,.F.,(4,4),(0.,0.380639039903466),.UNSPECIFIED.);
#566=B_SPLINE_CURVE_WITH_KNOTS('',3,(#30484,#30485,#30486,#30487,#30488,
#30489,#30490,#30491,#30492,#30493,#30494,#30495,#30496,#30497,#30498,#30499,
#30500),.UNSPECIFIED.,.F.,.F.,(4,1,1,1,1,1,1,1,1,1,1,1,1,1,4),(0.,0.125,
0.1875,0.25,0.3125,0.375,0.4375,0.5,0.625,0.6875,0.75,0.8125,0.875,0.9375,
0.999999754494977),.UNSPECIFIED.);
#567=B_SPLINE_CURVE_WITH_KNOTS('',3,(#30502,#30503,#30504,#30505),
 .UNSPECIFIED.,.F.,.F.,(4,4),(0.,1.),.UNSPECIFIED.);
#568=B_SPLINE_CURVE_WITH_KNOTS('',3,(#30507,#30508,#30509,#30510,#30511,
#30512,#30513,#30514,#30515,#30516,#30517,#30518,#30519),.UNSPECIFIED.,
 .F.,.F.,(4,1,1,1,1,1,1,1,1,1,4),(0.,0.125,0.25,0.3125,0.375,0.5,0.625,
0.6875,0.75,0.875,1.),.UNSPECIFIED.);
#569=B_SPLINE_CURVE_WITH_KNOTS('',3,(#30521,#30522,#30523,#30524),
 .UNSPECIFIED.,.F.,.F.,(4,4),(0.,1.),.UNSPECIFIED.);
#570=B_SPLINE_CURVE_WITH_KNOTS('',3,(#30525,#30526,#30527,#30528,#30529,
#30530,#30531,#30532,#30533,#30534,#30535,#30536,#30537,#30538,#30539,#30540,
#30541),.UNSPECIFIED.,.F.,.F.,(4,1,1,1,1,1,1,1,1,1,1,1,1,1,4),(4.29717416154947E-7,
0.0625,0.125,0.1875,0.25,0.3125,0.375,0.5,0.5625,0.625,0.6875,0.75,0.8125,
0.875,0.915239918615735),.UNSPECIFIED.);
#571=B_SPLINE_CURVE_WITH_KNOTS('',3,(#30543,#30544,#30545,#30546,#30547,
#30548,#30549,#30550,#30551,#30552,#30553,#30554,#30555,#30556,#30557,#30558,
#30559,#30560,#30561,#30562,#30563,#30564,#30565,#30566,#30567,#30568,#30569,
#30570,#30571,#30572,#30573,#30574,#30575,#30576),.UNSPECIFIED.,.F.,.F.,
(4,3,3,3,3,3,3,3,3,3,3,4),(0.,0.125,0.1875,0.214870088595688,0.25,0.3125,
0.375,0.4375,0.5,0.5625,0.625,0.626108993264048),.UNSPECIFIED.);
#572=B_SPLINE_CURVE_WITH_KNOTS('',3,(#30578,#30579,#30580,#30581,#30582,
#30583,#30584,#30585),.UNSPECIFIED.,.F.,.F.,(4,1,1,1,1,4),(1.26755486773303E-5,
0.0625,0.125,0.25,0.375,0.5),.UNSPECIFIED.);
#573=B_SPLINE_CURVE_WITH_KNOTS('',3,(#30587,#30588,#30589,#30590,#30591,
#30592,#30593,#30594,#30595),.UNSPECIFIED.,.F.,.F.,(4,1,1,1,1,1,4),(0.500407782941687,
0.625,0.6875,0.75,0.8125,0.875,0.998506616626188),.UNSPECIFIED.);
#574=B_SPLINE_CURVE_WITH_KNOTS('',3,(#30597,#30598,#30599,#30600,#30601,
#30602,#30603,#30604,#30605,#30606,#30607,#30608,#30609,#30610,#30611,#30612),
 .UNSPECIFIED.,.F.,.F.,(4,3,3,3,3,4),(0.658192818009893,0.6875,0.71693403423044,
0.75,0.875,0.997625654344755),.UNSPECIFIED.);
#575=B_SPLINE_CURVE_WITH_KNOTS('',3,(#30614,#30615,#30616,#30617,#30618,
#30619,#30620,#30621,#30622,#30623,#30624,#30625,#30626,#30627,#30628,#30629,
#30630,#30631,#30632),.UNSPECIFIED.,.F.,.F.,(4,3,3,3,3,3,4),(0.39947571826055,
0.4375,0.5,0.53125,0.5625,0.625,0.658192818009893),.UNSPECIFIED.);
#576=B_SPLINE_CURVE_WITH_KNOTS('',3,(#30633,#30634,#30635,#30636,#30637,
#30638,#30639,#30640,#30641,#30642),.UNSPECIFIED.,.F.,.F.,(4,3,3,4),(0.293194800091934,
0.3125,0.375,0.39947571826055),.UNSPECIFIED.);
#577=B_SPLINE_CURVE_WITH_KNOTS('',3,(#30644,#30645,#30646,#30647,#30648,
#30649,#30650,#30651,#30652,#30653,#30654,#30655,#30656,#30657),
 .UNSPECIFIED.,.F.,.F.,(4,1,1,1,1,1,1,1,1,1,1,4),(0.298021461655708,0.3125,
0.375,0.5,0.625,0.75,0.8125,0.84375,0.875,0.90625,0.9375,1.),
 .UNSPECIFIED.);
#578=B_SPLINE_CURVE_WITH_KNOTS('',3,(#30660,#30661,#30662,#30663,#30664,
#30665,#30666,#30667,#30668,#30669,#30670,#30671,#30672,#30673,#30674,#30675,
#30676,#30677,#30678,#30679,#30680,#30681,#30682,#30683,#30684,#30685,#30686,
#30687,#30688,#30689,#30690,#30691,#30692,#30693,#30694,#30695,#30696),
 .UNSPECIFIED.,.F.,.F.,(4,3,3,3,3,3,3,3,3,3,3,3,4),(2.62189710416264E-7,
0.0625,0.09375,0.125,0.15625,0.1875,0.25,0.367359141751235,0.375,0.5,0.625,
0.6875,0.701590233395244),.UNSPECIFIED.);
#579=B_SPLINE_CURVE_WITH_KNOTS('',3,(#30698,#30699,#30700,#30701,#30702,
#30703,#30704,#30705,#30706,#30707,#30708,#30709,#30710,#30711),
 .UNSPECIFIED.,.F.,.F.,(4,1,1,1,1,1,1,1,1,1,1,4),(0.298831604432797,0.3125,
0.375,0.5,0.625,0.75,0.8125,0.84375,0.875,0.90625,0.9375,1.),
 .UNSPECIFIED.);
#580=B_SPLINE_CURVE_WITH_KNOTS('',3,(#30714,#30715,#30716,#30717,#30718,
#30719,#30720,#30721,#30722,#30723,#30724,#30725,#30726,#30727,#30728,#30729,
#30730,#30731,#30732,#30733,#30734,#30735,#30736,#30737,#30738,#30739,#30740,
#30741,#30742,#30743,#30744,#30745,#30746,#30747,#30748,#30749,#30750),
 .UNSPECIFIED.,.F.,.F.,(4,3,3,3,3,3,3,3,3,3,3,3,4),(2.66010736456726E-7,
0.0625,0.09375,0.125,0.15625,0.1875,0.25,0.365514712737838,0.375,0.5,0.625,
0.6875,0.700679367798627),.UNSPECIFIED.);
#581=B_SPLINE_CURVE_WITH_KNOTS('',3,(#30752,#30753,#30754,#30755,#30756,
#30757,#30758,#30759,#30760,#30761,#30762,#30763,#30764,#30765),
 .UNSPECIFIED.,.F.,.F.,(4,1,1,1,1,1,1,1,1,1,1,4),(0.299787333569703,0.3125,
0.375,0.5,0.625,0.75,0.8125,0.84375,0.875,0.90625,0.9375,1.),
 .UNSPECIFIED.);
#582=B_SPLINE_CURVE_WITH_KNOTS('',3,(#30768,#30769,#30770,#30771,#30772,
#30773,#30774,#30775,#30776,#30777,#30778,#30779,#30780,#30781,#30782,#30783,
#30784,#30785,#30786,#30787,#30788,#30789,#30790,#30791,#30792,#30793,#30794,
#30795,#30796,#30797,#30798,#30799,#30800,#30801,#30802,#30803,#30804),
 .UNSPECIFIED.,.F.,.F.,(4,3,3,3,3,3,3,3,3,3,3,3,4),(2.75012543287525E-7,
0.0625,0.09375,0.125,0.15625,0.1875,0.25,0.363598682235725,0.375,0.5,0.625,
0.6875,0.699678783356034),.UNSPECIFIED.);
#583=B_SPLINE_CURVE_WITH_KNOTS('',3,(#30806,#30807,#30808,#30809,#30810,
#30811,#30812,#30813,#30814,#30815,#30816,#30817,#30818,#30819),
 .UNSPECIFIED.,.F.,.F.,(4,1,1,1,1,1,1,1,1,1,1,4),(0.300810905459472,0.3125,
0.375,0.5,0.625,0.75,0.8125,0.84375,0.875,0.90625,0.9375,1.),
 .UNSPECIFIED.);
#584=B_SPLINE_CURVE_WITH_KNOTS('',3,(#30822,#30823,#30824,#30825,#30826,
#30827,#30828,#30829,#30830,#30831,#30832,#30833,#30834,#30835,#30836,#30837,
#30838,#30839,#30840,#30841,#30842,#30843,#30844,#30845,#30846,#30847,#30848,
#30849,#30850,#30851,#30852,#30853,#30854,#30855,#30856,#30857,#30858),
 .UNSPECIFIED.,.F.,.F.,(4,3,3,3,3,3,3,3,3,3,3,3,4),(2.7737565455879E-7,
0.0625,0.09375,0.125,0.15625,0.1875,0.25,0.361643443501042,0.375,0.5,0.625,
0.6875,0.698643471576761),.UNSPECIFIED.);
#585=B_SPLINE_CURVE_WITH_KNOTS('',3,(#30860,#30861,#30862,#30863,#30864,
#30865,#30866,#30867,#30868,#30869,#30870,#30871,#30872,#30873),
 .UNSPECIFIED.,.F.,.F.,(4,1,1,1,1,1,1,1,1,1,1,4),(0.301839172550323,0.3125,
0.375,0.5,0.625,0.75,0.8125,0.84375,0.875,0.90625,0.9375,1.),
 .UNSPECIFIED.);
#586=B_SPLINE_CURVE_WITH_KNOTS('',3,(#30876,#30877,#30878,#30879,#30880,
#30881,#30882,#30883,#30884,#30885,#30886,#30887,#30888,#30889,#30890,#30891,
#30892,#30893,#30894,#30895,#30896,#30897,#30898,#30899,#30900,#30901,#30902,
#30903,#30904,#30905,#30906,#30907,#30908,#30909,#30910,#30911,#30912),
 .UNSPECIFIED.,.F.,.F.,(4,3,3,3,3,3,3,3,3,3,3,3,4),(2.80962005521138E-7,
0.0625,0.09375,0.125,0.15625,0.1875,0.25,0.359695004612115,0.375,0.5,0.625,
0.6875,0.697655525115426),.UNSPECIFIED.);
#587=B_SPLINE_CURVE_WITH_KNOTS('',3,(#30914,#30915,#30916,#30917,#30918,
#30919,#30920,#30921,#30922,#30923,#30924,#30925,#30926,#30927),
 .UNSPECIFIED.,.F.,.F.,(4,1,1,1,1,1,1,1,1,1,1,4),(0.302853998408664,0.3125,
0.375,0.5,0.625,0.75,0.8125,0.84375,0.875,0.90625,0.9375,1.),
 .UNSPECIFIED.);
#588=B_SPLINE_CURVE_WITH_KNOTS('',3,(#30930,#30931,#30932,#30933,#30934,
#30935,#30936,#30937,#30938,#30939,#30940,#30941,#30942,#30943,#30944,#30945,
#30946,#30947,#30948,#30949,#30950,#30951,#30952,#30953,#30954,#30955,#30956,
#30957,#30958,#30959,#30960,#30961,#30962,#30963),.UNSPECIFIED.,.F.,.F.,
(4,3,3,3,3,3,3,3,3,3,3,4),(2.873516990008E-7,0.0625,0.09375,0.125,0.15625,
0.1875,0.25,0.357103578474147,0.375,0.5,0.625,0.694959544378405),
 .UNSPECIFIED.);
#589=B_SPLINE_CURVE_WITH_KNOTS('',3,(#30965,#30966,#30967,#30968,#30969,
#30970,#30971,#30972,#30973,#30974,#30975,#30976,#30977,#30978,#30979),
 .UNSPECIFIED.,.F.,.F.,(4,1,1,1,1,1,1,1,1,1,1,1,4),(0.304441335563685,0.3125,
0.375,0.5,0.625,0.6875,0.75,0.8125,0.84375,0.875,0.90625,0.9375,1.),
 .UNSPECIFIED.);
#590=B_SPLINE_CURVE_WITH_KNOTS('',3,(#30982,#30983,#30984,#30985,#30986,
#30987,#30988,#30989,#30990,#30991,#30992,#30993,#30994,#30995,#30996),
 .UNSPECIFIED.,.F.,.F.,(4,1,1,1,1,1,1,1,1,1,1,1,4),(2.84937768142854E-7,
0.0625,0.09375,0.125,0.15625,0.1875,0.25,0.3125,0.375,0.5,0.625,0.6875,
0.69476673108169),.UNSPECIFIED.);
#591=B_SPLINE_CURVE_WITH_KNOTS('',3,(#30998,#30999,#31000,#31001,#31002,
#31003,#31004,#31005,#31006,#31007,#31008,#31009,#31010,#31011,#31012),
 .UNSPECIFIED.,.F.,.F.,(4,1,1,1,1,1,1,1,1,1,1,1,4),(0.305513267453618,0.3125,
0.375,0.5,0.625,0.6875,0.75,0.8125,0.84375,0.875,0.90625,0.9375,1.),
 .UNSPECIFIED.);
#592=B_SPLINE_CURVE_WITH_KNOTS('',3,(#31015,#31016,#31017,#31018,#31019,
#31020,#31021,#31022,#31023,#31024,#31025,#31026,#31027,#31028,#31029),
 .UNSPECIFIED.,.F.,.F.,(4,1,1,1,1,1,1,1,1,1,1,1,4),(2.86307819456861E-7,
0.0625,0.09375,0.125,0.15625,0.1875,0.25,0.3125,0.375,0.5,0.625,0.6875,
0.693739351488113),.UNSPECIFIED.);
#593=B_SPLINE_CURVE_WITH_KNOTS('',3,(#31031,#31032,#31033,#31034,#31035,
#31036,#31037,#31038,#31039,#31040,#31041,#31042,#31043,#31044,#31045),
 .UNSPECIFIED.,.F.,.F.,(4,1,1,1,1,1,1,1,1,1,1,1,4),(0.306675627321796,0.3125,
0.375,0.5,0.625,0.6875,0.75,0.8125,0.84375,0.875,0.90625,0.9375,1.),
 .UNSPECIFIED.);
#594=B_SPLINE_CURVE_WITH_KNOTS('',3,(#31048,#31049,#31050,#31051,#31052,
#31053,#31054,#31055,#31056,#31057,#31058,#31059,#31060,#31061,#31062),
 .UNSPECIFIED.,.F.,.F.,(4,1,1,1,1,1,1,1,1,1,1,1,4),(2.94206060623265E-7,
0.0625,0.09375,0.125,0.15625,0.1875,0.25,0.3125,0.375,0.5,0.625,0.6875,
0.692733007429323),.UNSPECIFIED.);
#595=B_SPLINE_CURVE_WITH_KNOTS('',3,(#31064,#31065,#31066,#31067,#31068,
#31069,#31070,#31071,#31072,#31073,#31074,#31075,#31076,#31077,#31078),
 .UNSPECIFIED.,.F.,.F.,(4,1,1,1,1,1,1,1,1,1,1,1,4),(0.307485444826301,0.3125,
0.375,0.5,0.625,0.6875,0.75,0.8125,0.84375,0.875,0.90625,0.9375,1.),
 .UNSPECIFIED.);
#596=B_SPLINE_CURVE_WITH_KNOTS('',3,(#31081,#31082,#31083,#31084,#31085,
#31086,#31087,#31088,#31089,#31090,#31091,#31092,#31093,#31094,#31095,#31096,
#31097,#31098,#31099,#31100,#31101,#31102,#31103,#31104,#31105,#31106,#31107,
#31108,#31109,#31110,#31111,#31112,#31113,#31114,#31115,#31116,#31117,#31118,
#31119,#31120),.UNSPECIFIED.,.F.,.F.,(4,3,3,3,3,3,3,3,3,3,3,3,3,4),(3.05038783548285E-7,
0.0625,0.09375,0.125,0.15625,0.1875,0.25,0.3125,0.348312622039473,0.375,
0.5,0.625,0.6875,0.691764098829342),.UNSPECIFIED.);
#597=B_SPLINE_CURVE_WITH_KNOTS('',3,(#31122,#31123,#31124,#31125,#31126,
#31127,#31128,#31129,#31130,#31131,#31132,#31133,#31134,#31135,#31136),
 .UNSPECIFIED.,.F.,.F.,(4,1,1,1,1,1,1,1,1,1,1,1,4),(0.308404661026527,0.3125,
0.375,0.5,0.625,0.6875,0.75,0.8125,0.84375,0.875,0.90625,0.9375,1.),
 .UNSPECIFIED.);
#598=B_SPLINE_CURVE_WITH_KNOTS('',3,(#31139,#31140,#31141,#31142,#31143,
#31144,#31145,#31146,#31147,#31148,#31149,#31150,#31151,#31152,#31153,#31154,
#31155,#31156,#31157,#31158,#31159,#31160,#31161,#31162,#31163,#31164,#31165,
#31166,#31167,#31168,#31169,#31170,#31171,#31172,#31173,#31174,#31175,#31176,
#31177,#31178),.UNSPECIFIED.,.F.,.F.,(4,3,3,3,3,3,3,3,3,3,3,3,3,4),(2.88155531850153E-7,
0.0625,0.09375,0.125,0.15625,0.1875,0.25,0.3125,0.346342722159355,0.375,
0.5,0.625,0.6875,0.690961556714303),.UNSPECIFIED.);
#599=B_SPLINE_CURVE_WITH_KNOTS('',3,(#31180,#31181,#31182,#31183,#31184,
#31185,#31186,#31187,#31188,#31189,#31190,#31191,#31192,#31193),
 .UNSPECIFIED.,.F.,.F.,(4,1,1,1,1,1,1,1,1,1,1,4),(0.302671489156909,0.3125,
0.375,0.5,0.625,0.75,0.8125,0.84375,0.875,0.90625,0.9375,1.),
 .UNSPECIFIED.);
#600=B_SPLINE_CURVE_WITH_KNOTS('',3,(#31197,#31198,#31199,#31200,#31201,
#31202,#31203,#31204,#31205,#31206,#31207,#31208,#31209,#31210,#31211,#31212,
#31213,#31214,#31215,#31216,#31217,#31218,#31219,#31220,#31221,#31222,#31223,
#31224),.UNSPECIFIED.,.F.,.F.,(4,3,3,3,3,3,3,3,3,4),(0.,0.0625,0.09375,
0.125,0.15625,0.1875,0.25,0.364633141489333,0.375,0.499908337236844),
 .UNSPECIFIED.);
#601=B_SPLINE_CURVE_WITH_KNOTS('',3,(#31225,#31226,#31227,#31228,#31229,
#31230,#31231,#31232,#31233,#31234),.UNSPECIFIED.,.F.,.F.,(4,3,3,4),(0.5,
0.625,0.6875,0.699974107082008),.UNSPECIFIED.);
#602=B_SPLINE_CURVE_WITH_KNOTS('',3,(#31236,#31237,#31238,#31239,#31240,
#31241,#31242,#31243,#31244,#31245),.UNSPECIFIED.,.F.,.F.,(4,3,3,4),(0.295540353636982,
0.3125,0.375,0.5),.UNSPECIFIED.);
#603=B_SPLINE_CURVE_WITH_KNOTS('',3,(#31247,#31248,#31249,#31250,#31251,
#31252,#31253,#31254,#31255,#31256,#31257,#31258,#31259,#31260,#31261,#31262,
#31263,#31264,#31265,#31266,#31267,#31268,#31269,#31270,#31271),
 .UNSPECIFIED.,.F.,.F.,(4,3,3,3,3,3,3,3,4),(0.500189461797682,0.625,0.75,
0.8125,0.84375,0.875,0.90625,0.9375,0.999997786243782),.UNSPECIFIED.);
#604=B_SPLINE_CURVE_WITH_KNOTS('',3,(#31273,#31274,#31275,#31276,#31277,
#31278,#31279,#31280),.UNSPECIFIED.,.F.,.F.,(4,1,1,1,1,4),(0.,0.0625,0.125,
0.25,0.375,0.5),.UNSPECIFIED.);
#605=B_SPLINE_CURVE_WITH_KNOTS('',3,(#31282,#31283,#31284,#31285,#31286,
#31287,#31288,#31289,#31290),.UNSPECIFIED.,.F.,.F.,(4,1,1,1,1,1,4),(0.500434798583671,
0.625,0.6875,0.75,0.8125,0.875,0.999998086846501),.UNSPECIFIED.);
#606=B_SPLINE_CURVE_WITH_KNOTS('',3,(#31291,#31292,#31293,#31294,#31295,
#31296,#31297,#31298,#31299,#31300,#31301,#31302,#31303),.UNSPECIFIED.,
 .F.,.F.,(4,1,1,1,1,1,1,1,1,1,4),(0.,0.0625,0.09375,0.125,0.15625,0.1875,
0.25,0.375,0.5,0.625,0.71355566892686),.UNSPECIFIED.);
#607=B_SPLINE_CURVE_WITH_KNOTS('',3,(#31305,#31306,#31307,#31308,#31309),
 .UNSPECIFIED.,.F.,.F.,(4,1,4),(0.271066582727647,0.375,0.4994045688759),
 .UNSPECIFIED.);
#608=B_SPLINE_CURVE_WITH_KNOTS('',3,(#31311,#31312,#31313,#31314,#31315,
#31316,#31317,#31318,#31319,#31320,#31321,#31322),.UNSPECIFIED.,.F.,.F.,
(4,1,1,1,1,1,1,1,1,4),(0.4994045688759,0.5,0.625,0.75,0.8125,0.84375,0.875,
0.90625,0.9375,1.),.UNSPECIFIED.);
#609=B_SPLINE_CURVE_WITH_KNOTS('',3,(#31324,#31325,#31326,#31327,#31328,
#31329,#31330,#31331,#31332,#31333,#31334,#31335,#31336,#31337,#31338,#31339,
#31340,#31341,#31342,#31343,#31344,#31345,#31346,#31347,#31348,#31349,#31350,
#31351,#31352,#31353,#31354),.UNSPECIFIED.,.F.,.F.,(4,3,3,3,3,3,3,3,3,3,
4),(1.20911684619388E-6,0.125,0.25,0.375,0.5,0.625,0.6875,0.75,0.8125,0.875,
0.999824037442535),.UNSPECIFIED.);
#610=B_SPLINE_CURVE_WITH_KNOTS('',3,(#31356,#31357,#31358,#31359,#31360,
#31361,#31362,#31363,#31364,#31365,#31366,#31367),.UNSPECIFIED.,.F.,.F.,
(4,1,1,1,1,1,1,1,1,4),(1.15789001547902E-5,0.0625,0.09375,0.125,0.15625,
0.1875,0.25,0.3125,0.375,0.463468292977054),.UNSPECIFIED.);
#611=B_SPLINE_CURVE_WITH_KNOTS('',3,(#31368,#31369,#31370,#31371,#31372,
#31373),.UNSPECIFIED.,.F.,.F.,(4,1,1,4),(0.463468292977054,0.5,0.625,0.743178274051315),
 .UNSPECIFIED.);
#612=B_SPLINE_CURVE_WITH_KNOTS('',3,(#31375,#31376,#31377,#31378,#31379),
 .UNSPECIFIED.,.F.,.F.,(4,1,4),(0.256944255797255,0.375,0.499319773304833),
 .UNSPECIFIED.);
#613=B_SPLINE_CURVE_WITH_KNOTS('',3,(#31381,#31382,#31383,#31384,#31385,
#31386,#31387,#31388,#31389,#31390,#31391,#31392,#31393),.UNSPECIFIED.,
 .F.,.F.,(4,1,1,1,1,1,1,1,1,1,4),(0.499319773304833,0.5,0.625,0.6875,0.75,
0.8125,0.84375,0.875,0.90625,0.9375,1.),.UNSPECIFIED.);
#614=B_SPLINE_CURVE_WITH_KNOTS('',3,(#31397,#31398,#31399,#31400,#31401,
#31402,#31403,#31404,#31405,#31406,#31407,#31408),.UNSPECIFIED.,.F.,.F.,
(4,1,1,1,1,1,1,1,1,4),(0.,0.0625,0.09375,0.125,0.15625,0.1875,0.25,0.3125,
0.375,0.5),.UNSPECIFIED.);
#615=B_SPLINE_CURVE_WITH_KNOTS('',3,(#31409,#31410,#31411,#31412,#31413),
 .UNSPECIFIED.,.F.,.F.,(4,1,4),(0.5,0.625,0.742719765959379),
 .UNSPECIFIED.);
#616=B_SPLINE_CURVE_WITH_KNOTS('',3,(#31415,#31416,#31417,#31418,#31419),
 .UNSPECIFIED.,.F.,.F.,(4,1,4),(0.257506245398161,0.375,0.499318574492738),
 .UNSPECIFIED.);
#617=B_SPLINE_CURVE_WITH_KNOTS('',3,(#31421,#31422,#31423,#31424,#31425,
#31426,#31427,#31428,#31429,#31430,#31431,#31432,#31433),.UNSPECIFIED.,
 .F.,.F.,(4,1,1,1,1,1,1,1,1,1,4),(0.499318574492738,0.5,0.625,0.6875,0.75,
0.8125,0.84375,0.875,0.90625,0.9375,1.),.UNSPECIFIED.);
#618=B_SPLINE_CURVE_WITH_KNOTS('',3,(#31437,#31438,#31439,#31440,#31441,
#31442,#31443,#31444,#31445,#31446,#31447,#31448),.UNSPECIFIED.,.F.,.F.,
(4,1,1,1,1,1,1,1,1,4),(0.,0.0625,0.09375,0.125,0.15625,0.1875,0.25,0.3125,
0.375,0.5),.UNSPECIFIED.);
#619=B_SPLINE_CURVE_WITH_KNOTS('',3,(#31449,#31450,#31451,#31452,#31453),
 .UNSPECIFIED.,.F.,.F.,(4,1,4),(0.5,0.625,0.742143863244383),
 .UNSPECIFIED.);
#620=B_SPLINE_CURVE_WITH_KNOTS('',3,(#31455,#31456,#31457,#31458,#31459,
#31460,#31461),.UNSPECIFIED.,.F.,.F.,(4,3,4),(0.339613136872108,0.375,0.499997657275256),
 .UNSPECIFIED.);
#621=B_SPLINE_CURVE_WITH_KNOTS('',3,(#31463,#31464,#31465,#31466,#31467,
#31468,#31469,#31470,#31471,#31472,#31473,#31474,#31475,#31476,#31477,#31478),
 .UNSPECIFIED.,.F.,.F.,(4,3,3,3,3,4),(0.5,0.625,0.718785408996563,0.75,
0.875,1.),.UNSPECIFIED.);
#622=B_SPLINE_CURVE_WITH_KNOTS('',3,(#31480,#31481,#31482,#31483,#31484,
#31485,#31486,#31487,#31488,#31489,#31490,#31491,#31492,#31493,#31494,#31495,
#31496,#31497,#31498,#31499,#31500,#31501,#31502,#31503,#31504),
 .UNSPECIFIED.,.F.,.F.,(4,3,3,3,3,3,3,3,4),(0.125,0.25,0.3125,0.375,0.4375,
0.5,0.625,0.75,1.),.UNSPECIFIED.);
#623=B_SPLINE_CURVE_WITH_KNOTS('',3,(#31506,#31507,#31508,#31509),
 .UNSPECIFIED.,.F.,.F.,(4,4),(9.19960507825898E-5,0.125),.UNSPECIFIED.);
#624=B_SPLINE_CURVE_WITH_KNOTS('',3,(#31511,#31512,#31513,#31514,#31515,
#31516,#31517),.UNSPECIFIED.,.F.,.F.,(4,3,4),(4.03926038141589E-9,0.621738318522071,
0.999999432402183),.UNSPECIFIED.);
#625=B_SPLINE_CURVE_WITH_KNOTS('',3,(#31519,#31520,#31521,#31522,#31523,
#31524,#31525,#31526,#31527,#31528,#31529,#31530,#31531,#31532,#31533,#31534),
 .UNSPECIFIED.,.F.,.F.,(4,3,3,3,3,4),(0.,0.25,0.5,0.625,0.75,0.999999984180473),
 .UNSPECIFIED.);
#626=B_SPLINE_CURVE_WITH_KNOTS('',3,(#31540,#31541,#31542,#31543,#31544,
#31545,#31546,#31547,#31548,#31549,#31550,#31551,#31552,#31553,#31554,#31555,
#31556,#31557,#31558,#31559,#31560,#31561,#31562,#31563,#31564,#31565,#31566,
#31567),.UNSPECIFIED.,.F.,.F.,(4,3,3,3,3,3,3,3,3,4),(0.,0.25,0.375,0.5,
0.625,0.6875,0.75,0.8125,0.875,0.999999996427379),.UNSPECIFIED.);
#627=B_SPLINE_CURVE_WITH_KNOTS('',3,(#31569,#31570,#31571,#31572,#31573,
#31574,#31575,#31576,#31577,#31578,#31579,#31580,#31581,#31582,#31583,#31584,
#31585,#31586,#31587,#31588,#31589,#31590),.UNSPECIFIED.,.F.,.F.,(4,3,3,
3,3,3,3,4),(5.11212140420089E-8,0.0625,0.09375,0.125,0.15625,0.1875,0.25,
0.251514333796608),.UNSPECIFIED.);
#628=B_SPLINE_CURVE_WITH_KNOTS('',3,(#31592,#31593,#31594,#31595,#31596,
#31597,#31598,#31599,#31600,#31601,#31602,#31603,#31604,#31605,#31606,#31607),
 .UNSPECIFIED.,.F.,.F.,(4,3,3,3,3,4),(0.251514333796608,0.3125,0.375,0.4375,
0.5,0.508539107283651),.UNSPECIFIED.);
#629=B_SPLINE_CURVE_WITH_KNOTS('',3,(#31609,#31610,#31611,#31612,#31613,
#31614,#31615,#31616,#31617,#31618,#31619,#31620,#31621,#31622,#31623,#31624),
 .UNSPECIFIED.,.F.,.F.,(4,3,3,3,3,4),(0.508539107283651,0.5275897246703,
0.625,0.75,0.875,1.),.UNSPECIFIED.);
#630=B_SPLINE_CURVE_WITH_KNOTS('',3,(#31626,#31627,#31628,#31629,#31630,
#31631,#31632,#31633,#31634,#31635,#31636,#31637,#31638,#31639,#31640,#31641,
#31642,#31643,#31644,#31645,#31646,#31647,#31648,#31649,#31650,#31651,#31652,
#31653,#31654,#31655,#31656,#31657,#31658,#31659,#31660,#31661,#31662,#31663,
#31664,#31665,#31666,#31667,#31668,#31669,#31670,#31671,#31672,#31673,#31674,
#31675,#31676,#31677,#31678,#31679,#31680,#31681,#31682,#31683,#31684,#31685,
#31686,#31687,#31688,#31689,#31690,#31691,#31692,#31693,#31694,#31695,#31696,
#31697,#31698,#31699,#31700,#31701,#31702,#31703,#31704,#31705,#31706,#31707,
#31708,#31709,#31710,#31711,#31712,#31713,#31714,#31715,#31716,#31717,#31718,
#31719,#31720,#31721,#31722,#31723,#31724,#31725,#31726,#31727,#31728,#31729,
#31730,#31731,#31732,#31733,#31734,#31735,#31736,#31737,#31738,#31739,#31740,
#31741,#31742,#31743,#31744,#31745,#31746,#31747,#31748,#31749,#31750,#31751,
#31752,#31753,#31754,#31755,#31756,#31757,#31758,#31759,#31760,#31761,#31762,
#31763,#31764,#31765,#31766,#31767,#31768,#31769,#31770,#31771,#31772,#31773,
#31774,#31775,#31776,#31777,#31778,#31779,#31780,#31781,#31782,#31783,#31784,
#31785),.UNSPECIFIED.,.F.,.F.,(4,3,3,3,3,3,3,3,3,3,3,3,3,3,3,3,3,3,3,3,
3,3,3,3,3,3,3,3,3,3,3,3,3,3,3,3,3,3,3,3,3,3,3,3,3,3,3,3,3,3,3,3,3,4),(0.,
0.03125,0.046875,0.0546875,0.0625,0.0703125,0.078125,0.09375,0.109375,0.125,
0.134813898918915,0.140625,0.15625,0.171875,0.1875,0.203125,0.21875,0.234375,
0.25,0.28125,0.296875,0.3125,0.328125,0.34375,0.356926011470558,0.359375,
0.375,0.390625,0.40625,0.421875,0.4375,0.46875,0.5,0.53125,0.5625,0.59375,
0.625,0.626999867348899,0.6875,0.75,0.8125,0.84375,0.855575696034116,0.875,
0.90625,0.921875,0.929958125829058,0.9375,0.953125,0.9609375,0.96875,0.9765625,
0.984375,0.999999930559409),.UNSPECIFIED.);
#631=B_SPLINE_CURVE_WITH_KNOTS('',3,(#31787,#31788,#31789,#31790,#31791,
#31792,#31793,#31794,#31795,#31796,#31797,#31798,#31799,#31800,#31801,#31802,
#31803,#31804,#31805,#31806,#31807,#31808,#31809,#31810,#31811,#31812,#31813,
#31814,#31815,#31816,#31817,#31818,#31819,#31820,#31821,#31822,#31823,#31824,
#31825,#31826,#31827,#31828,#31829,#31830,#31831,#31832,#31833,#31834,#31835,
#31836,#31837,#31838,#31839),.UNSPECIFIED.,.F.,.F.,(4,1,1,1,1,1,1,1,1,1,
1,1,1,1,1,1,1,1,1,1,1,1,1,1,1,1,1,1,1,1,1,1,1,1,1,1,1,1,1,1,1,1,1,1,1,1,
1,1,1,1,4),(2.33524176194205E-8,0.015625,0.0234375,0.03125,0.0390625,0.046875,
0.0625,0.078125,0.09375,0.125,0.15625,0.1875,0.25,0.3125,0.375,0.40625,
0.4375,0.46875,0.484375,0.5,0.515625,0.53125,0.5625,0.578125,0.59375,0.609375,
0.625,0.640625,0.65625,0.671875,0.6875,0.703125,0.71875,0.75,0.765625,0.78125,
0.796875,0.8125,0.828125,0.84375,0.859375,0.875,0.890625,0.90625,0.921875,
0.9296875,0.9375,0.9453125,0.953125,0.96875,1.),.UNSPECIFIED.);
#632=B_SPLINE_CURVE_WITH_KNOTS('',3,(#31841,#31842,#31843,#31844,#31845,
#31846,#31847,#31848,#31849,#31850,#31851,#31852,#31853,#31854,#31855,#31856),
 .UNSPECIFIED.,.F.,.F.,(4,3,3,3,3,4),(0.,0.125,0.25,0.375,0.4375,0.461967251686174),
 .UNSPECIFIED.);
#633=B_SPLINE_CURVE_WITH_KNOTS('',3,(#31858,#31859,#31860,#31861,#31862,
#31863,#31864,#31865,#31866,#31867,#31868,#31869,#31870,#31871,#31872,#31873),
 .UNSPECIFIED.,.F.,.F.,(4,3,3,3,3,4),(0.461967251686174,0.5,0.5625,0.625,
0.6875,0.748603143222001),.UNSPECIFIED.);
#634=B_SPLINE_CURVE_WITH_KNOTS('',3,(#31875,#31876,#31877,#31878,#31879,
#31880,#31881,#31882,#31883,#31884,#31885,#31886,#31887,#31888,#31889,#31890,
#31891,#31892,#31893,#31894,#31895,#31896),.UNSPECIFIED.,.F.,.F.,(4,3,3,
3,3,3,3,4),(0.748603143222001,0.75,0.8125,0.84375,0.875,0.90625,0.9375,
0.999999927233155),.UNSPECIFIED.);
#635=B_SPLINE_CURVE_WITH_KNOTS('',3,(#31898,#31899,#31900,#31901,#31902,
#31903,#31904,#31905,#31906),.UNSPECIFIED.,.F.,.F.,(4,1,1,1,1,1,4),(0.,
0.125,0.25,0.5,0.625,0.75,1.),.UNSPECIFIED.);
#636=B_SPLINE_CURVE_WITH_KNOTS('',3,(#31914,#31915,#31916,#31917,#31918,
#31919,#31920),.UNSPECIFIED.,.F.,.F.,(4,3,4),(0.028486178614514,0.5,1.),
 .UNSPECIFIED.);
#637=B_SPLINE_CURVE_WITH_KNOTS('',3,(#31922,#31923,#31924,#31925),
 .UNSPECIFIED.,.F.,.F.,(4,4),(0.,0.028486178614514),.UNSPECIFIED.);
#638=B_SPLINE_CURVE_WITH_KNOTS('',3,(#31927,#31928,#31929,#31930),
 .UNSPECIFIED.,.F.,.F.,(4,4),(0.875,1.),.UNSPECIFIED.);
#639=B_SPLINE_CURVE_WITH_KNOTS('',3,(#31932,#31933,#31934,#31935,#31936,
#31937,#31938,#31939,#31940,#31941,#31942,#31943,#31944,#31945,#31946,#31947,
#31948,#31949,#31950,#31951,#31952,#31953,#31954,#31955,#31956),
 .UNSPECIFIED.,.F.,.F.,(4,3,3,3,3,3,3,3,4),(0.,0.25,0.375,0.5,0.5625,0.625,
0.6875,0.75,0.875),.UNSPECIFIED.);
#640=B_SPLINE_CURVE_WITH_KNOTS('',3,(#31958,#31959,#31960,#31961,#31962,
#31963,#31964,#31965,#31966,#31967,#31968,#31969,#31970),.UNSPECIFIED.,
 .F.,.F.,(4,3,3,3,4),(0.,0.125,0.25,0.279719843926451,0.375),
 .UNSPECIFIED.);
#641=B_SPLINE_CURVE_WITH_KNOTS('',3,(#31972,#31973,#31974,#31975,#31976,
#31977,#31978,#31979,#31980,#31981,#31982,#31983,#31984,#31985,#31986,#31987,
#31988,#31989,#31990,#31991,#31992,#31993),.UNSPECIFIED.,.F.,.F.,(4,3,3,
3,3,3,3,4),(0.375,0.5,0.625,0.6875,0.75,0.8125,0.875,1.),.UNSPECIFIED.);
#642=B_SPLINE_CURVE_WITH_KNOTS('',3,(#31995,#31996,#31997,#31998,#31999,
#32000,#32001,#32002,#32003,#32004,#32005,#32006,#32007,#32008,#32009,#32010,
#32011,#32012,#32013),.UNSPECIFIED.,.F.,.F.,(4,3,3,3,3,3,4),(8.04807277738882E-5,
0.125,0.1875,0.25,0.3125,0.375,0.5),.UNSPECIFIED.);
#643=B_SPLINE_CURVE_WITH_KNOTS('',3,(#32015,#32016,#32017,#32018,#32019,
#32020,#32021,#32022,#32023,#32024,#32025,#32026,#32027),.UNSPECIFIED.,
 .F.,.F.,(4,3,3,3,4),(0.500165768693434,0.732349597796809,0.75,0.875,1.),
 .UNSPECIFIED.);
#644=B_SPLINE_CURVE_WITH_KNOTS('',3,(#32029,#32030,#32031,#32032,#32033,
#32034,#32035,#32036,#32037,#32038,#32039,#32040,#32041,#32042,#32043,#32044,
#32045,#32046,#32047,#32048,#32049,#32050,#32051,#32052,#32053,#32054,#32055,
#32056),.UNSPECIFIED.,.F.,.F.,(4,3,3,3,3,3,3,3,3,4),(1.05884092999222E-5,
0.125,0.25,0.3125,0.375,0.4375,0.5,0.625,0.75,1.),.UNSPECIFIED.);
#645=B_SPLINE_CURVE_WITH_KNOTS('',3,(#32058,#32059,#32060,#32061,#32062,
#32063,#32064),.UNSPECIFIED.,.F.,.F.,(4,3,4),(0.,0.5,0.999998285932114),
 .UNSPECIFIED.);
#646=B_SPLINE_CURVE_WITH_KNOTS('',3,(#32066,#32067,#32068,#32069,#32070,
#32071,#32072,#32073,#32074,#32075),.UNSPECIFIED.,.F.,.F.,(4,3,3,4),(0.,
0.5,0.75,1.),.UNSPECIFIED.);
#647=B_SPLINE_CURVE_WITH_KNOTS('',3,(#32081,#32082,#32083,#32084,#32085,
#32086,#32087),.UNSPECIFIED.,.F.,.F.,(4,3,4),(9.24712860392496E-13,0.5,
1.),.UNSPECIFIED.);
#648=B_SPLINE_CURVE_WITH_KNOTS('',3,(#32089,#32090,#32091,#32092,#32093,
#32094,#32095,#32096,#32097,#32098,#32099,#32100,#32101,#32102,#32103,#32104,
#32105,#32106,#32107),.UNSPECIFIED.,.F.,.F.,(4,1,1,1,1,1,1,1,1,1,1,1,1,
1,1,1,4),(0.000133962196229911,0.0625,0.09375,0.125,0.15625,0.1875,0.25,
0.375,0.4375,0.5,0.5625,0.625,0.6875,0.75,0.8125,0.875,1.),
 .UNSPECIFIED.);
#649=B_SPLINE_CURVE_WITH_KNOTS('',3,(#32109,#32110,#32111,#32112,#32113,
#32114,#32115,#32116,#32117,#32118,#32119,#32120,#32121,#32122,#32123,#32124,
#32125,#32126,#32127,#32128,#32129,#32130,#32131,#32132,#32133,#32134,#32135,
#32136,#32137,#32138,#32139,#32140,#32141,#32142,#32143,#32144,#32145,#32146,
#32147,#32148,#32149,#32150,#32151,#32152,#32153,#32154,#32155,#32156,#32157,
#32158,#32159,#32160,#32161,#32162,#32163,#32164,#32165,#32166,#32167,#32168,
#32169,#32170,#32171,#32172,#32173,#32174,#32175,#32176,#32177,#32178,#32179,
#32180,#32181,#32182,#32183,#32184,#32185,#32186,#32187,#32188,#32189,#32190,
#32191,#32192,#32193,#32194,#32195,#32196,#32197,#32198,#32199,#32200,#32201,
#32202,#32203,#32204,#32205,#32206,#32207,#32208,#32209,#32210,#32211,#32212,
#32213,#32214,#32215,#32216,#32217,#32218,#32219,#32220,#32221,#32222,#32223,
#32224,#32225,#32226,#32227,#32228,#32229,#32230,#32231,#32232,#32233,#32234,
#32235,#32236,#32237,#32238,#32239,#32240,#32241,#32242,#32243,#32244,#32245,
#32246,#32247,#32248,#32249,#32250,#32251,#32252,#32253,#32254,#32255,#32256,
#32257,#32258,#32259,#32260,#32261,#32262,#32263,#32264,#32265,#32266,#32267,
#32268,#32269,#32270,#32271),.UNSPECIFIED.,.F.,.F.,(4,3,3,3,3,3,3,3,3,3,
3,3,3,3,3,3,3,3,3,3,3,3,3,3,3,3,3,3,3,3,3,3,3,3,3,3,3,3,3,3,3,3,3,3,3,3,
3,3,3,3,3,3,3,3,4),(0.,0.03125,0.046875,0.0546875,0.0625,0.0703125,0.078125,
0.09375,0.109375,0.125,0.132706893319552,0.140625,0.15625,0.171875,0.1875,
0.203125,0.21875,0.234375,0.25,0.28125,0.296875,0.3125,0.328125,0.34375,
0.354656215967293,0.359375,0.375,0.390625,0.40625,0.421875,0.4375,0.453125,
0.46875,0.484375,0.5,0.53125,0.5625,0.59375,0.625,0.627549721648294,0.65625,
0.6875,0.75,0.8125,0.84375,0.85684618431259,0.875,0.90625,0.921875,0.930906239968274,
0.9375,0.953125,0.96875,0.984375,0.999999864466775),.UNSPECIFIED.);
#650=B_SPLINE_CURVE_WITH_KNOTS('',3,(#32272,#32273,#32274,#32275,#32276,
#32277,#32278,#32279,#32280,#32281,#32282),.UNSPECIFIED.,.F.,.F.,(4,1,1,
1,1,1,1,1,4),(6.13123545891853E-8,0.015625,0.03125,0.046875,0.0625,0.078125,
0.09375,0.125,0.142413158676735),.UNSPECIFIED.);
#651=B_SPLINE_CURVE_WITH_KNOTS('',3,(#32287,#32288,#32289,#32290,#32291,
#32292),.UNSPECIFIED.,.F.,.F.,(4,2,4),(-0.386868606697558,-0.228081755753299,
-0.000106832852268002),.UNSPECIFIED.);
#652=B_SPLINE_CURVE_WITH_KNOTS('',3,(#32294,#32295,#32296,#32297,#32298,
#32299,#32300,#32301,#32302,#32303,#32304,#32305,#32306,#32307,#32308,#32309,
#32310,#32311,#32312),.UNSPECIFIED.,.F.,.F.,(4,1,1,1,1,1,1,1,1,1,1,1,1,
1,1,1,4),(0.,0.125,0.1875,0.21875,0.25,0.28125,0.3125,0.375,0.5,0.625,0.75,
0.8125,0.84375,0.875,0.90625,0.9375,1.),.UNSPECIFIED.);
#653=B_SPLINE_CURVE_WITH_KNOTS('',3,(#32316,#32317,#32318,#32319,#32320,
#32321,#32322,#32323,#32324,#32325,#32326,#32327,#32328,#32329,#32330,#32331,
#32332,#32333,#32334,#32335,#32336,#32337,#32338,#32339,#32340,#32341,#32342,
#32343,#32344,#32345,#32346,#32347,#32348,#32349,#32350,#32351,#32352,#32353,
#32354,#32355,#32356,#32357,#32358,#32359,#32360,#32361),.UNSPECIFIED.,
 .F.,.F.,(4,3,3,3,3,3,3,3,3,3,3,3,3,3,3,4),(2.87286426861497E-7,0.0625,
0.09375,0.125,0.15625,0.1875,0.25,0.357099507040325,0.375,0.5,0.625,0.75,
0.8125,0.84375,0.875,0.999999985631448),.UNSPECIFIED.);
#654=B_SPLINE_CURVE_WITH_KNOTS('',3,(#32362,#32363,#32364,#32365,#32366,
#32367,#32368,#32369,#32370,#32371,#32372,#32373,#32374,#32375,#32376,#32377,
#32378,#32379,#32380,#32381,#32382),.UNSPECIFIED.,.F.,.F.,(4,1,1,1,1,1,
1,1,1,1,1,1,1,1,1,1,1,1,4),(0.,0.0625,0.09375,0.125,0.15625,0.1875,0.25,
0.3125,0.375,0.5,0.625,0.6875,0.75,0.8125,0.84375,0.875,0.90625,0.9375,
0.999999797571635),.UNSPECIFIED.);
#655=B_SPLINE_CURVE_WITH_KNOTS('',3,(#32387,#32388,#32389,#32390,#32391,
#32392,#32393,#32394,#32395,#32396,#32397,#32398,#32399,#32400,#32401,#32402,
#32403,#32404,#32405,#32406,#32407),.UNSPECIFIED.,.F.,.F.,(4,1,1,1,1,1,
1,1,1,1,1,1,1,1,1,1,1,1,4),(2.78773030124088E-7,0.0625,0.09375,0.125,0.15625,
0.1875,0.25,0.3125,0.375,0.5,0.625,0.6875,0.75,0.8125,0.84375,0.875,0.90625,
0.9375,0.999999822301832),.UNSPECIFIED.);
#656=B_SPLINE_CURVE_WITH_KNOTS('',3,(#32409,#32410,#32411,#32412,#32413,
#32414,#32415,#32416,#32417,#32418,#32419,#32420,#32421,#32422,#32423,#32424,
#32425,#32426,#32427,#32428,#32429),.UNSPECIFIED.,.F.,.F.,(4,1,1,1,1,1,
1,1,1,1,1,1,1,1,1,1,1,1,4),(0.,0.0625,0.09375,0.125,0.15625,0.1875,0.25,
0.3125,0.375,0.5,0.625,0.6875,0.75,0.8125,0.84375,0.875,0.90625,0.9375,
1.),.UNSPECIFIED.);
#657=B_SPLINE_CURVE_WITH_KNOTS('',3,(#32433,#32434,#32435,#32436,#32437,
#32438,#32439,#32440,#32441,#32442,#32443,#32444,#32445,#32446,#32447,#32448,
#32449,#32450,#32451,#32452,#32453),.UNSPECIFIED.,.F.,.F.,(4,1,1,1,1,1,
1,1,1,1,1,1,1,1,1,1,1,1,4),(2.8501534152819E-7,0.0625,0.09375,0.125,0.15625,
0.1875,0.25,0.3125,0.375,0.5,0.625,0.6875,0.75,0.8125,0.84375,0.875,0.90625,
0.9375,1.),.UNSPECIFIED.);
#658=B_SPLINE_CURVE_WITH_KNOTS('',3,(#32454,#32455,#32456,#32457,#32458,
#32459,#32460,#32461,#32462,#32463,#32464,#32465,#32466,#32467,#32468,#32469,
#32470,#32471,#32472,#32473,#32474),.UNSPECIFIED.,.F.,.F.,(4,1,1,1,1,1,
1,1,1,1,1,1,1,1,1,1,1,1,4),(1.11184293768699E-8,0.0625,0.09375,0.125,0.15625,
0.1875,0.25,0.3125,0.375,0.5,0.625,0.6875,0.75,0.8125,0.84375,0.875,0.90625,
0.9375,0.999999806772229),.UNSPECIFIED.);
#659=B_SPLINE_CURVE_WITH_KNOTS('',3,(#32479,#32480,#32481,#32482,#32483,
#32484,#32485,#32486,#32487,#32488,#32489,#32490,#32491,#32492,#32493,#32494,
#32495,#32496,#32497,#32498,#32499),.UNSPECIFIED.,.F.,.F.,(4,1,1,1,1,1,
1,1,1,1,1,1,1,1,1,1,1,1,4),(2.82686142298943E-7,0.0625,0.09375,0.125,0.15625,
0.1875,0.25,0.3125,0.375,0.5,0.625,0.6875,0.75,0.8125,0.84375,0.875,0.90625,
0.9375,0.999999781697572),.UNSPECIFIED.);
#660=B_SPLINE_CURVE_WITH_KNOTS('',3,(#32501,#32502,#32503,#32504,#32505,
#32506,#32507,#32508,#32509,#32510,#32511,#32512,#32513,#32514,#32515,#32516,
#32517,#32518,#32519,#32520,#32521),.UNSPECIFIED.,.F.,.F.,(4,1,1,1,1,1,
1,1,1,1,1,1,1,1,1,1,1,1,4),(0.,0.0625,0.09375,0.125,0.15625,0.1875,0.25,
0.3125,0.375,0.5,0.625,0.6875,0.75,0.8125,0.84375,0.875,0.90625,0.9375,
1.),.UNSPECIFIED.);
#661=B_SPLINE_CURVE_WITH_KNOTS('',3,(#32525,#32526,#32527,#32528,#32529,
#32530,#32531,#32532,#32533,#32534,#32535,#32536,#32537,#32538,#32539,#32540,
#32541,#32542,#32543,#32544,#32545),.UNSPECIFIED.,.F.,.F.,(4,1,1,1,1,1,
1,1,1,1,1,1,1,1,1,1,1,1,4),(2.86446402154255E-7,0.0625,0.09375,0.125,0.15625,
0.1875,0.25,0.3125,0.375,0.5,0.625,0.6875,0.75,0.8125,0.84375,0.875,0.90625,
0.9375,1.),.UNSPECIFIED.);
#662=B_SPLINE_CURVE_WITH_KNOTS('',3,(#32546,#32547,#32548,#32549,#32550,
#32551,#32552,#32553,#32554,#32555,#32556,#32557,#32558,#32559,#32560,#32561,
#32562,#32563,#32564,#32565,#32566,#32567,#32568,#32569,#32570,#32571,#32572,
#32573,#32574,#32575,#32576,#32577,#32578,#32579,#32580,#32581,#32582,#32583,
#32584,#32585,#32586,#32587,#32588,#32589,#32590,#32591,#32592,#32593,#32594,
#32595,#32596,#32597,#32598,#32599,#32600,#32601,#32602,#32603),
 .UNSPECIFIED.,.F.,.F.,(4,3,3,3,3,3,3,3,3,3,3,3,3,3,3,3,3,3,3,4),(2.61184801452757E-8,
0.0625,0.09375,0.125,0.15625,0.1875,0.25,0.3125,0.375,0.5,0.625,0.647792304041325,
0.6875,0.75,0.8125,0.84375,0.875,0.90625,0.9375,0.999999815671741),
 .UNSPECIFIED.);
#663=B_SPLINE_CURVE_WITH_KNOTS('',3,(#32608,#32609,#32610,#32611,#32612,
#32613,#32614,#32615,#32616,#32617,#32618,#32619,#32620,#32621,#32622,#32623,
#32624,#32625,#32626,#32627,#32628),.UNSPECIFIED.,.F.,.F.,(4,1,1,1,1,1,
1,1,1,1,1,1,1,1,1,1,1,1,4),(2.84967473049237E-7,0.0625,0.09375,0.125,0.15625,
0.1875,0.25,0.3125,0.375,0.5,0.625,0.6875,0.75,0.8125,0.84375,0.875,0.90625,
0.9375,0.999999714401756),.UNSPECIFIED.);
#664=B_SPLINE_CURVE_WITH_KNOTS('',3,(#32630,#32631,#32632,#32633,#32634,
#32635,#32636,#32637,#32638,#32639,#32640,#32641,#32642,#32643,#32644,#32645,
#32646,#32647,#32648,#32649,#32650),.UNSPECIFIED.,.F.,.F.,(4,1,1,1,1,1,
1,1,1,1,1,1,1,1,1,1,1,1,4),(0.,0.0625,0.09375,0.125,0.15625,0.1875,0.25,
0.3125,0.375,0.5,0.625,0.6875,0.75,0.8125,0.84375,0.875,0.90625,0.9375,
1.),.UNSPECIFIED.);
#665=B_SPLINE_CURVE_WITH_KNOTS('',3,(#32654,#32655,#32656,#32657,#32658,
#32659,#32660,#32661,#32662,#32663,#32664,#32665,#32666,#32667,#32668,#32669,
#32670,#32671,#32672,#32673,#32674),.UNSPECIFIED.,.F.,.F.,(4,1,1,1,1,1,
1,1,1,1,1,1,1,1,1,1,1,1,4),(2.94403525435868E-7,0.0625,0.09375,0.125,0.15625,
0.1875,0.25,0.3125,0.375,0.5,0.625,0.6875,0.75,0.8125,0.84375,0.875,0.90625,
0.9375,1.),.UNSPECIFIED.);
#666=B_SPLINE_CURVE_WITH_KNOTS('',3,(#32675,#32676,#32677,#32678,#32679,
#32680,#32681,#32682,#32683,#32684,#32685,#32686,#32687,#32688,#32689,#32690,
#32691,#32692,#32693,#32694,#32695,#32696,#32697,#32698,#32699,#32700,#32701,
#32702,#32703,#32704,#32705,#32706,#32707,#32708,#32709,#32710,#32711,#32712,
#32713,#32714,#32715,#32716,#32717,#32718,#32719,#32720,#32721,#32722,#32723,
#32724,#32725,#32726,#32727,#32728,#32729,#32730,#32731,#32732),
 .UNSPECIFIED.,.F.,.F.,(4,3,3,3,3,3,3,3,3,3,3,3,3,3,3,3,3,3,3,4),(3.81813237642607E-8,
0.0625,0.09375,0.125,0.15625,0.1875,0.25,0.3125,0.375,0.5,0.625,0.649759799039456,
0.6875,0.75,0.8125,0.84375,0.875,0.90625,0.9375,0.999999823797946),
 .UNSPECIFIED.);
#667=B_SPLINE_CURVE_WITH_KNOTS('',3,(#32737,#32738,#32739,#32740,#32741,
#32742,#32743,#32744,#32745,#32746,#32747,#32748,#32749,#32750,#32751,#32752,
#32753,#32754,#32755),.UNSPECIFIED.,.F.,.F.,(4,1,1,1,1,1,1,1,1,1,1,1,1,
1,1,1,4),(2.60222887639683E-7,0.0625,0.09375,0.125,0.15625,0.1875,0.25,
0.375,0.5,0.625,0.6875,0.71875,0.75,0.78125,0.8125,0.875,0.999999892515785),
 .UNSPECIFIED.);
#668=B_SPLINE_CURVE_WITH_KNOTS('',3,(#32757,#32758,#32759,#32760,#32761,
#32762,#32763,#32764,#32765,#32766,#32767,#32768,#32769,#32770,#32771,#32772,
#32773,#32774,#32775),.UNSPECIFIED.,.F.,.F.,(4,1,1,1,1,1,1,1,1,1,1,1,1,
1,1,1,4),(0.,0.125,0.1875,0.21875,0.25,0.28125,0.3125,0.375,0.5,0.625,0.75,
0.8125,0.84375,0.875,0.90625,0.9375,1.),.UNSPECIFIED.);
#669=B_SPLINE_CURVE_WITH_KNOTS('',3,(#32779,#32780,#32781,#32782,#32783,
#32784,#32785,#32786,#32787,#32788,#32789,#32790,#32791,#32792,#32793,#32794,
#32795,#32796,#32797,#32798,#32799,#32800,#32801,#32802,#32803,#32804,#32805,
#32806,#32807,#32808,#32809,#32810,#32811,#32812,#32813,#32814,#32815,#32816,
#32817,#32818,#32819,#32820,#32821,#32822,#32823,#32824,#32825,#32826,#32827,
#32828,#32829,#32830),.UNSPECIFIED.,.F.,.F.,(4,3,3,3,3,3,3,3,3,3,3,3,3,
3,3,3,3,4),(2.63017244894725E-7,0.0625,0.09375,0.125,0.15625,0.1875,0.25,
0.367332392673666,0.375,0.5,0.625,0.6875,0.71875,0.75,0.78125,0.8125,0.875,
0.99999998868207),.UNSPECIFIED.);
#670=B_SPLINE_CURVE_WITH_KNOTS('',3,(#32831,#32832,#32833,#32834,#32835,
#32836,#32837,#32838,#32839,#32840,#32841,#32842,#32843,#32844,#32845,#32846,
#32847,#32848,#32849,#32850,#32851,#32852,#32853,#32854,#32855,#32856,#32857,
#32858,#32859,#32860,#32861,#32862,#32863,#32864,#32865,#32866,#32867,#32868,
#32869,#32870,#32871,#32872,#32873,#32874,#32875,#32876,#32877,#32878,#32879,
#32880,#32881,#32882),.UNSPECIFIED.,.F.,.F.,(4,3,3,3,3,3,3,3,3,3,3,3,3,
3,3,3,3,4),(0.,0.125,0.1875,0.21875,0.25,0.28125,0.3125,0.375,0.5,0.625,
0.633637925900044,0.75,0.8125,0.84375,0.875,0.90625,0.9375,0.99999982150407),
 .UNSPECIFIED.);
#671=B_SPLINE_CURVE_WITH_KNOTS('',3,(#32887,#32888,#32889,#32890,#32891,
#32892,#32893,#32894,#32895,#32896,#32897,#32898,#32899,#32900,#32901,#32902,
#32903,#32904,#32905,#32906,#32907),.UNSPECIFIED.,.F.,.F.,(4,1,1,1,1,1,
1,1,1,1,1,1,1,1,1,1,1,1,4),(2.76569125747373E-7,0.0625,0.09375,0.125,0.15625,
0.1875,0.25,0.3125,0.375,0.5,0.625,0.6875,0.75,0.8125,0.84375,0.875,0.90625,
0.9375,0.999999617070618),.UNSPECIFIED.);
#672=B_SPLINE_CURVE_WITH_KNOTS('',3,(#32909,#32910,#32911,#32912,#32913,
#32914,#32915,#32916,#32917,#32918,#32919,#32920,#32921,#32922,#32923,#32924,
#32925,#32926,#32927,#32928,#32929),.UNSPECIFIED.,.F.,.F.,(4,1,1,1,1,1,
1,1,1,1,1,1,1,1,1,1,1,1,4),(0.,0.0625,0.09375,0.125,0.15625,0.1875,0.25,
0.3125,0.375,0.5,0.625,0.6875,0.75,0.8125,0.84375,0.875,0.90625,0.9375,
1.),.UNSPECIFIED.);
#673=B_SPLINE_CURVE_WITH_KNOTS('',3,(#32933,#32934,#32935,#32936,#32937,
#32938,#32939,#32940,#32941,#32942,#32943,#32944,#32945,#32946,#32947,#32948,
#32949,#32950,#32951,#32952,#32953,#32954,#32955,#32956,#32957,#32958,#32959,
#32960,#32961,#32962,#32963,#32964,#32965,#32966,#32967,#32968,#32969,#32970,
#32971,#32972,#32973,#32974,#32975,#32976,#32977,#32978,#32979,#32980,#32981,
#32982,#32983,#32984,#32985,#32986,#32987,#32988,#32989,#32990),
 .UNSPECIFIED.,.F.,.F.,(4,3,3,3,3,3,3,3,3,3,3,3,3,3,3,3,3,3,3,4),(2.8836184248057E-7,
0.0625,0.09375,0.125,0.15625,0.1875,0.25,0.3125,0.34633842624939,0.375,
0.5,0.625,0.6875,0.75,0.8125,0.84375,0.875,0.90625,0.9375,1.),
 .UNSPECIFIED.);
#674=B_SPLINE_CURVE_WITH_KNOTS('',3,(#32991,#32992,#32993,#32994,#32995,
#32996,#32997,#32998,#32999,#33000,#33001,#33002,#33003,#33004,#33005,#33006,
#33007,#33008,#33009,#33010,#33011,#33012,#33013,#33014,#33015,#33016,#33017,
#33018,#33019,#33020,#33021,#33022,#33023,#33024,#33025,#33026,#33027,#33028,
#33029,#33030,#33031,#33032,#33033,#33034,#33035,#33036,#33037,#33038,#33039,
#33040,#33041,#33042,#33043,#33044,#33045,#33046,#33047,#33048),
 .UNSPECIFIED.,.F.,.F.,(4,3,3,3,3,3,3,3,3,3,3,3,3,3,3,3,3,3,3,4),(8.75906255719806E-8,
0.0625,0.09375,0.125,0.15625,0.1875,0.25,0.3125,0.375,0.5,0.625,0.653697969502116,
0.6875,0.75,0.8125,0.84375,0.875,0.90625,0.9375,0.999999836937693),
 .UNSPECIFIED.);
#675=B_SPLINE_CURVE_WITH_KNOTS('',3,(#33053,#33054,#33055,#33056,#33057,
#33058,#33059,#33060,#33061,#33062,#33063,#33064),.UNSPECIFIED.,.F.,.F.,
(4,1,1,1,1,1,1,1,1,4),(0.,0.0625,0.09375,0.125,0.15625,0.1875,0.25,0.3125,
0.375,0.5),.UNSPECIFIED.);
#676=B_SPLINE_CURVE_WITH_KNOTS('',3,(#33066,#33067,#33068,#33069,#33070,
#33071,#33072,#33073,#33074,#33075,#33076),.UNSPECIFIED.,.F.,.F.,(4,1,1,
1,1,1,1,1,4),(0.5,0.625,0.75,0.8125,0.84375,0.875,0.90625,0.9375,1.),
 .UNSPECIFIED.);
#677=B_SPLINE_CURVE_WITH_KNOTS('',3,(#33078,#33079,#33080,#33081,#33082,
#33083,#33084,#33085,#33086,#33087,#33088),.UNSPECIFIED.,.F.,.F.,(4,1,1,
1,1,1,1,1,4),(7.15869646362667E-6,0.0625,0.09375,0.125,0.15625,0.1875,0.25,
0.375,0.499318743160308),.UNSPECIFIED.);
#678=B_SPLINE_CURVE_WITH_KNOTS('',3,(#33090,#33091,#33092,#33093,#33094,
#33095,#33096,#33097,#33098,#33099,#33100,#33101,#33102),.UNSPECIFIED.,
 .F.,.F.,(4,1,1,1,1,1,1,1,1,1,4),(0.499318743160308,0.5,0.625,0.6875,0.75,
0.8125,0.84375,0.875,0.90625,0.9375,1.),.UNSPECIFIED.);
#679=B_SPLINE_CURVE_WITH_KNOTS('',3,(#33106,#33107,#33108,#33109,#33110,
#33111,#33112,#33113,#33114,#33115,#33116,#33117),.UNSPECIFIED.,.F.,.F.,
(4,1,1,1,1,1,1,1,1,4),(0.,0.0625,0.09375,0.125,0.15625,0.1875,0.25,0.3125,
0.375,0.5),.UNSPECIFIED.);
#680=B_SPLINE_CURVE_WITH_KNOTS('',3,(#33119,#33120,#33121,#33122,#33123,
#33124,#33125,#33126,#33127,#33128,#33129),.UNSPECIFIED.,.F.,.F.,(4,1,1,
1,1,1,1,1,4),(0.5,0.625,0.75,0.8125,0.84375,0.875,0.90625,0.9375,1.),
 .UNSPECIFIED.);
#681=B_SPLINE_CURVE_WITH_KNOTS('',3,(#33131,#33132,#33133,#33134,#33135,
#33136,#33137,#33138,#33139,#33140,#33141),.UNSPECIFIED.,.F.,.F.,(4,1,1,
1,1,1,1,1,4),(2.21677758325209E-7,0.0625,0.09375,0.125,0.15625,0.1875,0.25,
0.375,0.499882005198117),.UNSPECIFIED.);
#682=B_SPLINE_CURVE_WITH_KNOTS('',3,(#33142,#33143,#33144,#33145,#33146,
#33147,#33148,#33149,#33150,#33151,#33152,#33153),.UNSPECIFIED.,.F.,.F.,
(4,1,1,1,1,1,1,1,1,4),(0.5,0.625,0.6875,0.75,0.8125,0.84375,0.875,0.90625,
0.9375,0.999977373123454),.UNSPECIFIED.);
#683=B_SPLINE_CURVE_WITH_KNOTS('',3,(#33158,#33159,#33160,#33161,#33162,
#33163,#33164,#33165,#33166,#33167,#33168,#33169,#33170,#33171,#33172,#33173,
#33174,#33175,#33176,#33177,#33178),.UNSPECIFIED.,.F.,.F.,(4,1,1,1,1,1,
1,1,1,1,1,1,1,1,1,1,1,1,4),(2.84936194355119E-7,0.0625,0.09375,0.125,0.15625,
0.1875,0.25,0.3125,0.375,0.5,0.625,0.6875,0.75,0.8125,0.84375,0.875,0.90625,
0.9375,0.999999655061917),.UNSPECIFIED.);
#684=B_SPLINE_CURVE_WITH_KNOTS('',3,(#33180,#33181,#33182,#33183,#33184,
#33185,#33186,#33187,#33188,#33189,#33190,#33191,#33192,#33193,#33194,#33195,
#33196,#33197,#33198,#33199,#33200),.UNSPECIFIED.,.F.,.F.,(4,1,1,1,1,1,
1,1,1,1,1,1,1,1,1,1,1,1,4),(0.,0.0625,0.09375,0.125,0.15625,0.1875,0.25,
0.3125,0.375,0.5,0.625,0.6875,0.75,0.8125,0.84375,0.875,0.90625,0.9375,
1.),.UNSPECIFIED.);
#685=B_SPLINE_CURVE_WITH_KNOTS('',3,(#33204,#33205,#33206,#33207,#33208,
#33209,#33210,#33211,#33212,#33213,#33214,#33215,#33216,#33217,#33218,#33219,
#33220,#33221,#33222,#33223,#33224,#33225,#33226,#33227,#33228,#33229,#33230,
#33231,#33232,#33233,#33234,#33235,#33236,#33237,#33238,#33239,#33240,#33241,
#33242,#33243,#33244,#33245,#33246,#33247,#33248,#33249,#33250,#33251,#33252,
#33253,#33254,#33255,#33256,#33257,#33258,#33259,#33260,#33261),
 .UNSPECIFIED.,.F.,.F.,(4,3,3,3,3,3,3,3,3,3,3,3,3,3,3,3,3,3,3,4),(3.05273049617562E-7,
0.0625,0.09375,0.125,0.15625,0.1875,0.25,0.3125,0.348322390156725,0.375,
0.5,0.625,0.6875,0.75,0.8125,0.84375,0.875,0.90625,0.9375,1.),
 .UNSPECIFIED.);
#686=B_SPLINE_CURVE_WITH_KNOTS('',3,(#33262,#33263,#33264,#33265,#33266,
#33267,#33268,#33269,#33270,#33271,#33272,#33273,#33274,#33275,#33276,#33277,
#33278,#33279,#33280,#33281,#33282,#33283,#33284,#33285,#33286,#33287,#33288,
#33289,#33290,#33291,#33292,#33293,#33294,#33295,#33296,#33297,#33298,#33299,
#33300,#33301,#33302,#33303,#33304,#33305,#33306,#33307,#33308,#33309,#33310,
#33311,#33312,#33313,#33314,#33315,#33316,#33317,#33318,#33319),
 .UNSPECIFIED.,.F.,.F.,(4,3,3,3,3,3,3,3,3,3,3,3,3,3,3,3,3,3,3,4),(6.62097895526065E-8,
0.0625,0.09375,0.125,0.15625,0.1875,0.25,0.3125,0.375,0.5,0.625,0.651832350452469,
0.6875,0.75,0.8125,0.84375,0.875,0.90625,0.9375,0.9999998312716),
 .UNSPECIFIED.);
#687=B_SPLINE_CURVE_WITH_KNOTS('',3,(#33324,#33325,#33326,#33327,#33328,
#33329,#33330,#33331,#33332,#33333,#33334,#33335,#33336,#33337,#33338,#33339,
#33340,#33341,#33342),.UNSPECIFIED.,.F.,.F.,(4,1,1,1,1,1,1,1,1,1,1,1,1,
1,1,1,4),(2.75587839344889E-7,0.0625,0.09375,0.125,0.15625,0.1875,0.25,
0.375,0.5,0.625,0.6875,0.71875,0.75,0.78125,0.8125,0.875,0.999999959370797),
 .UNSPECIFIED.);
#688=B_SPLINE_CURVE_WITH_KNOTS('',3,(#33344,#33345,#33346,#33347,#33348,
#33349,#33350,#33351,#33352,#33353,#33354,#33355,#33356,#33357,#33358,#33359,
#33360,#33361,#33362),.UNSPECIFIED.,.F.,.F.,(4,1,1,1,1,1,1,1,1,1,1,1,1,
1,1,1,4),(0.,0.125,0.1875,0.21875,0.25,0.28125,0.3125,0.375,0.5,0.625,0.75,
0.8125,0.84375,0.875,0.90625,0.9375,1.),.UNSPECIFIED.);
#689=B_SPLINE_CURVE_WITH_KNOTS('',3,(#33366,#33367,#33368,#33369,#33370,
#33371,#33372,#33373,#33374,#33375,#33376,#33377,#33378,#33379,#33380,#33381,
#33382,#33383,#33384,#33385,#33386,#33387,#33388,#33389,#33390,#33391,#33392,
#33393,#33394,#33395,#33396,#33397,#33398,#33399,#33400,#33401,#33402,#33403,
#33404,#33405,#33406,#33407,#33408,#33409,#33410,#33411,#33412,#33413,#33414,
#33415,#33416,#33417),.UNSPECIFIED.,.F.,.F.,(4,3,3,3,3,3,3,3,3,3,3,3,3,
3,3,3,3,4),(2.808774569524E-7,0.0625,0.09375,0.125,0.15625,0.1875,0.25,
0.35969017869594,0.375,0.5,0.625,0.6875,0.71875,0.75,0.78125,0.8125,0.875,
1.),.UNSPECIFIED.);
#690=B_SPLINE_CURVE_WITH_KNOTS('',3,(#33418,#33419,#33420,#33421,#33422,
#33423,#33424,#33425,#33426,#33427,#33428,#33429,#33430,#33431,#33432,#33433,
#33434,#33435,#33436,#33437,#33438,#33439,#33440,#33441,#33442,#33443,#33444,
#33445,#33446,#33447,#33448,#33449,#33450,#33451,#33452,#33453,#33454,#33455,
#33456,#33457,#33458,#33459,#33460,#33461,#33462,#33463,#33464,#33465,#33466,
#33467,#33468,#33469),.UNSPECIFIED.,.F.,.F.,(4,3,3,3,3,3,3,3,3,3,3,3,3,
3,3,3,3,4),(3.41422460553818E-8,0.125,0.1875,0.21875,0.25,0.28125,0.3125,
0.375,0.5,0.625,0.641077554901531,0.75,0.8125,0.84375,0.875,0.90625,0.9375,
0.999999822593873),.UNSPECIFIED.);
#691=B_SPLINE_CURVE_WITH_KNOTS('',3,(#33474,#33475,#33476,#33477,#33478,
#33479,#33480,#33481,#33482,#33483,#33484,#33485,#33486,#33487,#33488,#33489,
#33490,#33491,#33492),.UNSPECIFIED.,.F.,.F.,(4,1,1,1,1,1,1,1,1,1,1,1,1,
1,1,1,4),(2.80445484236532E-7,0.0625,0.09375,0.125,0.15625,0.1875,0.25,
0.375,0.5,0.625,0.6875,0.71875,0.75,0.78125,0.8125,0.875,0.999999987809309),
 .UNSPECIFIED.);
#692=B_SPLINE_CURVE_WITH_KNOTS('',3,(#33494,#33495,#33496,#33497,#33498,
#33499,#33500,#33501,#33502,#33503,#33504,#33505,#33506,#33507,#33508,#33509,
#33510,#33511,#33512),.UNSPECIFIED.,.F.,.F.,(4,1,1,1,1,1,1,1,1,1,1,1,1,
1,1,1,4),(0.,0.125,0.1875,0.21875,0.25,0.28125,0.3125,0.375,0.5,0.625,0.75,
0.8125,0.84375,0.875,0.90625,0.9375,1.),.UNSPECIFIED.);
#693=B_SPLINE_CURVE_WITH_KNOTS('',3,(#33516,#33517,#33518,#33519,#33520,
#33521,#33522,#33523,#33524,#33525,#33526,#33527,#33528,#33529,#33530,#33531,
#33532,#33533,#33534,#33535,#33536,#33537,#33538,#33539,#33540,#33541,#33542,
#33543,#33544,#33545,#33546,#33547,#33548,#33549,#33550,#33551,#33552,#33553,
#33554,#33555,#33556,#33557,#33558,#33559,#33560,#33561,#33562,#33563,#33564,
#33565,#33566,#33567),.UNSPECIFIED.,.F.,.F.,(4,3,3,3,3,3,3,3,3,3,3,3,3,
3,3,3,3,4),(2.77199665841602E-7,0.0625,0.09375,0.125,0.15625,0.1875,0.25,
0.361636464506202,0.375,0.5,0.625,0.6875,0.71875,0.75,0.78125,0.8125,0.875,
1.),.UNSPECIFIED.);
#694=B_SPLINE_CURVE_WITH_KNOTS('',3,(#33568,#33569,#33570,#33571,#33572,
#33573,#33574,#33575,#33576,#33577,#33578,#33579,#33580,#33581,#33582,#33583,
#33584,#33585,#33586,#33587,#33588,#33589,#33590,#33591,#33592,#33593,#33594,
#33595,#33596,#33597,#33598,#33599,#33600,#33601,#33602,#33603,#33604,#33605,
#33606,#33607,#33608,#33609,#33610,#33611,#33612,#33613,#33614,#33615,#33616,
#33617,#33618,#33619),.UNSPECIFIED.,.F.,.F.,(4,3,3,3,3,3,3,3,3,3,3,3,3,
3,3,3,3,4),(6.91571290081694E-8,0.125,0.1875,0.21875,0.25,0.28125,0.3125,
0.375,0.5,0.625,0.639335759650785,0.75,0.8125,0.84375,0.875,0.90625,0.9375,
0.999999825283333),.UNSPECIFIED.);
#695=B_SPLINE_CURVE_WITH_KNOTS('',3,(#33624,#33625,#33626,#33627,#33628,
#33629,#33630,#33631,#33632,#33633,#33634,#33635,#33636,#33637,#33638,#33639,
#33640,#33641,#33642),.UNSPECIFIED.,.F.,.F.,(4,1,1,1,1,1,1,1,1,1,1,1,1,
1,1,1,4),(2.6847278418118E-7,0.0625,0.09375,0.125,0.15625,0.1875,0.25,0.375,
0.5,0.625,0.6875,0.71875,0.75,0.78125,0.8125,0.875,1.),.UNSPECIFIED.);
#696=B_SPLINE_CURVE_WITH_KNOTS('',3,(#33644,#33645,#33646,#33647,#33648,
#33649,#33650,#33651,#33652,#33653,#33654,#33655,#33656,#33657,#33658,#33659,
#33660,#33661,#33662),.UNSPECIFIED.,.F.,.F.,(4,1,1,1,1,1,1,1,1,1,1,1,1,
1,1,1,4),(1.72418419787525E-8,0.125,0.1875,0.21875,0.25,0.28125,0.3125,
0.375,0.5,0.625,0.75,0.8125,0.84375,0.875,0.90625,0.9375,1.),
 .UNSPECIFIED.);
#697=B_SPLINE_CURVE_WITH_KNOTS('',3,(#33666,#33667,#33668,#33669,#33670,
#33671,#33672,#33673,#33674,#33675,#33676,#33677,#33678,#33679,#33680,#33681,
#33682,#33683,#33684,#33685,#33686,#33687,#33688,#33689,#33690,#33691,#33692,
#33693,#33694,#33695,#33696,#33697,#33698,#33699,#33700,#33701,#33702,#33703,
#33704,#33705,#33706,#33707,#33708,#33709,#33710,#33711,#33712,#33713,#33714,
#33715,#33716,#33717),.UNSPECIFIED.,.F.,.F.,(4,3,3,3,3,3,3,3,3,3,3,3,3,
3,3,3,3,4),(2.74314204166858E-7,0.0625,0.09375,0.125,0.15625,0.1875,0.25,
0.36358849545573,0.375,0.5,0.625,0.6875,0.71875,0.75,0.78125,0.8125,0.875,
1.),.UNSPECIFIED.);
#698=B_SPLINE_CURVE_WITH_KNOTS('',3,(#33718,#33719,#33720,#33721,#33722,
#33723,#33724,#33725,#33726,#33727,#33728,#33729,#33730,#33731,#33732,#33733,
#33734,#33735,#33736,#33737,#33738,#33739,#33740,#33741,#33742,#33743,#33744,
#33745,#33746,#33747,#33748,#33749,#33750,#33751,#33752,#33753,#33754,#33755,
#33756,#33757,#33758,#33759,#33760,#33761,#33762,#33763,#33764,#33765,#33766,
#33767,#33768,#33769),.UNSPECIFIED.,.F.,.F.,(4,3,3,3,3,3,3,3,3,3,3,3,3,
3,3,3,3,4),(7.63260218006573E-8,0.125,0.1875,0.21875,0.25,0.28125,0.3125,
0.375,0.5,0.625,0.637553797507691,0.75,0.8125,0.84375,0.875,0.90625,0.9375,
0.999999824822769),.UNSPECIFIED.);
#699=B_SPLINE_CURVE_WITH_KNOTS('',3,(#33774,#33775,#33776,#33777,#33778,
#33779,#33780,#33781,#33782,#33783,#33784,#33785,#33786,#33787,#33788,#33789,
#33790,#33791,#33792),.UNSPECIFIED.,.F.,.F.,(4,1,1,1,1,1,1,1,1,1,1,1,1,
1,1,1,4),(0.,0.0625,0.09375,0.125,0.15625,0.1875,0.25,0.375,0.5,0.625,0.6875,
0.71875,0.75,0.78125,0.8125,0.875,1.),.UNSPECIFIED.);
#700=B_SPLINE_CURVE_WITH_KNOTS('',3,(#33794,#33795,#33796,#33797,#33798,
#33799,#33800,#33801,#33802,#33803,#33804,#33805,#33806,#33807,#33808,#33809,
#33810,#33811,#33812),.UNSPECIFIED.,.F.,.F.,(4,1,1,1,1,1,1,1,1,1,1,1,1,
1,1,1,4),(2.65886426353366E-9,0.125,0.1875,0.21875,0.25,0.28125,0.3125,
0.375,0.5,0.625,0.75,0.8125,0.84375,0.875,0.90625,0.9375,1.),
 .UNSPECIFIED.);
#701=B_SPLINE_CURVE_WITH_KNOTS('',3,(#33816,#33817,#33818,#33819,#33820,
#33821,#33822,#33823,#33824,#33825,#33826,#33827,#33828,#33829,#33830,#33831,
#33832,#33833,#33834,#33835,#33836,#33837,#33838,#33839,#33840,#33841,#33842,
#33843,#33844,#33845,#33846,#33847,#33848,#33849,#33850,#33851,#33852,#33853,
#33854,#33855,#33856,#33857,#33858,#33859,#33860,#33861,#33862,#33863,#33864,
#33865,#33866,#33867),.UNSPECIFIED.,.F.,.F.,(4,3,3,3,3,3,3,3,3,3,3,3,3,
3,3,3,3,4),(2.63361468193179E-7,0.0625,0.09375,0.125,0.15625,0.1875,0.25,
0.365500799027569,0.375,0.5,0.625,0.6875,0.71875,0.75,0.78125,0.8125,0.875,
0.99999997625737),.UNSPECIFIED.);
#702=B_SPLINE_CURVE_WITH_KNOTS('',3,(#33868,#33869,#33870,#33871,#33872,
#33873,#33874,#33875,#33876,#33877,#33878,#33879,#33880,#33881,#33882,#33883,
#33884,#33885,#33886,#33887,#33888,#33889,#33890,#33891,#33892,#33893,#33894,
#33895,#33896,#33897,#33898,#33899,#33900,#33901,#33902,#33903,#33904,#33905,
#33906,#33907,#33908,#33909,#33910,#33911,#33912,#33913,#33914,#33915,#33916,
#33917,#33918,#33919),.UNSPECIFIED.,.F.,.F.,(4,3,3,3,3,3,3,3,3,3,3,3,3,
3,3,3,3,4),(0.,0.125,0.1875,0.21875,0.25,0.28125,0.3125,0.375,0.5,0.625,
0.635593203482249,0.75,0.8125,0.84375,0.875,0.90625,0.9375,0.999999822175548),
 .UNSPECIFIED.);
#703=B_SPLINE_CURVE_WITH_KNOTS('',3,(#33924,#33925,#33926,#33927,#33928,
#33929,#33930,#33931,#33932,#33933,#33934,#33935),.UNSPECIFIED.,.F.,.F.,
(4,1,1,1,1,1,1,1,1,4),(0.,0.0625,0.09375,0.125,0.15625,0.1875,0.25,0.3125,
0.375,0.5),.UNSPECIFIED.);
#704=B_SPLINE_CURVE_WITH_KNOTS('',3,(#33937,#33938,#33939,#33940,#33941,
#33942,#33943,#33944,#33945,#33946,#33947),.UNSPECIFIED.,.F.,.F.,(4,1,1,
1,1,1,1,1,4),(0.5,0.625,0.75,0.8125,0.84375,0.875,0.90625,0.9375,1.),
 .UNSPECIFIED.);
#705=B_SPLINE_CURVE_WITH_KNOTS('',3,(#33949,#33950,#33951,#33952,#33953,
#33954,#33955,#33956,#33957,#33958,#33959),.UNSPECIFIED.,.F.,.F.,(4,1,1,
1,1,1,1,1,4),(6.38525460793569E-6,0.0625,0.09375,0.125,0.15625,0.1875,0.25,
0.375,0.499319982454846),.UNSPECIFIED.);
#706=B_SPLINE_CURVE_WITH_KNOTS('',3,(#33961,#33962,#33963,#33964,#33965,
#33966,#33967,#33968,#33969,#33970,#33971,#33972,#33973),.UNSPECIFIED.,
 .F.,.F.,(4,1,1,1,1,1,1,1,1,1,4),(0.499319982454846,0.5,0.625,0.6875,0.75,
0.8125,0.84375,0.875,0.90625,0.9375,1.),.UNSPECIFIED.);
#707=B_SPLINE_CURVE_WITH_KNOTS('',3,(#33977,#33978,#33979,#33980,#33981,
#33982,#33983,#33984,#33985,#33986,#33987,#33988),.UNSPECIFIED.,.F.,.F.,
(4,1,1,1,1,1,1,1,1,4),(0.,0.0625,0.09375,0.125,0.15625,0.1875,0.25,0.3125,
0.375,0.5),.UNSPECIFIED.);
#708=B_SPLINE_CURVE_WITH_KNOTS('',3,(#33990,#33991,#33992,#33993,#33994,
#33995,#33996,#33997,#33998,#33999,#34000),.UNSPECIFIED.,.F.,.F.,(4,1,1,
1,1,1,1,1,4),(0.5,0.625,0.75,0.8125,0.84375,0.875,0.90625,0.9375,1.),
 .UNSPECIFIED.);
#709=B_SPLINE_CURVE_WITH_KNOTS('',3,(#34002,#34003,#34004,#34005,#34006,
#34007,#34008,#34009,#34010,#34011,#34012),.UNSPECIFIED.,.F.,.F.,(4,1,1,
1,1,1,1,1,4),(2.4708654656939E-7,0.0625,0.09375,0.125,0.15625,0.1875,0.25,
0.375,0.499884707955717),.UNSPECIFIED.);
#710=B_SPLINE_CURVE_WITH_KNOTS('',3,(#34013,#34014,#34015,#34016,#34017,
#34018,#34019,#34020,#34021,#34022,#34023,#34024),.UNSPECIFIED.,.F.,.F.,
(4,1,1,1,1,1,1,1,1,4),(0.5,0.625,0.6875,0.75,0.8125,0.84375,0.875,0.90625,
0.9375,0.999978109235681),.UNSPECIFIED.);
#711=B_SPLINE_CURVE_WITH_KNOTS('',3,(#34027,#34028,#34029,#34030,#34031,
#34032,#34033,#34034,#34035,#34036,#34037,#34038,#34039,#34040,#34041,#34042,
#34043,#34044,#34045,#34046,#34047,#34048,#34049,#34050,#34051,#34052,#34053,
#34054,#34055,#34056,#34057),.UNSPECIFIED.,.F.,.F.,(4,3,3,3,3,3,3,3,3,3,
4),(0.000176563406958893,0.125,0.1875,0.25,0.3125,0.375,0.5,0.625,0.75,
0.875,0.999998995305369),.UNSPECIFIED.);
#712=B_SPLINE_CURVE_WITH_KNOTS('',3,(#34059,#34060,#34061,#34062,#34063,
#34064,#34065,#34066,#34067,#34068,#34069,#34070,#34071),.UNSPECIFIED.,
 .F.,.F.,(4,1,1,1,1,1,1,1,1,1,4),(1.66911490650295E-8,0.0625,0.09375,0.125,
0.15625,0.1875,0.25,0.3125,0.375,0.5,0.500683333035046),.UNSPECIFIED.);
#713=B_SPLINE_CURVE_WITH_KNOTS('',3,(#34073,#34074,#34075,#34076,#34077,
#34078,#34079,#34080,#34081,#34082,#34083),.UNSPECIFIED.,.F.,.F.,(4,1,1,
1,1,1,1,1,4),(0.500683333035046,0.625,0.75,0.8125,0.84375,0.875,0.90625,
0.9375,0.999999813866294),.UNSPECIFIED.);
#714=B_SPLINE_CURVE_WITH_KNOTS('',3,(#34085,#34086,#34087,#34088,#34089,
#34090,#34091,#34092,#34093,#34094,#34095),.UNSPECIFIED.,.F.,.F.,(4,1,1,
1,1,1,1,1,4),(0.,0.0625,0.09375,0.125,0.15625,0.1875,0.25,0.375,0.499405889061093),
 .UNSPECIFIED.);
#715=B_SPLINE_CURVE_WITH_KNOTS('',3,(#34097,#34098,#34099,#34100,#34101,
#34102,#34103,#34104,#34105,#34106,#34107,#34108),.UNSPECIFIED.,.F.,.F.,
(4,1,1,1,1,1,1,1,1,4),(0.499405889061093,0.5,0.625,0.75,0.8125,0.84375,
0.875,0.90625,0.9375,1.),.UNSPECIFIED.);
#716=B_SPLINE_CURVE_WITH_KNOTS('',3,(#34110,#34111,#34112,#34113,#34114,
#34115,#34116,#34117,#34118,#34119,#34120,#34121,#34122,#34123,#34124,#34125,
#34126,#34127,#34128,#34129,#34130,#34131,#34132,#34133,#34134,#34135,#34136,
#34137,#34138,#34139,#34140),.UNSPECIFIED.,.F.,.F.,(4,3,3,3,3,3,3,3,3,3,
4),(3.42300885912184E-6,0.125,0.25,0.375,0.5,0.625,0.75,0.8125,0.875,0.9375,
0.999842771045948),.UNSPECIFIED.);
#717=B_SPLINE_CURVE_WITH_KNOTS('',3,(#34142,#34143,#34144,#34145,#34146,
#34147,#34148,#34149,#34150,#34151,#34152,#34153),.UNSPECIFIED.,.F.,.F.,
(4,1,1,1,1,1,1,1,1,4),(0.,0.0625,0.09375,0.125,0.15625,0.1875,0.25,0.3125,
0.375,0.461683849721955),.UNSPECIFIED.);
#718=B_SPLINE_CURVE_WITH_KNOTS('',3,(#34155,#34156,#34157,#34158,#34159,
#34160,#34161,#34162,#34163,#34164,#34165,#34166),.UNSPECIFIED.,.F.,.F.,
(4,1,1,1,1,1,1,1,1,4),(0.461683849721955,0.5,0.625,0.75,0.8125,0.84375,
0.875,0.90625,0.9375,1.),.UNSPECIFIED.);
#719=B_SPLINE_CURVE_WITH_KNOTS('',3,(#34168,#34169,#34170,#34171,#34172,
#34173,#34174,#34175,#34176,#34177,#34178),.UNSPECIFIED.,.F.,.F.,(4,1,1,
1,1,1,1,1,4),(2.44966122427333E-7,0.0625,0.09375,0.125,0.15625,0.1875,0.25,
0.375,0.499887143451556),.UNSPECIFIED.);
#720=B_SPLINE_CURVE_WITH_KNOTS('',3,(#34179,#34180,#34181,#34182,#34183,
#34184,#34185,#34186,#34187,#34188,#34189,#34190),.UNSPECIFIED.,.F.,.F.,
(4,1,1,1,1,1,1,1,1,4),(0.5,0.625,0.6875,0.75,0.8125,0.84375,0.875,0.90625,
0.9375,0.999988315055417),.UNSPECIFIED.);
#721=B_SPLINE_CURVE_WITH_KNOTS('',3,(#34193,#34194,#34195,#34196,#34197,
#34198,#34199,#34200,#34201),.UNSPECIFIED.,.F.,.F.,(4,1,1,1,1,1,4),(0.00162491627968111,
0.125,0.1875,0.25,0.3125,0.375,0.499422005584456),.UNSPECIFIED.);
#722=B_SPLINE_CURVE_WITH_KNOTS('',3,(#34203,#34204,#34205,#34206,#34207,
#34208,#34209,#34210),.UNSPECIFIED.,.F.,.F.,(4,1,1,1,1,4),(0.5,0.625,0.75,
0.875,0.9375,1.),.UNSPECIFIED.);
#723=B_SPLINE_CURVE_WITH_KNOTS('',3,(#34212,#34213,#34214,#34215,#34216,
#34217,#34218,#34219,#34220,#34221,#34222,#34223,#34224,#34225,#34226,#34227,
#34228,#34229,#34230,#34231,#34232,#34233,#34234,#34235,#34236,#34237,#34238,
#34239,#34240,#34241,#34242),.UNSPECIFIED.,.F.,.F.,(4,3,3,3,3,3,3,3,3,3,
4),(2.03685100085616E-6,0.0625,0.09375,0.125,0.15625,0.1875,0.25,0.373077890397942,
0.375,0.5,0.500627296921563),.UNSPECIFIED.);
#724=B_SPLINE_CURVE_WITH_KNOTS('',3,(#34244,#34245,#34246,#34247,#34248,
#34249,#34250,#34251,#34252,#34253,#34254,#34255,#34256,#34257,#34258,#34259,
#34260,#34261,#34262,#34263,#34264,#34265,#34266,#34267,#34268),
 .UNSPECIFIED.,.F.,.F.,(4,3,3,3,3,3,3,3,4),(0.500627296921563,0.625,0.6875,
0.71875,0.75,0.78125,0.8125,0.875,0.999999762981869),.UNSPECIFIED.);
#725=B_SPLINE_CURVE_WITH_KNOTS('',3,(#34270,#34271,#34272,#34273,#34274,
#34275,#34276,#34277,#34278,#34279,#34280,#34281,#34282,#34283,#34284,#34285,
#34286,#34287,#34288,#34289,#34290,#34291,#34292,#34293,#34294,#34295,#34296,
#34297),.UNSPECIFIED.,.F.,.F.,(4,3,3,3,3,3,3,3,3,4),(0.,0.125,0.1875,0.21875,
0.25,0.28125,0.3125,0.375,0.5,0.500193349382862),.UNSPECIFIED.);
#726=B_SPLINE_CURVE_WITH_KNOTS('',3,(#34299,#34300,#34301,#34302,#34303,
#34304,#34305,#34306,#34307,#34308,#34309,#34310,#34311,#34312,#34313,#34314,
#34315,#34316,#34317,#34318,#34319,#34320,#34321,#34322,#34323),
 .UNSPECIFIED.,.F.,.F.,(4,3,3,3,3,3,3,3,4),(0.500193349382862,0.625,0.75,
0.8125,0.84375,0.875,0.90625,0.9375,1.),.UNSPECIFIED.);
#727=B_SPLINE_CURVE_WITH_KNOTS('',3,(#34325,#34326,#34327,#34328,#34329,
#34330,#34331,#34332,#34333,#34334,#34335,#34336,#34337,#34338,#34339,#34340,
#34341,#34342,#34343,#34344,#34345,#34346,#34347,#34348,#34349,#34350,#34351,
#34352),.UNSPECIFIED.,.F.,.F.,(4,3,3,3,3,3,3,3,3,4),(3.81246354337078E-6,
0.125,0.25,0.375,0.5,0.625,0.75,0.875,0.9375,0.999998611687521),
 .UNSPECIFIED.);
#728=B_SPLINE_CURVE_WITH_KNOTS('',3,(#34354,#34355,#34356,#34357,#34358,
#34359,#34360,#34361,#34362,#34363,#34364,#34365,#34366,#34367,#34368,#34369,
#34370,#34371,#34372),.UNSPECIFIED.,.F.,.F.,(4,1,1,1,1,1,1,1,1,1,1,1,1,
1,1,1,4),(0.,0.0625,0.09375,0.125,0.15625,0.1875,0.25,0.375,0.5,0.625,0.75,
0.8125,0.84375,0.875,0.90625,0.9375,1.),.UNSPECIFIED.);
#729=B_SPLINE_CURVE_WITH_KNOTS('',3,(#34374,#34375,#34376,#34377),
 .UNSPECIFIED.,.F.,.F.,(4,4),(0.951680478228109,0.999996857021366),
 .UNSPECIFIED.);
#730=B_SPLINE_CURVE_WITH_KNOTS('',3,(#34379,#34380,#34381,#34382,#34383,
#34384,#34385,#34386,#34387,#34388,#34389,#34390,#34391,#34392,#34393,#34394,
#34395,#34396,#34397,#34398,#34399,#34400,#34401,#34402,#34403,#34404,#34405,
#34406),.UNSPECIFIED.,.F.,.F.,(4,3,3,3,3,3,3,3,3,4),(0.583516228419036,
0.59375,0.625,0.6875,0.71875,0.75,0.78125,0.8125,0.875,0.951680478228109),
 .UNSPECIFIED.);
#731=B_SPLINE_CURVE_WITH_KNOTS('',3,(#34408,#34409,#34410,#34411,#34412,
#34413,#34414,#34415,#34416,#34417,#34418,#34419,#34420,#34421,#34422,#34423,
#34424,#34425,#34426,#34427,#34428,#34429,#34430,#34431,#34432,#34433,#34434,
#34435,#34436,#34437,#34438,#34439,#34440,#34441,#34442,#34443,#34444,#34445,
#34446,#34447,#34448,#34449,#34450,#34451,#34452,#34453,#34454,#34455,#34456,
#34457,#34458,#34459,#34460,#34461,#34462,#34463,#34464,#34465),
 .UNSPECIFIED.,.F.,.F.,(4,3,3,3,3,3,3,3,3,3,3,3,3,3,3,3,3,3,3,4),(0.1328125,
0.140625,0.15625,0.171875,0.1875,0.203125,0.21875,0.25,0.28125,0.3125,0.375,
0.435752721141823,0.4375,0.46875,0.484375,0.5,0.515625,0.53125,0.5625,0.583516228419036),
 .UNSPECIFIED.);
#732=B_SPLINE_CURVE_WITH_KNOTS('',3,(#34466,#34467,#34468,#34469,#34470,
#34471,#34472,#34473,#34474,#34475,#34476,#34477,#34478,#34479,#34480,#34481),
 .UNSPECIFIED.,.F.,.F.,(4,3,3,3,3,4),(0.00169583748688586,0.0625,0.09375,
0.109375,0.125,0.1328125),.UNSPECIFIED.);
#733=B_SPLINE_CURVE_WITH_KNOTS('',3,(#34486,#34487,#34488,#34489,#34490,
#34491,#34492,#34493,#34494,#34495,#34496,#34497,#34498,#34499,#34500,#34501,
#34502,#34503,#34504),.UNSPECIFIED.,.F.,.F.,(4,1,1,1,1,1,1,1,1,1,1,1,1,
1,1,1,4),(0.,0.0625,0.09375,0.125,0.15625,0.1875,0.25,0.375,0.5,0.625,0.6875,
0.71875,0.75,0.78125,0.8125,0.875,0.999999781104463),.UNSPECIFIED.);
#734=B_SPLINE_CURVE_WITH_KNOTS('',3,(#34506,#34507,#34508,#34509,#34510,
#34511,#34512,#34513,#34514,#34515,#34516,#34517,#34518,#34519,#34520,#34521,
#34522,#34523,#34524),.UNSPECIFIED.,.F.,.F.,(4,1,1,1,1,1,1,1,1,1,1,1,1,
1,1,1,4),(0.,0.125,0.1875,0.21875,0.25,0.28125,0.3125,0.375,0.5,0.625,0.75,
0.8125,0.84375,0.875,0.90625,0.9375,1.),.UNSPECIFIED.);
#735=B_SPLINE_CURVE_WITH_KNOTS('',3,(#34528,#34529,#34530,#34531,#34532,
#34533,#34534,#34535,#34536,#34537,#34538,#34539,#34540,#34541,#34542,#34543,
#34544,#34545,#34546,#34547,#34548,#34549,#34550,#34551,#34552,#34553,#34554,
#34555),.UNSPECIFIED.,.F.,.F.,(4,3,3,3,3,3,3,3,3,4),(0.,0.0625,0.09375,
0.125,0.15625,0.1875,0.25,0.364624833230614,0.375,0.499908883353168),
 .UNSPECIFIED.);
#736=B_SPLINE_CURVE_WITH_KNOTS('',3,(#34557,#34558,#34559,#34560,#34561,
#34562,#34563,#34564,#34565,#34566,#34567,#34568,#34569,#34570,#34571,#34572,
#34573,#34574,#34575,#34576,#34577,#34578,#34579,#34580,#34581),
 .UNSPECIFIED.,.F.,.F.,(4,3,3,3,3,3,3,3,4),(0.5,0.625,0.6875,0.71875,0.75,
0.78125,0.8125,0.875,0.999999882722085),.UNSPECIFIED.);
#737=B_SPLINE_CURVE_WITH_KNOTS('',3,(#34583,#34584,#34585,#34586,#34587,
#34588,#34589,#34590,#34591,#34592,#34593,#34594,#34595,#34596,#34597,#34598,
#34599,#34600,#34601,#34602,#34603,#34604,#34605,#34606,#34607),
 .UNSPECIFIED.,.F.,.F.,(4,3,3,3,3,3,3,3,4),(0.,0.125,0.1875,0.21875,0.25,
0.28125,0.3125,0.375,0.5),.UNSPECIFIED.);
#738=B_SPLINE_CURVE_WITH_KNOTS('',3,(#34608,#34609,#34610,#34611,#34612,
#34613,#34614,#34615,#34616,#34617,#34618,#34619,#34620,#34621,#34622,#34623,
#34624,#34625,#34626,#34627,#34628,#34629,#34630,#34631,#34632,#34633,#34634,
#34635),.UNSPECIFIED.,.F.,.F.,(4,3,3,3,3,3,3,3,3,4),(0.5,0.625,0.636092397936151,
0.75,0.8125,0.84375,0.875,0.90625,0.9375,1.),.UNSPECIFIED.);
#739=B_SPLINE_CURVE_WITH_KNOTS('',3,(#34638,#34639,#34640,#34641,#34642,
#34643,#34644,#34645,#34646,#34647,#34648,#34649,#34650,#34651,#34652,#34653,
#34654,#34655,#34656,#34657,#34658,#34659,#34660,#34661,#34662,#34663,#34664,
#34665,#34666,#34667,#34668,#34669,#34670,#34671,#34672,#34673,#34674,#34675,
#34676,#34677,#34678,#34679,#34680,#34681,#34682,#34683,#34684,#34685,#34686,
#34687,#34688,#34689,#34690,#34691,#34692,#34693,#34694,#34695,#34696,#34697,
#34698,#34699,#34700,#34701,#34702,#34703,#34704,#34705,#34706,#34707,#34708,
#34709,#34710,#34711,#34712,#34713,#34714,#34715,#34716,#34717,#34718,#34719,
#34720,#34721,#34722,#34723,#34724,#34725,#34726,#34727,#34728,#34729,#34730,
#34731),.UNSPECIFIED.,.F.,.F.,(4,3,3,3,3,3,3,3,3,3,3,3,3,3,3,3,3,3,3,3,
3,3,3,3,3,3,3,3,3,3,3,4),(3.86564741912649E-6,0.0625,0.125,0.1875,0.211937941253132,
0.21875,0.234375,0.25,0.2578125,0.26171875,0.265625,0.28125,0.3125,0.34375,
0.359375,0.375,0.390625,0.40625,0.4375,0.46875,0.5,0.515625,0.53125,0.5625,
0.625,0.6875,0.71875,0.75,0.78125,0.8125,0.875,1.),.UNSPECIFIED.);
#740=B_SPLINE_CURVE_WITH_KNOTS('',3,(#34733,#34734,#34735,#34736,#34737,
#34738,#34739,#34740),.UNSPECIFIED.,.F.,.F.,(4,1,1,1,1,4),(3.28844511523668E-5,
0.0625,0.125,0.25,0.375,0.5),.UNSPECIFIED.);
#741=B_SPLINE_CURVE_WITH_KNOTS('',3,(#34742,#34743,#34744,#34745,#34746,
#34747,#34748,#34749,#34750),.UNSPECIFIED.,.F.,.F.,(4,1,1,1,1,1,4),(0.500408394295939,
0.625,0.6875,0.75,0.8125,0.875,0.99850331800662),.UNSPECIFIED.);
#742=B_SPLINE_CURVE_WITH_KNOTS('',3,(#34752,#34753,#34754,#34755,#34756,
#34757,#34758,#34759,#34760,#34761,#34762,#34763,#34764,#34765,#34766,#34767),
 .UNSPECIFIED.,.F.,.F.,(4,3,3,3,3,4),(0.658287225766538,0.6875,0.716881056108036,
0.75,0.875,0.997623466937086),.UNSPECIFIED.);
#743=B_SPLINE_CURVE_WITH_KNOTS('',3,(#34769,#34770,#34771,#34772,#34773,
#34774,#34775,#34776,#34777,#34778,#34779,#34780,#34781,#34782,#34783,#34784,
#34785,#34786,#34787),.UNSPECIFIED.,.F.,.F.,(4,3,3,3,3,3,4),(0.399644838371795,
0.4375,0.5,0.53125,0.5625,0.625,0.658287225766538),.UNSPECIFIED.);
#744=B_SPLINE_CURVE_WITH_KNOTS('',3,(#34789,#34790,#34791,#34792,#34793,
#34794,#34795,#34796,#34797,#34798,#34799,#34800,#34801,#34802,#34803,#34804,
#34805,#34806,#34807,#34808,#34809,#34810,#34811,#34812,#34813),
 .UNSPECIFIED.,.F.,.F.,(4,3,3,3,3,3,3,3,4),(0.057546946328656,0.125,0.1875,
0.21875,0.25,0.28125,0.3125,0.375,0.399644838371795),.UNSPECIFIED.);
#745=B_SPLINE_CURVE_WITH_KNOTS('',3,(#34815,#34816,#34817,#34818),
 .UNSPECIFIED.,.F.,.F.,(4,4),(6.88941806839869E-6,0.057546946328656),
 .UNSPECIFIED.);
#746=B_SPLINE_CURVE_WITH_KNOTS('',3,(#34820,#34821,#34822,#34823,#34824,
#34825,#34826,#34827,#34828,#34829,#34830,#34831,#34832,#34833,#34834,#34835,
#34836,#34837,#34838,#34839,#34840,#34841,#34842,#34843,#34844,#34845,#34846,
#34847,#34848,#34849,#34850,#34851,#34852,#34853,#34854,#34855,#34856,#34857,
#34858,#34859,#34860,#34861,#34862,#34863,#34864,#34865,#34866,#34867,#34868,
#34869,#34870,#34871),.UNSPECIFIED.,.F.,.F.,(4,3,3,3,3,3,3,3,3,3,3,3,3,
3,3,3,3,4),(0.,0.125,0.1875,0.21875,0.25,0.28125,0.3125,0.375,0.5,0.625,
0.668027506996217,0.75,0.8125,0.84375,0.875,0.90625,0.9375,0.999999676766783),
 .UNSPECIFIED.);
#747=B_SPLINE_CURVE_WITH_KNOTS('',3,(#34873,#34874,#34875,#34876,#34877,
#34878,#34879,#34880,#34881),.UNSPECIFIED.,.F.,.F.,(4,1,1,1,1,1,4),(0.,
0.125,0.1875,0.25,0.3125,0.375,0.499188734755095),.UNSPECIFIED.);
#748=B_SPLINE_CURVE_WITH_KNOTS('',3,(#34883,#34884,#34885,#34886,#34887,
#34888,#34889,#34890,#34891),.UNSPECIFIED.,.F.,.F.,(4,1,1,1,1,1,4),(0.499188734755095,
0.5,0.625,0.75,0.875,0.9375,0.998149180837463),.UNSPECIFIED.);
#749=B_SPLINE_CURVE_WITH_KNOTS('',3,(#34892,#34893,#34894,#34895,#34896,
#34897,#34898,#34899,#34900,#34901,#34902,#34903,#34904,#34905,#34906,#34907,
#34908,#34909,#34910,#34911,#34912,#34913,#34914,#34915,#34916,#34917,#34918,
#34919,#34920,#34921,#34922,#34923,#34924,#34925,#34926,#34927,#34928,#34929,
#34930,#34931,#34932,#34933,#34934,#34935,#34936,#34937,#34938,#34939,#34940,
#34941,#34942,#34943,#34944,#34945,#34946,#34947,#34948,#34949),
 .UNSPECIFIED.,.F.,.F.,(4,3,3,3,3,3,3,3,3,3,3,3,3,3,3,3,3,3,3,4),(0.,0.125,
0.1875,0.21875,0.25,0.28125,0.3125,0.375,0.4375,0.5,0.5625,0.625,0.6875,
0.71875,0.75,0.78125,0.790010298169663,0.8125,0.875,1.),.UNSPECIFIED.);
#750=B_SPLINE_CURVE_WITH_KNOTS('',3,(#35010,#35011,#35012,#35013,#35014,
#35015,#35016,#35017,#35018,#35019,#35020),.UNSPECIFIED.,.F.,.F.,(4,1,1,
1,1,1,1,1,4),(0.867768400737492,0.875,0.90625,0.9375,0.953125,0.96875,0.9765625,
0.984375,1.),.UNSPECIFIED.);
#751=B_SPLINE_CURVE_WITH_KNOTS('',3,(#35021,#35022,#35023,#35024),
 .UNSPECIFIED.,.F.,.F.,(4,4),(0.0677982128913682,0.499948130219197),
 .UNSPECIFIED.);
#752=B_SPLINE_CURVE_WITH_KNOTS('',3,(#35097,#35098,#35099,#35100),
 .UNSPECIFIED.,.F.,.F.,(4,4),(6.03873264751521,6.05787500817515),
 .UNSPECIFIED.);
#753=B_SPLINE_CURVE_WITH_KNOTS('',3,(#35102,#35103,#35104,#35105,#35106,
#35107),.UNSPECIFIED.,.F.,.F.,(4,2,4),(2.5354357802791,2.79846665434659,
2.96491518441833),.UNSPECIFIED.);
#754=B_SPLINE_CURVE_WITH_KNOTS('',3,(#35108,#35109,#35110,#35111),
 .UNSPECIFIED.,.F.,.F.,(4,4),(-0.165387428475329,-0.162180666309789),
 .UNSPECIFIED.);
#755=B_SPLINE_CURVE_WITH_KNOTS('',3,(#35114,#35115,#35116,#35117,#35118,
#35119),.UNSPECIFIED.,.F.,.F.,(4,2,4),(-2.47763566945841,-2.35421341597794,
-2.20494366203894),.UNSPECIFIED.);
#756=B_SPLINE_CURVE_WITH_KNOTS('',3,(#35120,#35121,#35122,#35123),
 .UNSPECIFIED.,.F.,.F.,(4,4),(-10.5382550693381,-10.5290312685128),
 .UNSPECIFIED.);
#757=B_SPLINE_CURVE_WITH_KNOTS('',3,(#35127,#35128,#35129,#35130),
 .UNSPECIFIED.,.F.,.F.,(4,4),(0.,1.),.UNSPECIFIED.);
#758=B_SPLINE_CURVE_WITH_KNOTS('',3,(#35134,#35135,#35136,#35137),
 .UNSPECIFIED.,.F.,.F.,(4,4),(0.,0.502010271881345),.UNSPECIFIED.);
#759=B_SPLINE_CURVE_WITH_KNOTS('',3,(#35139,#35140,#35141,#35142),
 .UNSPECIFIED.,.F.,.F.,(4,4),(0.502010271881345,0.999999999999999),
 .UNSPECIFIED.);
#760=B_SPLINE_CURVE_WITH_KNOTS('',3,(#35149,#35150,#35151,#35152),
 .UNSPECIFIED.,.F.,.F.,(4,4),(0.,0.497989729516545),.UNSPECIFIED.);
#761=B_SPLINE_CURVE_WITH_KNOTS('',3,(#35154,#35155,#35156,#35157),
 .UNSPECIFIED.,.F.,.F.,(4,4),(0.497989729516545,1.),.UNSPECIFIED.);
#762=B_SPLINE_CURVE_WITH_KNOTS('',3,(#35160,#35161,#35162,#35163),
 .UNSPECIFIED.,.F.,.F.,(4,4),(0.,1.),.UNSPECIFIED.);
#763=B_SPLINE_CURVE_WITH_KNOTS('',3,(#35169,#35170,#35171,#35172),
 .UNSPECIFIED.,.F.,.F.,(4,4),(0.,0.501026353593291),.UNSPECIFIED.);
#764=B_SPLINE_CURVE_WITH_KNOTS('',3,(#35174,#35175,#35176,#35177),
 .UNSPECIFIED.,.F.,.F.,(4,4),(0.501026353593291,1.),.UNSPECIFIED.);
#765=B_SPLINE_CURVE_WITH_KNOTS('',3,(#35179,#35180,#35181,#35182,#35183,
#35184,#35185,#35186,#35187,#35188,#35189,#35190),.UNSPECIFIED.,.F.,.F.,
(4,2,2,2,2,4),(1.5151239072314E-5,0.0118829596669569,0.0177755711303306,
0.0198524710636481,0.0207583312220325,0.0215368218022216),.UNSPECIFIED.);
#766=B_SPLINE_CURVE_WITH_KNOTS('',3,(#35191,#35192,#35193,#35194),
 .UNSPECIFIED.,.F.,.F.,(4,4),(0.,1.),.UNSPECIFIED.);
#767=B_SPLINE_CURVE_WITH_KNOTS('',3,(#35198,#35199,#35200,#35201),
 .UNSPECIFIED.,.F.,.F.,(4,4),(0.,1.),.UNSPECIFIED.);
#768=B_SPLINE_CURVE_WITH_KNOTS('',3,(#35205,#35206,#35207,#35208),
 .UNSPECIFIED.,.F.,.F.,(4,4),(0.,0.502010320052747),.UNSPECIFIED.);
#769=B_SPLINE_CURVE_WITH_KNOTS('',3,(#35210,#35211,#35212,#35213),
 .UNSPECIFIED.,.F.,.F.,(4,4),(0.502010320052747,1.),.UNSPECIFIED.);
#770=B_SPLINE_CURVE_WITH_KNOTS('',3,(#35217,#35218,#35219,#35220,#35221,
#35222,#35223,#35224),.UNSPECIFIED.,.F.,.F.,(4,2,2,4),(-3.01857335434641,
-3.01637328016506,-2.78274428831762,-2.67485962322313),.UNSPECIFIED.);
#771=B_SPLINE_CURVE_WITH_KNOTS('',3,(#35225,#35226,#35227,#35228),
 .UNSPECIFIED.,.F.,.F.,(4,4),(-0.274599042102008,-0.00061961661749236),
 .UNSPECIFIED.);
#772=B_SPLINE_CURVE_WITH_KNOTS('',3,(#35388,#35389,#35390,#35391,#35392,
#35393,#35394,#35395,#35396,#35397,#35398,#35399,#35400,#35401,#35402,#35403,
#35404,#35405,#35406,#35407,#35408,#35409),.UNSPECIFIED.,.F.,.F.,(4,3,3,
3,3,3,3,4),(5.10562847884237E-9,0.00374014353849567,0.00748028707699134,
0.00749196373323959,0.00935035884623917,0.011220430615487,0.0130905023847349,
0.0149605741539827),.UNSPECIFIED.);
#773=B_SPLINE_CURVE_WITH_KNOTS('',3,(#35411,#35412,#35413,#35414,#35415,
#35416,#35417,#35418,#35419,#35420,#35421,#35422,#35423,#35424,#35425,#35426,
#35427,#35428,#35429,#35430,#35431,#35432),.UNSPECIFIED.,.F.,.F.,(4,3,3,
3,3,3,3,4),(0.0149612645537521,0.0168306459232305,0.0187007176924783,0.0205707894617261,
0.0224303512848831,0.022440861230974,0.0261810047694697,0.0299211432894142),
 .UNSPECIFIED.);
#774=B_SPLINE_CURVE_WITH_KNOTS('',3,(#35435,#35436,#35437,#35438,#35439,
#35440,#35441,#35442,#35443,#35444,#35445,#35446,#35447,#35448,#35449,#35450,
#35451,#35452,#35453,#35454,#35455,#35456,#35457,#35458,#35459),
 .UNSPECIFIED.,.F.,.F.,(4,3,3,3,3,3,3,3,4),(5.10602741926278E-9,0.00374013872221605,
0.0074802774444321,0.00749195384150005,0.00935034680554015,0.0112204161666482,
0.0130904855277562,0.0149605548888642,0.0158713903754465),.UNSPECIFIED.);
#775=B_SPLINE_CURVE_WITH_KNOTS('',3,(#35463,#35464,#35465,#35466,#35467,
#35468,#35469),.UNSPECIFIED.,.F.,.F.,(4,1,1,1,4),(1.7347234759768E-18,0.00269008839466431,
0.00538017678932861,0.00807026518399292,0.0107603535786572),
 .UNSPECIFIED.);
#776=B_SPLINE_CURVE_WITH_KNOTS('',3,(#35471,#35472,#35473,#35474,#35475,
#35476,#35477,#35478,#35479,#35480,#35481,#35482,#35483,#35484,#35485,#35486,
#35487,#35488,#35489,#35490,#35491,#35492,#35493,#35494,#35495,#35496,#35497,
#35498,#35499,#35500,#35501,#35502,#35503,#35504,#35505,#35506,#35507,#35508,
#35509,#35510),.UNSPECIFIED.,.F.,.F.,(4,3,3,3,3,3,3,3,3,3,3,3,3,4),(1.10894064381892E-8,
0.125,0.25,0.3125,0.375,0.4375,0.46875,0.5,0.53125,0.5625,0.625,0.75,0.875,
0.999999989312939),.UNSPECIFIED.);
#777=B_SPLINE_CURVE_WITH_KNOTS('',3,(#35512,#35513,#35514,#35515,#35516,
#35517,#35518,#35519,#35520,#35521,#35522,#35523,#35524,#35525,#35526,#35527,
#35528,#35529,#35530,#35531,#35532,#35533,#35534,#35535,#35536,#35537,#35538,
#35539,#35540,#35541,#35542,#35543,#35544,#35545,#35546,#35547,#35548,#35549,
#35550,#35551,#35552,#35553,#35554,#35555,#35556,#35557,#35558,#35559,#35560,
#35561,#35562,#35563,#35564,#35565,#35566,#35567,#35568,#35569,#35570,#35571,
#35572),.UNSPECIFIED.,.F.,.F.,(4,3,3,3,3,3,3,3,3,3,3,3,3,3,3,3,3,3,3,3,
4),(1.70073241358158E-10,0.00197446710728151,0.00220015688427838,0.00440031376855676,
0.00512931019723391,0.00550039221069595,0.00625356878405253,0.00660047065283514,
0.00728477966928603,0.00880062753711352,0.00920071084948763,0.0101615955899537,
0.0106616073838042,0.0110007844213919,0.011183305887491,0.0121008628635311,
0.0122880395709336,0.0132009413056703,0.0135642393762939,0.0154010981899487,
0.0176012549038037),.UNSPECIFIED.);
#778=B_SPLINE_CURVE_WITH_KNOTS('',3,(#35574,#35575,#35576,#35577,#35578,
#35579,#35580,#35581,#35582,#35583,#35584,#35585,#35586,#35587,#35588,#35589,
#35590,#35591,#35592,#35593,#35594,#35595,#35596,#35597,#35598,#35599,#35600,
#35601),.UNSPECIFIED.,.F.,.F.,(4,3,3,3,3,3,3,3,3,4),(1.06497082191348E-8,
0.0625,0.125,0.15625,0.1875,0.25,0.375,0.5,0.75,0.999999988547865),
 .UNSPECIFIED.);
#779=B_SPLINE_CURVE_WITH_KNOTS('',3,(#35603,#35604,#35605,#35606,#35607,
#35608,#35609),.UNSPECIFIED.,.F.,.F.,(4,1,1,1,4),(3.33360433782453E-17,
0.00266695541805129,0.00533391083610256,0.00800086625415382,0.0106678216722051),
 .UNSPECIFIED.);
#780=B_SPLINE_CURVE_WITH_KNOTS('',3,(#35613,#35614,#35615,#35616,#35617,
#35618,#35619),.UNSPECIFIED.,.F.,.F.,(4,1,1,1,4),(2.43480042509997E-17,
0.00269008902712854,0.00538017805425706,0.00807026708138558,0.0107603561085141),
 .UNSPECIFIED.);
#781=B_SPLINE_CURVE_WITH_KNOTS('',3,(#35621,#35622,#35623,#35624,#35625,
#35626,#35627,#35628,#35629,#35630,#35631,#35632,#35633,#35634,#35635,#35636,
#35637,#35638,#35639,#35640,#35641,#35642,#35643,#35644,#35645,#35646,#35647,
#35648,#35649,#35650,#35651,#35652,#35653,#35654,#35655,#35656,#35657,#35658,
#35659,#35660),.UNSPECIFIED.,.F.,.F.,(4,3,3,3,3,3,3,3,3,3,3,3,3,4),(1.10899779061613E-8,
0.125,0.25,0.3125,0.375,0.4375,0.46875,0.5,0.53125,0.5625,0.625,0.75,0.875,
0.999999989362077),.UNSPECIFIED.);
#782=B_SPLINE_CURVE_WITH_KNOTS('',3,(#35661,#35662,#35663,#35664,#35665,
#35666,#35667,#35668,#35669,#35670,#35671,#35672,#35673,#35674,#35675,#35676,
#35677,#35678,#35679,#35680,#35681,#35682,#35683,#35684,#35685,#35686,#35687,
#35688,#35689,#35690,#35691,#35692,#35693,#35694,#35695,#35696,#35697,#35698,
#35699,#35700,#35701,#35702,#35703),.UNSPECIFIED.,.F.,.F.,(4,3,3,3,3,3,
3,3,3,3,3,3,3,3,4),(1.70091092863581E-10,0.00197446788219035,0.00220015692671693,
0.00440031385343386,0.00512931098783657,0.00550039231679233,0.00625356907264106,
0.00660047078015079,0.00728477985782865,0.00880062770686772,0.00920071115763201,
0.01016159594726,0.0106616077611924,0.0110007846335847,0.0111833063008374),
 .UNSPECIFIED.);
#783=B_SPLINE_CURVE_WITH_KNOTS('',3,(#35706,#35707,#35708,#35709),
 .UNSPECIFIED.,.F.,.F.,(4,4),(6.55458962298397E-7,1.),.UNSPECIFIED.);
#784=B_SPLINE_CURVE_WITH_KNOTS('',3,(#35711,#35712,#35713,#35714),
 .UNSPECIFIED.,.F.,.F.,(4,4),(3.49092837846564E-8,0.000279639041028945),
 .UNSPECIFIED.);
#785=B_SPLINE_CURVE_WITH_KNOTS('',3,(#35716,#35717,#35718,#35719,#35720,
#35721,#35722,#35723,#35724,#35725),.UNSPECIFIED.,.F.,.F.,(4,2,2,2,4),(5.89420191983957E-6,
0.000303437783884664,0.000632488927968499,0.00143564842888828,0.00301213449051446),
 .UNSPECIFIED.);
#786=B_SPLINE_CURVE_WITH_KNOTS('',3,(#35727,#35728,#35729,#35730),
 .UNSPECIFIED.,.F.,.F.,(4,4),(5.05038109498685E-5,0.999936832443628),
 .UNSPECIFIED.);
#787=B_SPLINE_CURVE_WITH_KNOTS('',3,(#35732,#35733,#35734,#35735,#35736,
#35737,#35738,#35739,#35740,#35741),.UNSPECIFIED.,.F.,.F.,(4,2,2,2,4),(-0.0032145494986627,
-0.00295256209228294,-0.0026513848523457,-0.00194290947785501,-1.68534414557259E-6),
 .UNSPECIFIED.);
#788=B_SPLINE_CURVE_WITH_KNOTS('',3,(#35743,#35744,#35745,#35746),
 .UNSPECIFIED.,.F.,.F.,(4,4),(2.31286388414311E-11,0.000279603602071489),
 .UNSPECIFIED.);
#789=B_SPLINE_CURVE_WITH_KNOTS('',3,(#35747,#35748,#35749,#35750),
 .UNSPECIFIED.,.F.,.F.,(4,4),(0.,1.),.UNSPECIFIED.);
#790=B_SPLINE_CURVE_WITH_KNOTS('',3,(#35753,#35754,#35755,#35756,#35757,
#35758,#35759,#35760,#35761,#35762,#35763,#35764,#35765,#35766,#35767,#35768,
#35769,#35770,#35771,#35772,#35773,#35774,#35775,#35776,#35777,#35778,#35779,
#35780),.UNSPECIFIED.,.F.,.F.,(4,3,3,3,3,3,3,3,3,4),(0.,0.00219009522320418,
0.00438019044640836,0.00547523805801045,0.00657028566961254,0.00876038089281672,
0.0109504761160209,0.012045523727623,0.0131405713392251,0.0146411293071528),
 .UNSPECIFIED.);
#791=B_SPLINE_CURVE_WITH_KNOTS('',3,(#35781,#35782,#35783,#35784,#35785,
#35786,#35787),.UNSPECIFIED.,.F.,.F.,(4,3,4),(0.0146411293071528,0.0153306665624293,
0.0175207617856334),.UNSPECIFIED.);
#792=B_SPLINE_CURVE_WITH_KNOTS('',3,(#35789,#35790,#35791,#35792),
 .UNSPECIFIED.,.F.,.F.,(4,4),(4.55973828920902E-10,0.00219012841858902),
 .UNSPECIFIED.);
#793=B_SPLINE_CURVE_WITH_KNOTS('',3,(#35793,#35794,#35795,#35796,#35797,
#35798,#35799,#35800,#35801,#35802,#35803,#35804,#35805,#35806,#35807,#35808,
#35809,#35810,#35811,#35812,#35813,#35814,#35815,#35816,#35817,#35818,#35819,
#35820),.UNSPECIFIED.,.F.,.F.,(4,3,3,3,3,3,3,3,3,4),(0.00219035076041224,
0.00438070152082448,0.00547587690103059,0.00657105228123671,0.00876140304164895,
0.0109517538020612,0.0120469291822673,0.0131421045624734,0.0153324553228857,
0.0175228056278763),.UNSPECIFIED.);
#794=B_SPLINE_CURVE_WITH_KNOTS('',3,(#35823,#35824,#35825,#35826,#35827,
#35828,#35829,#35830,#35831,#35832,#35833,#35834,#35835,#35836,#35837,#35838,
#35839,#35840,#35841,#35842,#35843,#35844,#35845,#35846,#35847,#35848,#35849,
#35850),.UNSPECIFIED.,.F.,.F.,(4,3,3,3,3,3,3,3,3,4),(0.,0.00219009519209258,
0.00438019038418515,0.00547523798023144,0.00657028557627773,0.0087603807683703,
0.0109504759604629,0.0120455235565092,0.0131405711525555,0.0146411150843174),
 .UNSPECIFIED.);
#795=B_SPLINE_CURVE_WITH_KNOTS('',3,(#35851,#35852,#35853,#35854,#35855,
#35856,#35857),.UNSPECIFIED.,.F.,.F.,(4,3,4),(0.0146411150843174,0.015330666344648,
0.0175207615367406),.UNSPECIFIED.);
#796=B_SPLINE_CURVE_WITH_KNOTS('',3,(#35859,#35860,#35861,#35862),
 .UNSPECIFIED.,.F.,.F.,(4,4),(4.55959294391392E-10,0.00219012846087483),
 .UNSPECIFIED.);
#797=B_SPLINE_CURVE_WITH_KNOTS('',3,(#35863,#35864,#35865,#35866,#35867,
#35868,#35869,#35870,#35871,#35872,#35873,#35874,#35875,#35876,#35877,#35878,
#35879,#35880,#35881,#35882,#35883,#35884,#35885,#35886,#35887,#35888,#35889,
#35890),.UNSPECIFIED.,.F.,.F.,(4,3,3,3,3,3,3,3,3,4),(0.00219035079403417,
0.00438070158806835,0.00547587698508544,0.00657105238210252,0.0087614031761367,
0.0109517539701709,0.012046929367188,0.013142104764205,0.0153324555582392,
0.0175228058968349),.UNSPECIFIED.);
#798=B_SPLINE_CURVE_WITH_KNOTS('',3,(#35893,#35894,#35895,#35896),
 .UNSPECIFIED.,.F.,.F.,(4,4),(6.67616818609268E-7,1.),.UNSPECIFIED.);
#799=B_SPLINE_CURVE_WITH_KNOTS('',3,(#35898,#35899,#35900,#35901),
 .UNSPECIFIED.,.F.,.F.,(4,4),(3.49092066549658E-8,0.000279639070515748),
 .UNSPECIFIED.);
#800=B_SPLINE_CURVE_WITH_KNOTS('',3,(#35903,#35904,#35905,#35906),
 .UNSPECIFIED.,.F.,.F.,(4,4),(0.00344166019661847,0.00347128806463756),
 .UNSPECIFIED.);
#801=B_SPLINE_CURVE_WITH_KNOTS('',3,(#35908,#35909,#35910,#35911),
 .UNSPECIFIED.,.F.,.F.,(4,4),(7.68669616547862E-6,0.999996430487618),
 .UNSPECIFIED.);
#802=B_SPLINE_CURVE_WITH_KNOTS('',3,(#35915,#35916,#35917,#35918),
 .UNSPECIFIED.,.F.,.F.,(4,4),(2.31289797358325E-11,0.000279603631692585),
 .UNSPECIFIED.);
#803=B_SPLINE_CURVE_WITH_KNOTS('',3,(#35919,#35920,#35921,#35922),
 .UNSPECIFIED.,.F.,.F.,(4,4),(0.,1.),.UNSPECIFIED.);
#804=B_SPLINE_CURVE_WITH_KNOTS('',3,(#35928,#35929,#35930,#35931,#35932),
 .UNSPECIFIED.,.F.,.F.,(4,1,4),(3.90312782094781E-18,0.00385428159543372,
0.00770856319086743),.UNSPECIFIED.);
#805=B_SPLINE_CURVE_WITH_KNOTS('',3,(#35934,#35935,#35936,#35937),
 .UNSPECIFIED.,.F.,.F.,(4,4),(0.00770856319086743,0.0115628447863011),
 .UNSPECIFIED.);
#806=B_SPLINE_CURVE_WITH_KNOTS('',3,(#35939,#35940,#35941,#35942),
 .UNSPECIFIED.,.F.,.F.,(4,4),(0.0115628447863011,0.0154171263817349),
 .UNSPECIFIED.);
#807=B_SPLINE_CURVE_WITH_KNOTS('',3,(#35944,#35945,#35946,#35947,#35948,
#35949,#35950),.UNSPECIFIED.,.F.,.F.,(4,1,1,1,4),(0.0154171263817349,0.0192714079771686,
0.0231256895726023,0.026979971168036,0.0308342527634697),.UNSPECIFIED.);
#808=B_SPLINE_CURVE_WITH_KNOTS('',3,(#35953,#35954,#35955,#35956,#35957,
#35958,#35959,#35960,#35961,#35962,#35963,#35964,#35965,#35966,#35967,#35968,
#35969,#35970,#35971,#35972,#35973,#35974,#35975,#35976,#35977),
 .UNSPECIFIED.,.F.,.F.,(4,3,3,3,3,3,3,3,4),(3.49644694633735E-18,0.0038084153469596,
0.00761683069391923,0.0114252460408789,0.0152336613878385,0.0190420767347981,
0.0228504920817577,0.0266589074287173,0.0304673227756769),.UNSPECIFIED.);
#809=B_SPLINE_CURVE_WITH_KNOTS('',3,(#35980,#35981,#35982,#35983,#35984,
#35985,#35986,#35987,#35988,#35989),.UNSPECIFIED.,.F.,.F.,(4,3,3,4),(4.95617171550503E-9,
0.03125,0.0625,0.09375),.UNSPECIFIED.);
#810=B_SPLINE_CURVE_WITH_KNOTS('',3,(#35991,#35992,#35993,#35994,#35995,
#35996,#35997,#35998,#35999,#36000,#36001,#36002,#36003,#36004,#36005,#36006,
#36007,#36008,#36009),.UNSPECIFIED.,.F.,.F.,(4,3,3,3,3,3,4),(0.09375,0.125,
0.15625,0.1875,0.21875,0.25,0.28125),.UNSPECIFIED.);
#811=B_SPLINE_CURVE_WITH_KNOTS('',3,(#36011,#36012,#36013,#36014,#36015,
#36016,#36017,#36018,#36019,#36020,#36021,#36022,#36023,#36024,#36025,#36026),
 .UNSPECIFIED.,.F.,.F.,(4,3,3,3,3,4),(0.28125,0.3125,0.375,0.5,0.625,0.658880396082507),
 .UNSPECIFIED.);
#812=B_SPLINE_CURVE_WITH_KNOTS('',3,(#36028,#36029,#36030,#36031,#36032,
#36033,#36034,#36035,#36036,#36037,#36038,#36039,#36040,#36041,#36042,#36043,
#36044,#36045,#36046,#36047,#36048,#36049,#36050,#36051,#36052),
 .UNSPECIFIED.,.F.,.F.,(4,3,3,3,3,3,3,3,4),(0.658880396082507,0.6875,0.71875,
0.75,0.78125,0.8125,0.84375,0.875,0.901787328791184),.UNSPECIFIED.);
#813=B_SPLINE_CURVE_WITH_KNOTS('',3,(#36054,#36055,#36056,#36057,#36058,
#36059,#36060,#36061,#36062,#36063,#36064,#36065,#36066),.UNSPECIFIED.,
 .F.,.F.,(4,3,3,3,4),(0.901787328791184,0.90625,0.9375,0.96875,0.999999995039462),
 .UNSPECIFIED.);
#814=B_SPLINE_CURVE_WITH_KNOTS('',3,(#36070,#36071,#36072,#36073,#36074,
#36075,#36076,#36077,#36078,#36079),.UNSPECIFIED.,.F.,.F.,(4,3,3,4),(0.,
0.03125,0.0625,0.078125),.UNSPECIFIED.);
#815=B_SPLINE_CURVE_WITH_KNOTS('',3,(#36081,#36082,#36083,#36084,#36085,
#36086,#36087,#36088,#36089,#36090,#36091,#36092,#36093,#36094,#36095,#36096,
#36097,#36098,#36099,#36100,#36101,#36102),.UNSPECIFIED.,.F.,.F.,(4,3,3,
3,3,3,3,4),(0.078125,0.09375,0.125,0.15625,0.1875,0.21875,0.25,0.28125),
 .UNSPECIFIED.);
#816=B_SPLINE_CURVE_WITH_KNOTS('',3,(#36104,#36105,#36106,#36107,#36108,
#36109,#36110,#36111,#36112,#36113,#36114,#36115,#36116,#36117,#36118,#36119),
 .UNSPECIFIED.,.F.,.F.,(4,3,3,3,3,4),(0.28125,0.3125,0.375,0.5,0.625,0.658099954027992),
 .UNSPECIFIED.);
#817=B_SPLINE_CURVE_WITH_KNOTS('',3,(#36121,#36122,#36123,#36124,#36125,
#36126,#36127,#36128,#36129,#36130,#36131,#36132,#36133,#36134,#36135,#36136,
#36137,#36138,#36139,#36140,#36141,#36142,#36143,#36144,#36145),
 .UNSPECIFIED.,.F.,.F.,(4,3,3,3,3,3,3,3,4),(0.658099954027992,0.6875,0.71875,
0.75,0.78125,0.8125,0.84375,0.875,0.899951537400222),.UNSPECIFIED.);
#818=B_SPLINE_CURVE_WITH_KNOTS('',3,(#36146,#36147,#36148,#36149,#36150,
#36151,#36152,#36153,#36154,#36155,#36156,#36157,#36158,#36159,#36160,#36161),
 .UNSPECIFIED.,.F.,.F.,(4,3,3,3,3,4),(0.899951537400222,0.90625,0.921875,
0.9375,0.96875,1.),.UNSPECIFIED.);
#819=B_SPLINE_CURVE_WITH_KNOTS('',3,(#36167,#36168,#36169,#36170,#36171,
#36172,#36173,#36174,#36175,#36176),.UNSPECIFIED.,.F.,.F.,(4,3,3,4),(4.95657091019873E-9,
0.03125,0.0625,0.09375),.UNSPECIFIED.);
#820=B_SPLINE_CURVE_WITH_KNOTS('',3,(#36178,#36179,#36180,#36181,#36182,
#36183,#36184,#36185,#36186,#36187,#36188,#36189,#36190,#36191,#36192,#36193,
#36194,#36195,#36196),.UNSPECIFIED.,.F.,.F.,(4,3,3,3,3,3,4),(0.09375,0.125,
0.15625,0.1875,0.21875,0.25,0.28125),.UNSPECIFIED.);
#821=B_SPLINE_CURVE_WITH_KNOTS('',3,(#36198,#36199,#36200,#36201,#36202,
#36203,#36204,#36205,#36206,#36207,#36208,#36209,#36210,#36211,#36212,#36213),
 .UNSPECIFIED.,.F.,.F.,(4,3,3,3,3,4),(0.28125,0.3125,0.375,0.5,0.625,0.658881231743818),
 .UNSPECIFIED.);
#822=B_SPLINE_CURVE_WITH_KNOTS('',3,(#36215,#36216,#36217,#36218,#36219,
#36220,#36221,#36222,#36223,#36224,#36225,#36226,#36227,#36228,#36229,#36230,
#36231,#36232,#36233,#36234,#36235,#36236,#36237,#36238,#36239),
 .UNSPECIFIED.,.F.,.F.,(4,3,3,3,3,3,3,3,4),(0.658881231743818,0.6875,0.71875,
0.75,0.78125,0.8125,0.84375,0.875,0.901786418266221),.UNSPECIFIED.);
#823=B_SPLINE_CURVE_WITH_KNOTS('',3,(#36240,#36241,#36242,#36243,#36244,
#36245,#36246,#36247,#36248,#36249,#36250,#36251,#36252),.UNSPECIFIED.,
 .F.,.F.,(4,3,3,3,4),(0.901786418266221,0.90625,0.9375,0.96875,0.999999995039868),
 .UNSPECIFIED.);
#824=B_SPLINE_CURVE_WITH_KNOTS('',3,(#36254,#36255,#36256,#36257,#36258,
#36259,#36260,#36261,#36262,#36263),.UNSPECIFIED.,.F.,.F.,(4,3,3,4),(0.,
0.03125,0.0625,0.078125),.UNSPECIFIED.);
#825=B_SPLINE_CURVE_WITH_KNOTS('',3,(#36265,#36266,#36267,#36268,#36269,
#36270,#36271,#36272,#36273,#36274,#36275,#36276,#36277,#36278,#36279,#36280,
#36281,#36282,#36283,#36284,#36285,#36286),.UNSPECIFIED.,.F.,.F.,(4,3,3,
3,3,3,3,4),(0.078125,0.09375,0.125,0.15625,0.1875,0.21875,0.25,0.28125),
 .UNSPECIFIED.);
#826=B_SPLINE_CURVE_WITH_KNOTS('',3,(#36288,#36289,#36290,#36291,#36292,
#36293,#36294,#36295,#36296,#36297,#36298,#36299,#36300,#36301,#36302,#36303),
 .UNSPECIFIED.,.F.,.F.,(4,3,3,3,3,4),(0.28125,0.3125,0.375,0.5,0.625,0.658099136367619),
 .UNSPECIFIED.);
#827=B_SPLINE_CURVE_WITH_KNOTS('',3,(#36305,#36306,#36307,#36308,#36309,
#36310,#36311,#36312,#36313,#36314,#36315,#36316,#36317,#36318,#36319,#36320,
#36321,#36322,#36323,#36324,#36325,#36326,#36327,#36328,#36329),
 .UNSPECIFIED.,.F.,.F.,(4,3,3,3,3,3,3,3,4),(0.658099136367619,0.6875,0.71875,
0.75,0.78125,0.8125,0.84375,0.875,0.899952381870881),.UNSPECIFIED.);
#828=B_SPLINE_CURVE_WITH_KNOTS('',3,(#36330,#36331,#36332,#36333,#36334,
#36335,#36336,#36337,#36338,#36339,#36340,#36341,#36342,#36343,#36344,#36345),
 .UNSPECIFIED.,.F.,.F.,(4,3,3,3,3,4),(0.899952381870881,0.90625,0.921875,
0.9375,0.96875,1.),.UNSPECIFIED.);
#829=B_SPLINE_CURVE_WITH_KNOTS('',3,(#36348,#36349,#36350,#36351,#36352),
 .UNSPECIFIED.,.F.,.F.,(4,1,4),(2.21134721367331E-18,0.00385428119363376,
0.00770856238726751),.UNSPECIFIED.);
#830=B_SPLINE_CURVE_WITH_KNOTS('',3,(#36354,#36355,#36356,#36357),
 .UNSPECIFIED.,.F.,.F.,(4,4),(0.00770856238726751,0.0115628435809013),
 .UNSPECIFIED.);
#831=B_SPLINE_CURVE_WITH_KNOTS('',3,(#36359,#36360,#36361,#36362),
 .UNSPECIFIED.,.F.,.F.,(4,4),(0.0115628435809013,0.015417124774535),
 .UNSPECIFIED.);
#832=B_SPLINE_CURVE_WITH_KNOTS('',3,(#36363,#36364,#36365,#36366,#36367,
#36368,#36369),.UNSPECIFIED.,.F.,.F.,(4,1,1,1,4),(0.015417124774535,0.0192714059681688,
0.0231256871618025,0.0269799683554363,0.0308342495490701),.UNSPECIFIED.);
#833=B_SPLINE_CURVE_WITH_KNOTS('',3,(#36370,#36371,#36372,#36373,#36374,
#36375,#36376,#36377,#36378,#36379,#36380,#36381,#36382,#36383,#36384,#36385,
#36386,#36387,#36388,#36389,#36390,#36391,#36392,#36393,#36394),
 .UNSPECIFIED.,.F.,.F.,(4,3,3,3,3,3,3,3,4),(3.03576608295941E-18,0.00380841492928532,
0.00761682985857062,0.0114252447878558,0.0152336597171411,0.0190420746464265,
0.0228504895757117,0.026658904504997,0.0304673194342823),.UNSPECIFIED.);
#834=B_SPLINE_CURVE_WITH_KNOTS('',3,(#36397,#36398,#36399,#36400,#36401,
#36402,#36403),.UNSPECIFIED.,.F.,.F.,(4,1,1,1,4),(5.23213817258733E-8,0.0029056070149641,
0.00581121402992687,0.00871682104488963,0.0116224280598524),
 .UNSPECIFIED.);
#835=B_SPLINE_CURVE_WITH_KNOTS('',3,(#36406,#36407,#36408,#36409,#36410,
#36411,#36412,#36413,#36414,#36415,#36416,#36417,#36418,#36419,#36420,#36421,
#36422,#36423,#36424,#36425,#36426,#36427,#36428,#36429,#36430,#36431,#36432,
#36433,#36434,#36435,#36436),.UNSPECIFIED.,.F.,.F.,(4,3,3,3,3,3,3,3,3,3,
4),(0.000307410351405465,0.0030481449392632,0.0030636165255644,0.00441851223319206,
0.00578887952712092,0.00581844748756307,0.00715924682104978,0.00852961411497865,
0.00857611852702666,0.00989998140890752,0.0112703487028364),
 .UNSPECIFIED.);
#836=B_SPLINE_CURVE_WITH_KNOTS('',3,(#36439,#36440,#36441,#36442,#36443,
#36444,#36445),.UNSPECIFIED.,.F.,.F.,(4,1,1,1,4),(3.65940318147201E-17,
0.00281356312006687,0.00562712624013371,0.00844068936020054,0.0112542524802674),
 .UNSPECIFIED.);
#837=B_SPLINE_CURVE_WITH_KNOTS('',3,(#36447,#36448,#36449,#36450,#36451,
#36452,#36453,#36454,#36455,#36456,#36457,#36458,#36459),.UNSPECIFIED.,
 .F.,.F.,(4,3,3,3,4),(0.,0.25,0.5,0.75,0.999991910881764),.UNSPECIFIED.);
#838=B_SPLINE_CURVE_WITH_KNOTS('',3,(#36460,#36461,#36462,#36463,#36464,
#36465,#36466),.UNSPECIFIED.,.F.,.F.,(4,1,1,1,4),(0.000444700170075515,
0.00338593218391437,0.00632716419775323,0.00926839621159208,0.0122095755614429),
 .UNSPECIFIED.);
#839=B_SPLINE_CURVE_WITH_KNOTS('',3,(#36471,#36472,#36473,#36474,#36475,
#36476,#36477),.UNSPECIFIED.,.F.,.F.,(4,1,1,1,4),(1.46628880702953E-15,
0.00294691748194268,0.0058938349638839,0.00884075244582512,0.0117876171100227),
 .UNSPECIFIED.);
#840=B_SPLINE_CURVE_WITH_KNOTS('',3,(#36478,#36479,#36480,#36481,#36482,
#36483,#36484),.UNSPECIFIED.,.F.,.F.,(4,1,1,1,4),(9.42515350988308E-17,
0.00274256564248042,0.00548513128496075,0.00822769692744107,0.0109702625699214),
 .UNSPECIFIED.);
#841=B_SPLINE_CURVE_WITH_KNOTS('',3,(#36487,#36488,#36489,#36490,#36491,
#36492,#36493),.UNSPECIFIED.,.F.,.F.,(4,1,1,1,4),(5.24770762208555E-8,0.0029075980930468,
0.00581519618608887,0.00872279427913093,0.011630392372173),
 .UNSPECIFIED.);
#842=B_SPLINE_CURVE_WITH_KNOTS('',3,(#36496,#36497,#36498,#36499,#36500,
#36501,#36502,#36503,#36504,#36505,#36506,#36507,#36508,#36509,#36510,#36511,
#36512,#36513,#36514,#36515,#36516,#36517,#36518,#36519,#36520,#36521,#36522,
#36523,#36524,#36525,#36526),.UNSPECIFIED.,.F.,.F.,(4,3,3,3,3,3,3,3,3,3,
4),(0.000307411164707473,0.00304814514067886,0.00306361677010575,0.00441851212866456,
0.00578887911665026,0.00581844712117058,0.00715924610463596,0.00852961309262165,
0.00857611755053204,0.00989998008060733,0.011270347068593),
 .UNSPECIFIED.);
#843=B_SPLINE_CURVE_WITH_KNOTS('',3,(#36569,#36570,#36571,#36572,#36573,
#36574,#36575),.UNSPECIFIED.,.F.,.F.,(4,3,4),(1.7082471228229E-5,0.825036313420024,
1.),.UNSPECIFIED.);
#844=B_SPLINE_CURVE_WITH_KNOTS('',3,(#36599,#36600,#36601,#36602,#36603,
#36604),.UNSPECIFIED.,.F.,.F.,(4,2,4),(-0.0126200035614453,-0.00663868323303364,
-1.51764961458753E-5),.UNSPECIFIED.);
#845=B_SPLINE_CURVE_WITH_KNOTS('',3,(#36605,#36606,#36607,#36608,#36609,
#36610,#36611),.UNSPECIFIED.,.F.,.F.,(4,3,4),(0.,0.632718071204813,0.999999748705075),
 .UNSPECIFIED.);
#846=B_SPLINE_CURVE_WITH_KNOTS('',3,(#36634,#36635,#36636,#36637,#36638,
#36639,#36640),.UNSPECIFIED.,.F.,.F.,(4,3,4),(2.03490870871502E-6,0.698513719527809,
1.),.UNSPECIFIED.);
#847=B_SPLINE_CURVE_WITH_KNOTS('',3,(#36642,#36643,#36644,#36645,#36646,
#36647,#36648),.UNSPECIFIED.,.F.,.F.,(4,3,4),(2.56083752551901E-7,0.698445555099148,
0.9999999084914),.UNSPECIFIED.);
#848=B_SPLINE_CURVE_WITH_KNOTS('',3,(#36650,#36651,#36652,#36653,#36654,
#36655,#36656),.UNSPECIFIED.,.F.,.F.,(4,3,4),(4.92776746415909E-7,0.6333331216261,
0.999995687372378),.UNSPECIFIED.);
#849=B_SPLINE_CURVE_WITH_KNOTS('',3,(#36779,#36780,#36781,#36782,#36783,
#36784,#36785),.UNSPECIFIED.,.F.,.F.,(4,3,4),(0.,0.861053093920219,1.),
 .UNSPECIFIED.);
#850=B_SPLINE_CURVE_WITH_KNOTS('',3,(#36786,#36787,#36788,#36789,#36790,
#36791,#36792),.UNSPECIFIED.,.F.,.F.,(4,3,4),(0.,0.861042149630975,1.),
 .UNSPECIFIED.);
#851=B_SPLINE_CURVE_WITH_KNOTS('',3,(#36794,#36795,#36796,#36797,#36798,
#36799,#36800),.UNSPECIFIED.,.F.,.F.,(4,3,4),(0.,0.861053136203872,1.),
 .UNSPECIFIED.);
#852=B_SPLINE_CURVE_WITH_KNOTS('',3,(#36802,#36803,#36804,#36805,#36806,
#36807,#36808),.UNSPECIFIED.,.F.,.F.,(4,3,4),(0.,0.861042192136075,1.),
 .UNSPECIFIED.);
#853=B_SPLINE_CURVE_WITH_KNOTS('',3,(#36913,#36914,#36915,#36916,#36917,
#36918,#36919),.UNSPECIFIED.,.F.,.F.,(4,3,4),(0.,0.730996929438668,1.),
 .UNSPECIFIED.);
#854=B_SPLINE_CURVE_WITH_KNOTS('',3,(#36922,#36923,#36924,#36925,#36926,
#36927,#36928),.UNSPECIFIED.,.F.,.F.,(4,3,4),(0.,0.770155557257018,1.),
 .UNSPECIFIED.);
#855=B_SPLINE_CURVE_WITH_KNOTS('',3,(#36953,#36954,#36955,#36956,#36957,
#36958,#36959),.UNSPECIFIED.,.F.,.F.,(4,3,4),(0.,0.730997037997434,1.),
 .UNSPECIFIED.);
#856=B_SPLINE_CURVE_WITH_KNOTS('',3,(#36988,#36989,#36990,#36991,#36992,
#36993,#36994),.UNSPECIFIED.,.F.,.F.,(4,3,4),(0.,0.770155702463764,1.),
 .UNSPECIFIED.);
#857=B_SPLINE_CURVE_WITH_KNOTS('',3,(#37016,#37017,#37018,#37019),
 .UNSPECIFIED.,.F.,.F.,(4,4),(0.,1.),.UNSPECIFIED.);
#858=B_SPLINE_CURVE_WITH_KNOTS('',3,(#37148,#37149,#37150,#37151),
 .UNSPECIFIED.,.F.,.F.,(4,4),(-0.705935800703831,-0.696391995080821),
 .UNSPECIFIED.);
#859=B_SPLINE_CURVE_WITH_KNOTS('',3,(#37293,#37294,#37295,#37296,#37297,
#37298,#37299,#37300,#37301,#37302),.UNSPECIFIED.,.F.,.F.,(4,3,3,4),(0.00380005432105398,
0.00387434298579466,0.00432138238092229,0.00476842177604991),
 .UNSPECIFIED.);
#860=B_SPLINE_CURVE_WITH_KNOTS('',3,(#37304,#37305,#37306,#37307,#37308,
#37309),.UNSPECIFIED.,.F.,.F.,(4,2,4),(3.88881683081212E-5,0.0373227534595625,
0.0745507150811631),.UNSPECIFIED.);
#861=B_SPLINE_CURVE_WITH_KNOTS('',3,(#37313,#37314,#37315,#37316,#37317,
#37318),.UNSPECIFIED.,.F.,.F.,(4,2,4),(-0.0999913936388849,-0.0500013329569702,
-4.68222846500675E-6),.UNSPECIFIED.);
#862=B_SPLINE_CURVE_WITH_KNOTS('',3,(#37322,#37323,#37324,#37325,#37326,
#37327),.UNSPECIFIED.,.F.,.F.,(4,2,4),(0.000679649455705054,0.0157748102346675,
0.0307661125813358),.UNSPECIFIED.);
#863=B_SPLINE_CURVE_WITH_KNOTS('',3,(#37328,#37329,#37330,#37331,#37332,
#37333),.UNSPECIFIED.,.F.,.F.,(4,2,4),(4.78528932733694E-5,0.047856719715927,
0.0963109409074384),.UNSPECIFIED.);
#864=B_SPLINE_CURVE_WITH_KNOTS('',3,(#37337,#37338,#37339,#37340,#37341,
#37342,#37343,#37344,#37345,#37346,#37347,#37348,#37349,#37350,#37351,#37352,
#37353),.UNSPECIFIED.,.F.,.F.,(4,1,1,1,1,1,1,1,1,1,1,1,1,1,4),(0.,0.125,
0.1875,0.25,0.3125,0.375,0.5,0.625,0.6875,0.71875,0.75,0.78125,0.8125,0.875,
1.),.UNSPECIFIED.);
#865=B_SPLINE_CURVE_WITH_KNOTS('',3,(#37355,#37356,#37357,#37358,#37359,
#37360,#37361,#37362),.UNSPECIFIED.,.F.,.F.,(4,2,2,4),(0.725687494856636,
0.750372622948823,0.818321739027402,0.830322368571011),.UNSPECIFIED.);
#866=B_SPLINE_CURVE_WITH_KNOTS('',3,(#37364,#37365,#37366,#37367),
 .UNSPECIFIED.,.F.,.F.,(4,4),(-1.14929610836797,-1.05359988011008),
 .UNSPECIFIED.);
#867=B_SPLINE_CURVE_WITH_KNOTS('',3,(#37369,#37370,#37371,#37372,#37373,
#37374,#37375,#37376,#37377,#37378,#37379,#37380,#37381,#37382,#37383,#37384,
#37385),.UNSPECIFIED.,.F.,.F.,(4,1,1,1,1,1,1,1,1,1,1,1,1,1,4),(0.,0.125,
0.1875,0.25,0.3125,0.375,0.5,0.625,0.6875,0.71875,0.75,0.78125,0.8125,0.875,
0.999999992807185),.UNSPECIFIED.);
#868=B_SPLINE_CURVE_WITH_KNOTS('',3,(#37387,#37388,#37389,#37390,#37391,
#37392,#37393,#37394,#37395,#37396,#37397,#37398,#37399,#37400,#37401,#37402,
#37403),.UNSPECIFIED.,.F.,.F.,(4,1,1,1,1,1,1,1,1,1,1,1,1,1,4),(4.6260540190425E-9,
0.125,0.1875,0.21875,0.25,0.28125,0.3125,0.375,0.5,0.625,0.6875,0.75,0.8125,
0.875,1.),.UNSPECIFIED.);
#869=B_SPLINE_CURVE_WITH_KNOTS('',3,(#37404,#37405,#37406,#37407),
 .UNSPECIFIED.,.F.,.F.,(4,4),(-1.14869222711582,-1.05773312703723),
 .UNSPECIFIED.);
#870=B_SPLINE_CURVE_WITH_KNOTS('',3,(#37411,#37412,#37413,#37414,#37415,
#37416,#37417,#37418,#37419,#37420,#37421,#37422,#37423,#37424,#37425,#37426,
#37427),.UNSPECIFIED.,.F.,.F.,(4,1,1,1,1,1,1,1,1,1,1,1,1,1,4),(0.,0.125,
0.1875,0.25,0.3125,0.375,0.5,0.625,0.6875,0.71875,0.75,0.78125,0.8125,0.875,
1.),.UNSPECIFIED.);
#871=B_SPLINE_CURVE_WITH_KNOTS('',3,(#37429,#37430,#37431,#37432,#37433,
#37434,#37435,#37436,#37437,#37438,#37439,#37440,#37441,#37442,#37443,#37444,
#37445,#37446,#37447,#37448,#37449),.UNSPECIFIED.,.F.,.F.,(4,1,1,1,1,1,
1,1,1,1,1,1,1,1,1,1,1,1,4),(1.38893867511916E-7,0.03125,0.0625,0.125,0.1875,
0.21875,0.25,0.28125,0.3125,0.375,0.5,0.625,0.6875,0.71875,0.75,0.78125,
0.8125,0.875,1.),.UNSPECIFIED.);
#872=B_SPLINE_CURVE_WITH_KNOTS('',3,(#37451,#37452,#37453,#37454),
 .UNSPECIFIED.,.F.,.F.,(4,4),(-1.13334392424363,-1.03901243078379),
 .UNSPECIFIED.);
#873=B_SPLINE_CURVE_WITH_KNOTS('',3,(#37456,#37457,#37458,#37459,#37460,
#37461,#37462,#37463,#37464,#37465,#37466,#37467,#37468,#37469,#37470,#37471,
#37472),.UNSPECIFIED.,.F.,.F.,(4,1,1,1,1,1,1,1,1,1,1,1,1,1,4),(0.,0.125,
0.1875,0.25,0.3125,0.375,0.5,0.625,0.6875,0.71875,0.75,0.78125,0.8125,0.875,
1.),.UNSPECIFIED.);
#874=B_SPLINE_CURVE_WITH_KNOTS('',3,(#37474,#37475,#37476,#37477,#37478,
#37479,#37480,#37481,#37482,#37483,#37484,#37485,#37486,#37487,#37488,#37489,
#37490,#37491,#37492),.UNSPECIFIED.,.F.,.F.,(4,1,1,1,1,1,1,1,1,1,1,1,1,
1,1,1,4),(0.,0.125,0.1875,0.21875,0.25,0.28125,0.3125,0.375,0.5,0.625,0.6875,
0.71875,0.75,0.78125,0.8125,0.875,1.),.UNSPECIFIED.);
#875=B_SPLINE_CURVE_WITH_KNOTS('',3,(#37493,#37494,#37495,#37496),
 .UNSPECIFIED.,.F.,.F.,(4,4),(-1.14029447472564,-1.04889589827956),
 .UNSPECIFIED.);
#876=B_SPLINE_CURVE_WITH_KNOTS('',3,(#37500,#37501,#37502,#37503,#37504,
#37505,#37506,#37507,#37508,#37509,#37510,#37511,#37512,#37513,#37514,#37515,
#37516,#37517,#37518,#37519,#37520,#37521,#37522,#37523,#37524,#37525,#37526,
#37527,#37528,#37529,#37530,#37531,#37532,#37533,#37534,#37535,#37536,#37537,
#37538,#37539,#37540,#37541,#37542,#37543,#37544,#37545,#37546,#37547,#37548),
 .UNSPECIFIED.,.F.,.F.,(4,3,3,3,3,3,3,3,3,3,3,3,3,3,3,3,4),(0.,0.125,0.1875,
0.21875,0.25,0.28125,0.3125,0.375,0.5,0.625,0.6875,0.71875,0.75,0.78125,
0.8125,0.875,1.),.UNSPECIFIED.);
#877=B_SPLINE_CURVE_WITH_KNOTS('',3,(#37550,#37551,#37552,#37553,#37554,
#37555,#37556,#37557,#37558,#37559,#37560,#37561,#37562,#37563,#37564,#37565,
#37566,#37567,#37568),.UNSPECIFIED.,.F.,.F.,(4,1,1,1,1,1,1,1,1,1,1,1,1,
1,1,1,4),(2.20369844643671E-7,0.125000167295231,0.187500155345571,0.218750149370742,
0.250000143395912,0.281250137421082,0.312500131446253,0.375000119496593,
0.500000095597275,0.625000071697956,0.687500059748297,0.718750053773467,
0.750000047798637,0.781250041823808,0.812500035848978,0.875000023899319,
1.),.UNSPECIFIED.);
#878=B_SPLINE_CURVE_WITH_KNOTS('',3,(#37570,#37571,#37572,#37573),
 .UNSPECIFIED.,.F.,.F.,(4,4),(-1.13396995922952,-1.03919754738596),
 .UNSPECIFIED.);
#879=B_SPLINE_CURVE_WITH_KNOTS('',3,(#37575,#37576,#37577,#37578,#37579,
#37580,#37581,#37582,#37583,#37584,#37585,#37586,#37587,#37588,#37589,#37590,
#37591,#37592,#37593),.UNSPECIFIED.,.F.,.F.,(4,1,1,1,1,1,1,1,1,1,1,1,1,
1,1,1,4),(0.,0.125,0.1875,0.21875,0.25,0.28125,0.3125,0.375,0.5,0.625,0.6875,
0.71875,0.75,0.78125,0.8125,0.875,1.),.UNSPECIFIED.);
#880=B_SPLINE_CURVE_WITH_KNOTS('',3,(#37595,#37596,#37597,#37598,#37599,
#37600,#37601,#37602,#37603,#37604,#37605,#37606,#37607,#37608,#37609,#37610,
#37611,#37612,#37613,#37614,#37615,#37616,#37617,#37618,#37619,#37620,#37621,
#37622,#37623,#37624,#37625,#37626,#37627,#37628,#37629,#37630,#37631,#37632,
#37633,#37634,#37635,#37636,#37637,#37638,#37639,#37640,#37641,#37642,#37643),
 .UNSPECIFIED.,.F.,.F.,(4,3,3,3,3,3,3,3,3,3,3,3,3,3,3,3,4),(3.09854816786387E-7,
0.125000271122965,0.187500251757039,0.218750242074076,0.250000232391113,
0.28125022270815,0.312500213025186,0.37500019365926,0.500000154927408,0.625000116195556,
0.68750009682963,0.718750087146667,0.750000077463704,0.781250067780741,
0.812500058097778,0.875000038731852,1.),.UNSPECIFIED.);
#881=B_SPLINE_CURVE_WITH_KNOTS('',3,(#37644,#37645,#37646,#37647),
 .UNSPECIFIED.,.F.,.F.,(4,4),(-1.13870654772476,-1.04617847256649),
 .UNSPECIFIED.);
#882=B_SPLINE_CURVE_WITH_KNOTS('',3,(#37651,#37652,#37653,#37654,#37655,
#37656,#37657,#37658,#37659,#37660,#37661,#37662,#37663,#37664,#37665,#37666,
#37667,#37668,#37669,#37670,#37671,#37672,#37673,#37674,#37675,#37676,#37677,
#37678,#37679,#37680,#37681,#37682,#37683,#37684,#37685,#37686,#37687,#37688,
#37689,#37690,#37691,#37692,#37693,#37694,#37695,#37696,#37697,#37698,#37699),
 .UNSPECIFIED.,.F.,.F.,(4,3,3,3,3,3,3,3,3,3,3,3,3,3,3,3,4),(0.,0.125,0.1875,
0.21875,0.25,0.28125,0.3125,0.375,0.5,0.625,0.6875,0.71875,0.75,0.78125,
0.8125,0.875,1.),.UNSPECIFIED.);
#883=B_SPLINE_CURVE_WITH_KNOTS('',3,(#37701,#37702,#37703,#37704,#37705,
#37706,#37707,#37708,#37709,#37710,#37711,#37712,#37713,#37714,#37715,#37716,
#37717,#37718,#37719),.UNSPECIFIED.,.F.,.F.,(4,1,1,1,1,1,1,1,1,1,1,1,1,
1,1,1,4),(1.47023832197186E-7,0.125,0.1875,0.21875,0.25,0.28125,0.3125,
0.375,0.5,0.625,0.6875,0.71875,0.75,0.78125,0.8125,0.875,1.),
 .UNSPECIFIED.);
#884=B_SPLINE_CURVE_WITH_KNOTS('',3,(#37721,#37722,#37723,#37724),
 .UNSPECIFIED.,.F.,.F.,(4,4),(-1.13203448436853,-1.03921975837767),
 .UNSPECIFIED.);
#885=B_SPLINE_CURVE_WITH_KNOTS('',3,(#37726,#37727,#37728,#37729,#37730,
#37731,#37732,#37733,#37734,#37735,#37736,#37737,#37738,#37739,#37740,#37741,
#37742,#37743,#37744,#37745,#37746,#37747,#37748,#37749,#37750,#37751,#37752,
#37753,#37754,#37755,#37756,#37757,#37758,#37759,#37760,#37761,#37762,#37763,
#37764,#37765,#37766,#37767,#37768,#37769,#37770,#37771,#37772,#37773,#37774),
 .UNSPECIFIED.,.F.,.F.,(4,3,3,3,3,3,3,3,3,3,3,3,3,3,3,3,4),(0.,0.125,0.1875,
0.21875,0.25,0.28125,0.3125,0.375,0.5,0.625,0.6875,0.71875,0.75,0.78125,
0.8125,0.875,1.),.UNSPECIFIED.);
#886=B_SPLINE_CURVE_WITH_KNOTS('',3,(#37776,#37777,#37778,#37779,#37780,
#37781,#37782,#37783,#37784,#37785,#37786,#37787,#37788,#37789,#37790,#37791,
#37792,#37793,#37794,#37795,#37796,#37797,#37798,#37799,#37800,#37801,#37802,
#37803,#37804,#37805,#37806,#37807,#37808,#37809,#37810,#37811,#37812,#37813,
#37814,#37815,#37816,#37817,#37818,#37819,#37820,#37821,#37822,#37823,#37824,
#37825,#37826,#37827,#37828,#37829,#37830,#37831,#37832,#37833,#37834,#37835,
#37836,#37837,#37838,#37839),.UNSPECIFIED.,.F.,.F.,(4,3,3,3,3,3,3,3,3,3,
3,3,3,3,3,3,3,3,3,3,3,4),(0.,0.0078125,0.015625,0.03125,0.0625,0.09375,
0.125,0.1875,0.21875,0.25,0.28125,0.3125,0.375,0.5,0.625,0.6875,0.71875,
0.75,0.78125,0.8125,0.875,1.),.UNSPECIFIED.);
#887=B_SPLINE_CURVE_WITH_KNOTS('',3,(#37840,#37841,#37842,#37843),
 .UNSPECIFIED.,.F.,.F.,(4,4),(-1.14623761520631,-1.05526208703702),
 .UNSPECIFIED.);
#888=B_SPLINE_CURVE_WITH_KNOTS('',3,(#37847,#37848,#37849,#37850,#37851,
#37852,#37853,#37854,#37855,#37856,#37857,#37858,#37859,#37860,#37861,#37862,
#37863),.UNSPECIFIED.,.F.,.F.,(4,1,1,1,1,1,1,1,1,1,1,1,1,1,4),(0.,0.125,
0.1875,0.25,0.3125,0.375,0.5,0.625,0.6875,0.71875,0.75,0.78125,0.8125,0.875,
1.),.UNSPECIFIED.);
#889=B_SPLINE_CURVE_WITH_KNOTS('',3,(#37865,#37866,#37867,#37868,#37869,
#37870,#37871,#37872,#37873,#37874,#37875,#37876,#37877,#37878,#37879,#37880,
#37881,#37882,#37883,#37884),.UNSPECIFIED.,.F.,.F.,(4,1,1,1,1,1,1,1,1,1,
1,1,1,1,1,1,1,4),(1.32416122177584E-7,0.015625,0.03125,0.0625,0.125,0.1875,
0.21875,0.25,0.28125,0.3125,0.375,0.5,0.625,0.6875,0.75,0.8125,0.875,1.),
 .UNSPECIFIED.);
#890=B_SPLINE_CURVE_WITH_KNOTS('',3,(#37886,#37887,#37888,#37889),
 .UNSPECIFIED.,.F.,.F.,(4,4),(-1.14630381292734,-1.04873232335616),
 .UNSPECIFIED.);
#891=B_SPLINE_CURVE_WITH_KNOTS('',3,(#37891,#37892,#37893,#37894,#37895,
#37896,#37897,#37898,#37899,#37900,#37901,#37902,#37903,#37904,#37905,#37906,
#37907,#37908),.UNSPECIFIED.,.F.,.F.,(4,1,1,1,1,1,1,1,1,1,1,1,1,1,1,4),
(0.,0.125,0.1875,0.25,0.3125,0.375,0.5,0.625,0.6875,0.71875,0.75,0.78125,
0.8125,0.875,0.9375,0.999999980241856),.UNSPECIFIED.);
#892=B_SPLINE_CURVE_WITH_KNOTS('',3,(#37910,#37911,#37912,#37913,#37914,
#37915,#37916,#37917,#37918,#37919,#37920,#37921,#37922,#37923,#37924,#37925,
#37926),.UNSPECIFIED.,.F.,.F.,(4,1,1,1,1,1,1,1,1,1,1,1,1,1,4),(2.27348631753915E-8,
0.125,0.1875,0.21875,0.25,0.28125,0.3125,0.375,0.5,0.625,0.6875,0.75,0.8125,
0.875,1.),.UNSPECIFIED.);
#893=B_SPLINE_CURVE_WITH_KNOTS('',3,(#37927,#37928,#37929,#37930),
 .UNSPECIFIED.,.F.,.F.,(4,4),(-1.13789426893553,-1.04477626914527),
 .UNSPECIFIED.);
#894=B_SPLINE_CURVE_WITH_KNOTS('',3,(#37934,#37935,#37936,#37937,#37938,
#37939,#37940,#37941,#37942,#37943,#37944,#37945,#37946,#37947,#37948,#37949,
#37950,#37951,#37952),.UNSPECIFIED.,.F.,.F.,(4,1,1,1,1,1,1,1,1,1,1,1,1,
1,1,1,4),(0.,0.125,0.1875,0.21875,0.25,0.28125,0.3125,0.375,0.5,0.625,0.6875,
0.71875,0.75,0.78125,0.8125,0.875,1.),.UNSPECIFIED.);
#895=B_SPLINE_CURVE_WITH_KNOTS('',3,(#37954,#37955,#37956,#37957,#37958,
#37959,#37960,#37961,#37962,#37963,#37964,#37965,#37966,#37967,#37968,#37969,
#37970,#37971,#37972,#37973),.UNSPECIFIED.,.F.,.F.,(4,1,1,1,1,1,1,1,1,1,
1,1,1,1,1,1,1,4),(2.05561699507991E-7,0.0625,0.125,0.1875,0.21875,0.25,
0.28125,0.3125,0.375,0.5,0.625,0.6875,0.71875,0.75,0.78125,0.8125,0.875,
1.),.UNSPECIFIED.);
#896=B_SPLINE_CURVE_WITH_KNOTS('',3,(#37975,#37976,#37977,#37978),
 .UNSPECIFIED.,.F.,.F.,(4,4),(-1.138991292616,-1.0479930898435),
 .UNSPECIFIED.);
#897=B_SPLINE_CURVE_WITH_KNOTS('',3,(#37980,#37981,#37982,#37983,#37984,
#37985,#37986,#37987,#37988,#37989,#37990,#37991,#37992,#37993,#37994,#37995,
#37996,#37997,#37998,#37999,#38000,#38001,#38002,#38003,#38004,#38005,#38006,
#38007,#38008,#38009,#38010,#38011,#38012,#38013,#38014,#38015,#38016,#38017,
#38018,#38019,#38020,#38021,#38022,#38023,#38024,#38025,#38026,#38027,#38028,
#38029,#38030,#38031),.UNSPECIFIED.,.F.,.F.,(4,3,3,3,3,3,3,3,3,3,3,3,3,
3,3,3,3,4),(0.,0.125,0.1875,0.21875,0.25,0.28125,0.3125,0.375,0.5,0.625,
0.6875,0.71875,0.75,0.78125,0.8125,0.875,0.9375,1.),.UNSPECIFIED.);
#898=B_SPLINE_CURVE_WITH_KNOTS('',3,(#38033,#38034,#38035,#38036,#38037,
#38038,#38039,#38040,#38041,#38042,#38043,#38044,#38045,#38046,#38047,#38048,
#38049,#38050,#38051,#38052,#38053,#38054,#38055,#38056,#38057,#38058,#38059,
#38060,#38061,#38062,#38063,#38064,#38065,#38066,#38067,#38068,#38069,#38070,
#38071,#38072,#38073,#38074,#38075,#38076,#38077,#38078,#38079,#38080,#38081),
 .UNSPECIFIED.,.F.,.F.,(4,3,3,3,3,3,3,3,3,3,3,3,3,3,3,3,4),(0.,0.125,0.1875,
0.21875,0.25,0.28125,0.3125,0.375,0.5,0.625,0.6875,0.71875,0.75,0.78125,
0.8125,0.875,1.),.UNSPECIFIED.);
#899=B_SPLINE_CURVE_WITH_KNOTS('',3,(#38082,#38083,#38084,#38085),
 .UNSPECIFIED.,.F.,.F.,(4,4),(-1.15404648390436,-1.06229819758988),
 .UNSPECIFIED.);
#900=B_SPLINE_CURVE_WITH_KNOTS('',3,(#38089,#38090,#38091,#38092,#38093,
#38094,#38095,#38096,#38097,#38098,#38099,#38100,#38101,#38102,#38103,#38104,
#38105,#38106),.UNSPECIFIED.,.F.,.F.,(4,1,1,1,1,1,1,1,1,1,1,1,1,1,1,4),
(0.,0.125,0.1875,0.25,0.3125,0.375,0.4375,0.5,0.625,0.6875,0.71875,0.75,
0.78125,0.8125,0.875,1.),.UNSPECIFIED.);
#901=B_SPLINE_CURVE_WITH_KNOTS('',3,(#38108,#38109,#38110,#38111,#38112,
#38113,#38114,#38115,#38116,#38117,#38118,#38119,#38120,#38121,#38122,#38123,
#38124,#38125,#38126,#38127),.UNSPECIFIED.,.F.,.F.,(4,1,1,1,1,1,1,1,1,1,
1,1,1,1,1,1,1,4),(2.17724807565861E-7,0.03125,0.0625,0.125,0.1875,0.21875,
0.25,0.28125,0.3125,0.375,0.5,0.5625,0.625,0.6875,0.75,0.8125,0.875,0.999999262331069),
 .UNSPECIFIED.);
#902=B_SPLINE_CURVE_WITH_KNOTS('',3,(#38129,#38130,#38131,#38132),
 .UNSPECIFIED.,.F.,.F.,(4,4),(-1.14332564091168,-1.05240155346319),
 .UNSPECIFIED.);
#903=B_SPLINE_CURVE_WITH_KNOTS('',3,(#38134,#38135,#38136,#38137,#38138,
#38139,#38140,#38141,#38142,#38143,#38144,#38145,#38146,#38147,#38148,#38149,
#38150,#38151,#38152,#38153),.UNSPECIFIED.,.F.,.F.,(4,1,1,1,1,1,1,1,1,1,
1,1,1,1,1,1,1,4),(0.,0.125,0.1875,0.25,0.3125,0.375,0.4375,0.5,0.625,0.6875,
0.71875,0.75,0.78125,0.8125,0.875,0.9375,0.96875,0.999999826165719),
 .UNSPECIFIED.);
#904=B_SPLINE_CURVE_WITH_KNOTS('',3,(#38155,#38156,#38157,#38158,#38159,
#38160,#38161,#38162,#38163,#38164,#38165,#38166,#38167,#38168,#38169,#38170,
#38171,#38172),.UNSPECIFIED.,.F.,.F.,(4,1,1,1,1,1,1,1,1,1,1,1,1,1,1,4),
(0.,0.125,0.1875,0.21875,0.25,0.28125,0.3125,0.375,0.5,0.5625,0.625,0.6875,
0.75,0.8125,0.875,1.),.UNSPECIFIED.);
#905=B_SPLINE_CURVE_WITH_KNOTS('',3,(#38173,#38174,#38175,#38176),
 .UNSPECIFIED.,.F.,.F.,(4,4),(-1.168912721115,-1.07795603507789),
 .UNSPECIFIED.);
#906=B_SPLINE_CURVE_WITH_KNOTS('',3,(#38180,#38181,#38182,#38183,#38184,
#38185,#38186,#38187,#38188,#38189,#38190,#38191,#38192,#38193,#38194,#38195,
#38196,#38197,#38198),.UNSPECIFIED.,.F.,.F.,(4,1,1,1,1,1,1,1,1,1,1,1,1,
1,1,1,4),(0.,0.125,0.1875,0.21875,0.25,0.28125,0.3125,0.375,0.5,0.625,0.6875,
0.71875,0.75,0.78125,0.8125,0.875,1.),.UNSPECIFIED.);
#907=B_SPLINE_CURVE_WITH_KNOTS('',3,(#38200,#38201,#38202,#38203,#38204,
#38205,#38206,#38207,#38208,#38209,#38210,#38211,#38212,#38213,#38214,#38215,
#38216,#38217,#38218,#38219,#38220,#38221,#38222,#38223),.UNSPECIFIED.,
 .F.,.F.,(4,1,1,1,1,1,1,1,1,1,1,1,1,1,1,1,1,1,1,1,1,4),(1.6543685732775E-6,
0.0078125,0.015625,0.03125,0.0625,0.09375,0.125,0.1875,0.21875,0.25,0.28125,
0.3125,0.375,0.5,0.625,0.6875,0.71875,0.75,0.78125,0.8125,0.875,1.),
 .UNSPECIFIED.);
#908=B_SPLINE_CURVE_WITH_KNOTS('',3,(#38225,#38226,#38227,#38228),
 .UNSPECIFIED.,.F.,.F.,(4,4),(-1.1365411740379,-1.04546711889777),
 .UNSPECIFIED.);
#909=B_SPLINE_CURVE_WITH_KNOTS('',3,(#38230,#38231,#38232,#38233,#38234,
#38235,#38236,#38237,#38238,#38239,#38240,#38241,#38242,#38243,#38244,#38245,
#38246,#38247,#38248,#38249,#38250,#38251,#38252,#38253,#38254,#38255,#38256,
#38257,#38258,#38259,#38260,#38261,#38262,#38263,#38264,#38265,#38266,#38267,
#38268,#38269,#38270,#38271,#38272,#38273,#38274,#38275,#38276,#38277,#38278),
 .UNSPECIFIED.,.F.,.F.,(4,3,3,3,3,3,3,3,3,3,3,3,3,3,3,3,4),(0.,0.125,0.1875,
0.21875,0.25,0.28125,0.3125,0.375,0.5,0.625,0.6875,0.71875,0.75,0.78125,
0.8125,0.875,1.),.UNSPECIFIED.);
#910=B_SPLINE_CURVE_WITH_KNOTS('',3,(#38280,#38281,#38282,#38283,#38284,
#38285,#38286,#38287,#38288,#38289,#38290,#38291,#38292,#38293,#38294,#38295,
#38296,#38297,#38298,#38299,#38300,#38301,#38302,#38303,#38304,#38305,#38306,
#38307,#38308,#38309,#38310,#38311,#38312,#38313,#38314,#38315,#38316,#38317,
#38318,#38319,#38320,#38321,#38322,#38323,#38324,#38325,#38326,#38327,#38328),
 .UNSPECIFIED.,.F.,.F.,(4,3,3,3,3,3,3,3,3,3,3,3,3,3,3,3,4),(0.,0.125,0.1875,
0.21875,0.25,0.28125,0.3125,0.375,0.5,0.625,0.6875,0.71875,0.75,0.78125,
0.8125,0.875,1.),.UNSPECIFIED.);
#911=B_SPLINE_CURVE_WITH_KNOTS('',3,(#38329,#38330,#38331,#38332),
 .UNSPECIFIED.,.F.,.F.,(4,4),(-1.14644022259357,-1.05547256732452),
 .UNSPECIFIED.);
#912=B_SPLINE_CURVE_WITH_KNOTS('',3,(#38336,#38337,#38338,#38339,#38340,
#38341,#38342,#38343,#38344,#38345,#38346,#38347,#38348,#38349,#38350,#38351,
#38352),.UNSPECIFIED.,.F.,.F.,(4,1,1,1,1,1,1,1,1,1,1,1,1,1,4),(0.,0.125,
0.1875,0.25,0.3125,0.375,0.5,0.625,0.6875,0.71875,0.75,0.78125,0.8125,0.875,
1.),.UNSPECIFIED.);
#913=B_SPLINE_CURVE_WITH_KNOTS('',3,(#38354,#38355,#38356,#38357,#38358,
#38359,#38360,#38361,#38362,#38363,#38364,#38365,#38366,#38367,#38368,#38369,
#38370,#38371,#38372,#38373),.UNSPECIFIED.,.F.,.F.,(4,1,1,1,1,1,1,1,1,1,
1,1,1,1,1,1,1,4),(7.22897047608602E-8,0.015625,0.03125,0.0625,0.125,0.1875,
0.21875,0.25,0.28125,0.3125,0.375,0.5,0.625,0.6875,0.75,0.8125,0.875,1.),
 .UNSPECIFIED.);
#914=B_SPLINE_CURVE_WITH_KNOTS('',3,(#38375,#38376,#38377,#38378),
 .UNSPECIFIED.,.F.,.F.,(4,4),(-1.14915858321821,-1.05511789649031),
 .UNSPECIFIED.);
#915=B_SPLINE_CURVE_WITH_KNOTS('',3,(#38380,#38381,#38382,#38383,#38384,
#38385,#38386,#38387,#38388,#38389,#38390,#38391,#38392,#38393,#38394,#38395,
#38396,#38397,#38398),.UNSPECIFIED.,.F.,.F.,(4,1,1,1,1,1,1,1,1,1,1,1,1,
1,1,1,4),(0.,0.125,0.1875,0.25,0.3125,0.375,0.5,0.625,0.6875,0.71875,0.75,
0.78125,0.8125,0.875,0.9375,0.96875,0.999999982337592),.UNSPECIFIED.);
#916=B_SPLINE_CURVE_WITH_KNOTS('',3,(#38400,#38401,#38402,#38403,#38404,
#38405,#38406,#38407,#38408,#38409,#38410,#38411,#38412,#38413,#38414,#38415,
#38416),.UNSPECIFIED.,.F.,.F.,(4,1,1,1,1,1,1,1,1,1,1,1,1,1,4),(1.83406697454463E-8,
0.125,0.1875,0.21875,0.25,0.28125,0.3125,0.375,0.5,0.625,0.6875,0.75,0.8125,
0.875,1.),.UNSPECIFIED.);
#917=B_SPLINE_CURVE_WITH_KNOTS('',3,(#38417,#38418,#38419,#38420),
 .UNSPECIFIED.,.F.,.F.,(4,4),(-1.14293348037966,-1.05189856760605),
 .UNSPECIFIED.);
#918=B_SPLINE_CURVE_WITH_KNOTS('',3,(#38424,#38425,#38426,#38427,#38428,
#38429,#38430,#38431,#38432,#38433,#38434,#38435,#38436,#38437,#38438,#38439,
#38440),.UNSPECIFIED.,.F.,.F.,(4,1,1,1,1,1,1,1,1,1,1,1,1,1,4),(0.,0.125,
0.1875,0.25,0.3125,0.375,0.5,0.625,0.6875,0.71875,0.75,0.78125,0.8125,0.875,
1.),.UNSPECIFIED.);
#919=B_SPLINE_CURVE_WITH_KNOTS('',3,(#38442,#38443,#38444,#38445,#38446,
#38447,#38448,#38449,#38450,#38451,#38452,#38453,#38454,#38455,#38456,#38457,
#38458,#38459,#38460),.UNSPECIFIED.,.F.,.F.,(4,1,1,1,1,1,1,1,1,1,1,1,1,
1,1,1,4),(4.59429913662085E-8,0.03125,0.0625,0.125,0.1875,0.21875,0.25,
0.28125,0.3125,0.375,0.5,0.625,0.6875,0.75,0.8125,0.875,1.),
 .UNSPECIFIED.);
#920=B_SPLINE_CURVE_WITH_KNOTS('',3,(#38462,#38463,#38464,#38465),
 .UNSPECIFIED.,.F.,.F.,(4,4),(-1.1400229377893,-1.04896134555146),
 .UNSPECIFIED.);
#921=B_SPLINE_CURVE_WITH_KNOTS('',3,(#38467,#38468,#38469,#38470,#38471,
#38472,#38473,#38474,#38475,#38476,#38477,#38478,#38479,#38480,#38481,#38482,
#38483,#38484),.UNSPECIFIED.,.F.,.F.,(4,1,1,1,1,1,1,1,1,1,1,1,1,1,1,4),
(0.,0.125,0.1875,0.25,0.3125,0.375,0.5,0.625,0.6875,0.71875,0.75,0.78125,
0.8125,0.875,0.9375,0.999999974036836),.UNSPECIFIED.);
#922=B_SPLINE_CURVE_WITH_KNOTS('',3,(#38486,#38487,#38488,#38489,#38490,
#38491,#38492,#38493,#38494,#38495,#38496,#38497,#38498,#38499,#38500,#38501,
#38502),.UNSPECIFIED.,.F.,.F.,(4,1,1,1,1,1,1,1,1,1,1,1,1,1,4),(1.69179276891372E-8,
0.125,0.1875,0.21875,0.25,0.28125,0.3125,0.375,0.5,0.625,0.6875,0.75,0.8125,
0.875,1.),.UNSPECIFIED.);
#923=B_SPLINE_CURVE_WITH_KNOTS('',3,(#38503,#38504,#38505,#38506),
 .UNSPECIFIED.,.F.,.F.,(4,4),(-1.14119404467057,-1.05000176302202),
 .UNSPECIFIED.);
#924=B_SPLINE_CURVE_WITH_KNOTS('',3,(#38510,#38511,#38512,#38513,#38514,
#38515,#38516,#38517,#38518,#38519,#38520,#38521,#38522,#38523,#38524,#38525,
#38526),.UNSPECIFIED.,.F.,.F.,(4,1,1,1,1,1,1,1,1,1,1,1,1,1,4),(0.,0.125,
0.1875,0.25,0.3125,0.375,0.5,0.625,0.6875,0.71875,0.75,0.78125,0.8125,0.875,
0.9999999591332),.UNSPECIFIED.);
#925=B_SPLINE_CURVE_WITH_KNOTS('',3,(#38528,#38529,#38530,#38531,#38532,
#38533,#38534,#38535,#38536,#38537,#38538,#38539,#38540,#38541,#38542,#38543,
#38544,#38545,#38546,#38547),.UNSPECIFIED.,.F.,.F.,(4,1,1,1,1,1,1,1,1,1,
1,1,1,1,1,1,1,4),(0.,0.015625,0.03125,0.0625,0.125,0.1875,0.21875,0.25,
0.28125,0.3125,0.375,0.5,0.625,0.6875,0.75,0.8125,0.875,1.),
 .UNSPECIFIED.);
#926=B_SPLINE_CURVE_WITH_KNOTS('',3,(#38549,#38550,#38551,#38552),
 .UNSPECIFIED.,.F.,.F.,(4,4),(-1.14875038807723,-1.05593562205532),
 .UNSPECIFIED.);
#927=B_SPLINE_CURVE_WITH_KNOTS('',3,(#38554,#38555,#38556,#38557,#38558,
#38559,#38560,#38561,#38562,#38563,#38564,#38565,#38566,#38567,#38568,#38569,
#38570,#38571,#38572),.UNSPECIFIED.,.F.,.F.,(4,1,1,1,1,1,1,1,1,1,1,1,1,
1,1,1,4),(0.,0.125,0.1875,0.25,0.3125,0.375,0.5,0.625,0.6875,0.71875,0.75,
0.78125,0.8125,0.875,0.9375,0.96875,0.999999969096218),.UNSPECIFIED.);
#928=B_SPLINE_CURVE_WITH_KNOTS('',3,(#38574,#38575,#38576,#38577,#38578,
#38579,#38580,#38581,#38582,#38583,#38584,#38585,#38586,#38587,#38588,#38589,
#38590),.UNSPECIFIED.,.F.,.F.,(4,1,1,1,1,1,1,1,1,1,1,1,1,1,4),(1.69694494032564E-8,
0.125,0.1875,0.21875,0.25,0.28125,0.3125,0.375,0.5,0.625,0.6875,0.75,0.8125,
0.875,1.),.UNSPECIFIED.);
#929=B_SPLINE_CURVE_WITH_KNOTS('',3,(#38591,#38592,#38593,#38594),
 .UNSPECIFIED.,.F.,.F.,(4,4),(-1.14085663885015,-1.04963197175557),
 .UNSPECIFIED.);
#930=B_SPLINE_CURVE_WITH_KNOTS('',3,(#38598,#38599,#38600,#38601,#38602,
#38603,#38604,#38605,#38606,#38607,#38608,#38609,#38610,#38611,#38612,#38613,
#38614),.UNSPECIFIED.,.F.,.F.,(4,1,1,1,1,1,1,1,1,1,1,1,1,1,4),(0.,0.125,
0.1875,0.25,0.3125,0.375,0.5,0.625,0.6875,0.71875,0.75,0.78125,0.8125,0.875,
0.999999967427316),.UNSPECIFIED.);
#931=B_SPLINE_CURVE_WITH_KNOTS('',3,(#38616,#38617,#38618,#38619,#38620,
#38621,#38622,#38623,#38624,#38625,#38626,#38627,#38628,#38629,#38630,#38631,
#38632,#38633,#38634,#38635),.UNSPECIFIED.,.F.,.F.,(4,1,1,1,1,1,1,1,1,1,
1,1,1,1,1,1,1,4),(0.,0.015625,0.03125,0.0625,0.125,0.1875,0.21875,0.25,
0.28125,0.3125,0.375,0.5,0.625,0.6875,0.75,0.8125,0.875,1.),
 .UNSPECIFIED.);
#932=B_SPLINE_CURVE_WITH_KNOTS('',3,(#38637,#38638,#38639,#38640),
 .UNSPECIFIED.,.F.,.F.,(4,4),(-1.14024200034905,-1.04934844889581),
 .UNSPECIFIED.);
#933=B_SPLINE_CURVE_WITH_KNOTS('',3,(#38642,#38643,#38644,#38645,#38646,
#38647,#38648,#38649,#38650,#38651,#38652,#38653,#38654,#38655,#38656,#38657,
#38658,#38659),.UNSPECIFIED.,.F.,.F.,(4,1,1,1,1,1,1,1,1,1,1,1,1,1,1,4),
(0.,0.125,0.1875,0.25,0.3125,0.375,0.5,0.625,0.6875,0.71875,0.75,0.78125,
0.8125,0.875,0.9375,0.99999998105284),.UNSPECIFIED.);
#934=B_SPLINE_CURVE_WITH_KNOTS('',3,(#38661,#38662,#38663,#38664,#38665,
#38666,#38667,#38668,#38669,#38670,#38671,#38672,#38673,#38674,#38675,#38676,
#38677),.UNSPECIFIED.,.F.,.F.,(4,1,1,1,1,1,1,1,1,1,1,1,1,1,4),(2.32949966596595E-8,
0.125,0.1875,0.21875,0.25,0.28125,0.3125,0.375,0.5,0.625,0.6875,0.75,0.8125,
0.875,1.),.UNSPECIFIED.);
#935=B_SPLINE_CURVE_WITH_KNOTS('',3,(#38678,#38679,#38680,#38681),
 .UNSPECIFIED.,.F.,.F.,(4,4),(-1.15396147913084,-1.0581629542817),
 .UNSPECIFIED.);
#936=B_SPLINE_CURVE_WITH_KNOTS('',3,(#38685,#38686,#38687,#38688,#38689,
#38690,#38691,#38692,#38693,#38694,#38695,#38696,#38697,#38698,#38699,#38700,
#38701,#38702),.UNSPECIFIED.,.F.,.F.,(4,1,1,1,1,1,1,1,1,1,1,1,1,1,1,4),
(0.,0.125,0.1875,0.25,0.3125,0.375,0.4375,0.5,0.625,0.6875,0.71875,0.75,
0.78125,0.8125,0.875,1.),.UNSPECIFIED.);
#937=B_SPLINE_CURVE_WITH_KNOTS('',3,(#38704,#38705,#38706,#38707,#38708,
#38709,#38710,#38711,#38712,#38713,#38714,#38715,#38716,#38717,#38718,#38719,
#38720,#38721,#38722,#38723,#38724),.UNSPECIFIED.,.F.,.F.,(4,1,1,1,1,1,
1,1,1,1,1,1,1,1,1,1,1,1,4),(1.76059286925808E-7,0.015625,0.03125,0.0625,
0.125,0.1875,0.21875,0.25,0.28125,0.3125,0.375,0.5,0.5625,0.625,0.6875,
0.75,0.8125,0.875,0.999999334182892),.UNSPECIFIED.);
#938=B_SPLINE_CURVE_WITH_KNOTS('',3,(#38726,#38727,#38728,#38729),
 .UNSPECIFIED.,.F.,.F.,(4,4),(-1.1418971753089,-1.05100194193717),
 .UNSPECIFIED.);
#939=B_SPLINE_CURVE_WITH_KNOTS('',3,(#38731,#38732,#38733,#38734,#38735,
#38736,#38737,#38738,#38739,#38740,#38741,#38742,#38743,#38744,#38745,#38746,
#38747,#38748,#38749,#38750,#38751),.UNSPECIFIED.,.F.,.F.,(4,1,1,1,1,1,
1,1,1,1,1,1,1,1,1,1,1,1,4),(0.,0.125,0.1875,0.25,0.3125,0.375,0.4375,0.5,
0.625,0.6875,0.71875,0.75,0.78125,0.8125,0.875,0.9375,0.96875,0.984375,
0.999999828518404),.UNSPECIFIED.);
#940=B_SPLINE_CURVE_WITH_KNOTS('',3,(#38753,#38754,#38755,#38756,#38757,
#38758,#38759,#38760,#38761,#38762,#38763,#38764,#38765,#38766,#38767,#38768,
#38769,#38770),.UNSPECIFIED.,.F.,.F.,(4,1,1,1,1,1,1,1,1,1,1,1,1,1,1,4),
(0.,0.125,0.1875,0.21875,0.25,0.28125,0.3125,0.375,0.5,0.5625,0.625,0.6875,
0.75,0.8125,0.875,1.),.UNSPECIFIED.);
#941=B_SPLINE_CURVE_WITH_KNOTS('',3,(#38771,#38772,#38773,#38774),
 .UNSPECIFIED.,.F.,.F.,(4,4),(-1.16831528067923,-1.07737821672828),
 .UNSPECIFIED.);
#942=B_SPLINE_CURVE_WITH_KNOTS('',3,(#38778,#38779,#38780,#38781,#38782,
#38783,#38784,#38785,#38786,#38787,#38788,#38789,#38790,#38791,#38792,#38793,
#38794),.UNSPECIFIED.,.F.,.F.,(4,1,1,1,1,1,1,1,1,1,1,1,1,1,4),(0.,0.125,
0.1875,0.25,0.3125,0.375,0.5,0.625,0.6875,0.71875,0.75,0.78125,0.8125,0.875,
1.),.UNSPECIFIED.);
#943=B_SPLINE_CURVE_WITH_KNOTS('',3,(#38796,#38797,#38798,#38799,#38800,
#38801,#38802,#38803,#38804,#38805,#38806,#38807,#38808,#38809,#38810,#38811,
#38812,#38813,#38814,#38815,#38816),.UNSPECIFIED.,.F.,.F.,(4,1,1,1,1,1,
1,1,1,1,1,1,1,1,1,1,1,1,4),(1.86298453241034E-7,0.015625,0.03125,0.0625,
0.125,0.1875,0.21875,0.25,0.28125,0.3125,0.375,0.5,0.5625,0.625,0.6875,
0.75,0.8125,0.875,0.999989495952636),.UNSPECIFIED.);
#944=B_SPLINE_CURVE_WITH_KNOTS('',3,(#38818,#38819,#38820,#38821,#38822,
#38823,#38824,#38825,#38826),.UNSPECIFIED.,.F.,.F.,(4,1,1,1,1,1,4),(4.64451719452503E-7,
0.25000034833879,0.375000290282325,0.50000023222586,0.625000174169395,0.75000011611293,
0.999999973113588),.UNSPECIFIED.);
#945=B_SPLINE_CURVE_WITH_KNOTS('',3,(#38828,#38829,#38830,#38831,#38832,
#38833,#38834,#38835,#38836,#38837,#38838,#38839,#38840,#38841,#38842,#38843,
#38844,#38845,#38846,#38847),.UNSPECIFIED.,.F.,.F.,(4,1,1,1,1,1,1,1,1,1,
1,1,1,1,1,1,1,4),(0.,0.125,0.1875,0.25,0.3125,0.375,0.4375,0.5,0.625,0.6875,
0.71875,0.75,0.78125,0.8125,0.875,0.9375,0.96875,0.999999724320717),
 .UNSPECIFIED.);
#946=B_SPLINE_CURVE_WITH_KNOTS('',3,(#38849,#38850,#38851,#38852,#38853,
#38854,#38855,#38856,#38857,#38858,#38859,#38860,#38861,#38862,#38863,#38864,
#38865,#38866),.UNSPECIFIED.,.F.,.F.,(4,1,1,1,1,1,1,1,1,1,1,1,1,1,1,4),
(0.,0.125,0.1875,0.21875,0.25,0.28125,0.3125,0.375,0.5,0.5625,0.625,0.6875,
0.75,0.8125,0.875,1.),.UNSPECIFIED.);
#947=B_SPLINE_CURVE_WITH_KNOTS('',3,(#38867,#38868,#38869,#38870,#38871,
#38872,#38873,#38874,#38875,#38876,#38877,#38878,#38879,#38880,#38881,#38882,
#38883,#38884,#38885,#38886,#38887,#38888,#38889,#38890,#38891),
 .UNSPECIFIED.,.F.,.F.,(4,3,3,3,3,3,3,3,4),(4.61042881515865E-6,0.181769987194646,
0.249999940419039,0.374999910628558,0.460304714091956,0.499999880838077,
0.624999851047596,0.749999821257116,0.999990442009691),.UNSPECIFIED.);
#948=B_SPLINE_CURVE_WITH_KNOTS('',3,(#38895,#38896,#38897,#38898,#38899,
#38900,#38901,#38902,#38903,#38904,#38905,#38906,#38907,#38908,#38909,#38910,
#38911),.UNSPECIFIED.,.F.,.F.,(4,1,1,1,1,1,1,1,1,1,1,1,1,1,4),(0.,0.125,
0.1875,0.25,0.3125,0.375,0.5,0.625,0.6875,0.71875,0.75,0.78125,0.8125,0.875,
0.99999998679207),.UNSPECIFIED.);
#949=B_SPLINE_CURVE_WITH_KNOTS('',3,(#38913,#38914,#38915,#38916,#38917,
#38918,#38919,#38920,#38921,#38922,#38923,#38924,#38925,#38926,#38927,#38928,
#38929,#38930),.UNSPECIFIED.,.F.,.F.,(4,1,1,1,1,1,1,1,1,1,1,1,1,1,1,4),
(8.65166934464853E-8,0.0625,0.125,0.1875,0.21875,0.25,0.28125,0.3125,0.375,
0.5,0.625,0.6875,0.75,0.8125,0.875,0.999868727025638),.UNSPECIFIED.);
#950=B_SPLINE_CURVE_WITH_KNOTS('',3,(#38932,#38933,#38934,#38935,#38936,
#38937,#38938,#38939,#38940,#38941,#38942,#38943,#38944,#38945,#38946,#38947,
#38948,#38949,#38950,#38951,#38952,#38953),.UNSPECIFIED.,.F.,.F.,(4,3,3,
3,3,3,3,4),(3.21388604215392E-7,0.250000241041453,0.375000200867878,0.500000160694302,
0.522785205722169,0.625000120520727,0.750000080347151,0.994571406786842),
 .UNSPECIFIED.);
#951=B_SPLINE_CURVE_WITH_KNOTS('',3,(#38955,#38956,#38957,#38958,#38959,
#38960,#38961,#38962),.UNSPECIFIED.,.F.,.F.,(4,2,2,4),(0.164816343944014,
0.188483278277886,0.274212380797636,0.359271548700789),.UNSPECIFIED.);
#952=B_SPLINE_CURVE_WITH_KNOTS('',3,(#38964,#38965,#38966,#38967,#38968,
#38969,#38970,#38971,#38972,#38973,#38974,#38975,#38976,#38977,#38978,#38979,
#38980),.UNSPECIFIED.,.F.,.F.,(4,1,1,1,1,1,1,1,1,1,1,1,1,1,4),(0.,0.125,
0.1875,0.21875,0.25,0.28125,0.3125,0.375,0.5,0.625,0.6875,0.75,0.8125,0.875,
0.999914460666039),.UNSPECIFIED.);
#953=B_SPLINE_CURVE_WITH_KNOTS('',3,(#38981,#38982,#38983,#38984,#38985,
#38986,#38987,#38988),.UNSPECIFIED.,.F.,.F.,(4,2,2,4),(0.000134614298568453,
0.0312571106388446,0.0597187154751761,0.108092813562148),.UNSPECIFIED.);
#954=B_SPLINE_CURVE_WITH_KNOTS('',3,(#38992,#38993,#38994,#38995,#38996,
#38997,#38998,#38999,#39000,#39001,#39002,#39003,#39004,#39005,#39006,#39007,
#39008),.UNSPECIFIED.,.F.,.F.,(4,1,1,1,1,1,1,1,1,1,1,1,1,1,4),(0.,0.125,
0.1875,0.25,0.3125,0.375,0.5,0.625,0.6875,0.71875,0.75,0.78125,0.8125,0.875,
1.),.UNSPECIFIED.);
#955=B_SPLINE_CURVE_WITH_KNOTS('',3,(#39010,#39011,#39012,#39013,#39014,
#39015,#39016,#39017,#39018,#39019,#39020,#39021,#39022,#39023,#39024,#39025,
#39026,#39027,#39028,#39029),.UNSPECIFIED.,.F.,.F.,(4,1,1,1,1,1,1,1,1,1,
1,1,1,1,1,1,1,4),(1.54060242968102E-7,0.015625,0.03125,0.0625,0.125,0.1875,
0.21875,0.25,0.28125,0.3125,0.375,0.5,0.625,0.6875,0.75,0.8125,0.875,1.),
 .UNSPECIFIED.);
#956=B_SPLINE_CURVE_WITH_KNOTS('',3,(#39031,#39032,#39033,#39034),
 .UNSPECIFIED.,.F.,.F.,(4,4),(8.88179596710341E-5,1.),.UNSPECIFIED.);
#957=B_SPLINE_CURVE_WITH_KNOTS('',3,(#39036,#39037,#39038,#39039,#39040,
#39041,#39042,#39043,#39044,#39045,#39046,#39047,#39048,#39049,#39050,#39051,
#39052),.UNSPECIFIED.,.F.,.F.,(4,1,1,1,1,1,1,1,1,1,1,1,1,1,4),(0.,0.125,
0.1875,0.25,0.3125,0.375,0.5,0.625,0.6875,0.71875,0.75,0.78125,0.8125,0.875,
0.999999976331826),.UNSPECIFIED.);
#958=B_SPLINE_CURVE_WITH_KNOTS('',3,(#39054,#39055,#39056,#39057,#39058,
#39059,#39060,#39061,#39062,#39063,#39064,#39065,#39066,#39067,#39068,#39069,
#39070),.UNSPECIFIED.,.F.,.F.,(4,1,1,1,1,1,1,1,1,1,1,1,1,1,4),(2.51851931900819E-8,
0.125,0.1875,0.21875,0.25,0.28125,0.3125,0.375,0.5,0.625,0.6875,0.75,0.8125,
0.875,1.),.UNSPECIFIED.);
#959=B_SPLINE_CURVE_WITH_KNOTS('',3,(#39071,#39072,#39073,#39074),
 .UNSPECIFIED.,.F.,.F.,(4,4),(0.,0.999911764093188),.UNSPECIFIED.);
#960=B_SPLINE_CURVE_WITH_KNOTS('',3,(#39078,#39079,#39080,#39081,#39082,
#39083,#39084,#39085),.UNSPECIFIED.,.F.,.F.,(4,2,2,4),(0.194407098287881,
0.199210339160986,0.303119902588705,0.355842009022126),.UNSPECIFIED.);
#961=B_SPLINE_CURVE_WITH_KNOTS('',3,(#39087,#39088,#39089,#39090,#39091,
#39092,#39093,#39094,#39095,#39096,#39097,#39098,#39099,#39100,#39101,#39102,
#39103,#39104,#39105),.UNSPECIFIED.,.F.,.F.,(4,3,3,3,3,3,4),(0.00444962817548656,
0.25,0.375,0.5,0.625,0.75,0.999988823500867),.UNSPECIFIED.);
#962=B_SPLINE_CURVE_WITH_KNOTS('',3,(#39107,#39108,#39109,#39110,#39111,
#39112,#39113,#39114),.UNSPECIFIED.,.F.,.F.,(4,2,2,4),(0.77443684568303,
0.777443693348876,0.895320737726667,0.914820143068275),.UNSPECIFIED.);
#963=B_SPLINE_CURVE_WITH_KNOTS('',3,(#39116,#39117,#39118,#39119,#39120,
#39121),.UNSPECIFIED.,.F.,.F.,(4,2,4),(0.586399068895315,0.598734783294216,
0.63797926634324),.UNSPECIFIED.);
#964=B_SPLINE_CURVE_WITH_KNOTS('',3,(#39123,#39124,#39125,#39126,#39127,
#39128,#39129,#39130,#39131,#39132,#39133,#39134,#39135,#39136,#39137,#39138,
#39139,#39140,#39141),.UNSPECIFIED.,.F.,.F.,(4,3,3,3,3,3,4),(3.45882434345197E-9,
0.25,0.375,0.5,0.625,0.75,1.),.UNSPECIFIED.);
#965=B_SPLINE_CURVE_WITH_KNOTS('',3,(#39142,#39143,#39144,#39145,#39146,
#39147,#39148,#39149,#39150,#39151,#39152,#39153,#39154,#39155,#39156,#39157,
#39158,#39159,#39160,#39161),.UNSPECIFIED.,.F.,.F.,(4,1,1,1,1,1,1,1,1,1,
1,1,1,1,1,1,1,4),(0.,0.125,0.1875,0.25,0.3125,0.375,0.5,0.625,0.6875,0.71875,
0.75,0.78125,0.8125,0.875,0.9375,0.96875,0.984375,0.999999989997333),
 .UNSPECIFIED.);
#966=B_SPLINE_CURVE_WITH_KNOTS('',3,(#39163,#39164,#39165,#39166),
 .UNSPECIFIED.,.F.,.F.,(4,4),(-0.0665009223849787,-0.0568933364251996),
 .UNSPECIFIED.);
#967=B_SPLINE_CURVE_WITH_KNOTS('',3,(#39167,#39168,#39169,#39170),
 .UNSPECIFIED.,.F.,.F.,(4,4),(-10.5474701151172,-10.5382467411489),
 .UNSPECIFIED.);
#968=B_SPLINE_CURVE_WITH_KNOTS('',3,(#39175,#39176,#39177,#39178,#39179,
#39180,#39181,#39182,#39183,#39184,#39185,#39186,#39187,#39188,#39189,#39190,
#39191),.UNSPECIFIED.,.F.,.F.,(4,1,1,1,1,1,1,1,1,1,1,1,1,1,4),(0.,0.125,
0.1875,0.25,0.3125,0.375,0.5,0.625,0.6875,0.71875,0.75,0.78125,0.8125,0.875,
1.),.UNSPECIFIED.);
#969=B_SPLINE_CURVE_WITH_KNOTS('',3,(#39193,#39194,#39195,#39196,#39197,
#39198,#39199,#39200),.UNSPECIFIED.,.F.,.F.,(4,2,2,4),(0.723946350565727,
0.748538685805071,0.816066681444924,0.827939780191109),.UNSPECIFIED.);
#970=B_SPLINE_CURVE_WITH_KNOTS('',3,(#39202,#39203,#39204,#39205),
 .UNSPECIFIED.,.F.,.F.,(4,4),(-1.14947842120138,-1.05363271233087),
 .UNSPECIFIED.);
#971=B_SPLINE_CURVE_WITH_KNOTS('',3,(#39207,#39208,#39209,#39210,#39211,
#39212,#39213,#39214,#39215,#39216,#39217,#39218,#39219,#39220,#39221,#39222,
#39223),.UNSPECIFIED.,.F.,.F.,(4,1,1,1,1,1,1,1,1,1,1,1,1,1,4),(0.,0.125,
0.1875,0.25,0.3125,0.375,0.5,0.625,0.6875,0.71875,0.75,0.78125,0.8125,0.875,
0.999999992783616),.UNSPECIFIED.);
#972=B_SPLINE_CURVE_WITH_KNOTS('',3,(#39225,#39226,#39227,#39228,#39229,
#39230,#39231,#39232,#39233,#39234,#39235,#39236,#39237,#39238,#39239,#39240,
#39241),.UNSPECIFIED.,.F.,.F.,(4,1,1,1,1,1,1,1,1,1,1,1,1,1,4),(4.61532930101729E-9,
0.125,0.1875,0.21875,0.25,0.28125,0.3125,0.375,0.5,0.625,0.6875,0.75,0.8125,
0.875,1.),.UNSPECIFIED.);
#973=B_SPLINE_CURVE_WITH_KNOTS('',3,(#39242,#39243,#39244,#39245),
 .UNSPECIFIED.,.F.,.F.,(4,4),(-1.1486920679677,-1.05773319824162),
 .UNSPECIFIED.);
#974=B_SPLINE_CURVE_WITH_KNOTS('',3,(#39249,#39250,#39251,#39252,#39253,
#39254,#39255,#39256,#39257,#39258,#39259,#39260,#39261,#39262,#39263,#39264,
#39265),.UNSPECIFIED.,.F.,.F.,(4,1,1,1,1,1,1,1,1,1,1,1,1,1,4),(0.,0.125,
0.1875,0.25,0.3125,0.375,0.5,0.625,0.6875,0.71875,0.75,0.78125,0.8125,0.875,
0.999999986938439),.UNSPECIFIED.);
#975=B_SPLINE_CURVE_WITH_KNOTS('',3,(#39267,#39268,#39269,#39270,#39271,
#39272,#39273,#39274,#39275,#39276,#39277,#39278,#39279,#39280,#39281,#39282,
#39283,#39284,#39285),.UNSPECIFIED.,.F.,.F.,(4,1,1,1,1,1,1,1,1,1,1,1,1,
1,1,1,4),(9.72661732996662E-8,0.125,0.1875,0.21875,0.25,0.28125,0.3125,
0.375,0.5,0.625,0.6875,0.71875,0.75,0.78125,0.8125,0.875,1.),
 .UNSPECIFIED.);
#976=B_SPLINE_CURVE_WITH_KNOTS('',3,(#39287,#39288,#39289,#39290),
 .UNSPECIFIED.,.F.,.F.,(4,4),(-1.13349992980958,-1.03925436083094),
 .UNSPECIFIED.);
#977=B_SPLINE_CURVE_WITH_KNOTS('',3,(#39292,#39293,#39294,#39295,#39296,
#39297,#39298,#39299,#39300,#39301,#39302,#39303,#39304,#39305,#39306,#39307,
#39308,#39309,#39310),.UNSPECIFIED.,.F.,.F.,(4,1,1,1,1,1,1,1,1,1,1,1,1,
1,1,1,4),(0.,0.125,0.1875,0.21875,0.25,0.28125,0.3125,0.375,0.5,0.625,0.6875,
0.71875,0.75,0.78125,0.8125,0.875,1.),.UNSPECIFIED.);
#978=B_SPLINE_CURVE_WITH_KNOTS('',3,(#39312,#39313,#39314,#39315,#39316,
#39317,#39318,#39319,#39320,#39321,#39322,#39323,#39324,#39325,#39326,#39327,
#39328),.UNSPECIFIED.,.F.,.F.,(4,1,1,1,1,1,1,1,1,1,1,1,1,1,4),(0.,0.125,
0.1875,0.21875,0.25,0.28125,0.3125,0.375,0.5,0.625,0.6875,0.75,0.8125,0.875,
1.),.UNSPECIFIED.);
#979=B_SPLINE_CURVE_WITH_KNOTS('',3,(#39329,#39330,#39331,#39332),
 .UNSPECIFIED.,.F.,.F.,(4,4),(-1.14030765698104,-1.04891270929124),
 .UNSPECIFIED.);
#980=B_SPLINE_CURVE_WITH_KNOTS('',3,(#39336,#39337,#39338,#39339,#39340,
#39341,#39342,#39343,#39344,#39345,#39346,#39347,#39348,#39349,#39350,#39351,
#39352,#39353,#39354,#39355,#39356,#39357,#39358,#39359,#39360,#39361,#39362,
#39363,#39364,#39365,#39366,#39367,#39368,#39369,#39370,#39371,#39372,#39373,
#39374,#39375,#39376,#39377,#39378,#39379,#39380,#39381,#39382,#39383,#39384),
 .UNSPECIFIED.,.F.,.F.,(4,3,3,3,3,3,3,3,3,3,3,3,3,3,3,3,4),(2.55001903434036E-14,
0.125,0.1875,0.21875,0.25,0.28125,0.3125,0.375,0.5,0.625,0.6875,0.71875,
0.75,0.78125,0.8125,0.875,0.999999987092966),.UNSPECIFIED.);
#981=B_SPLINE_CURVE_WITH_KNOTS('',3,(#39386,#39387,#39388,#39389,#39390,
#39391,#39392,#39393,#39394,#39395,#39396,#39397,#39398,#39399,#39400,#39401,
#39402,#39403,#39404),.UNSPECIFIED.,.F.,.F.,(4,1,1,1,1,1,1,1,1,1,1,1,1,
1,1,1,4),(1.12071241714957E-7,0.125,0.1875,0.21875,0.25,0.28125,0.3125,
0.375,0.5,0.625,0.6875,0.71875,0.75,0.78125,0.8125,0.875,1.),
 .UNSPECIFIED.);
#982=B_SPLINE_CURVE_WITH_KNOTS('',3,(#39406,#39407,#39408,#39409),
 .UNSPECIFIED.,.F.,.F.,(4,4),(-1.13407654678454,-1.03941382788935),
 .UNSPECIFIED.);
#983=B_SPLINE_CURVE_WITH_KNOTS('',3,(#39411,#39412,#39413,#39414,#39415,
#39416,#39417,#39418,#39419,#39420,#39421,#39422,#39423,#39424,#39425,#39426,
#39427,#39428,#39429,#39430,#39431,#39432,#39433,#39434,#39435,#39436,#39437,
#39438,#39439,#39440,#39441,#39442,#39443,#39444,#39445,#39446,#39447,#39448,
#39449,#39450,#39451,#39452,#39453,#39454,#39455,#39456,#39457,#39458,#39459),
 .UNSPECIFIED.,.F.,.F.,(4,3,3,3,3,3,3,3,3,3,3,3,3,3,3,3,4),(0.,0.125,0.1875,
0.21875,0.25,0.28125,0.3125,0.375,0.5,0.625,0.6875,0.71875,0.75,0.78125,
0.8125,0.875,1.),.UNSPECIFIED.);
#984=B_SPLINE_CURVE_WITH_KNOTS('',3,(#39461,#39462,#39463,#39464,#39465,
#39466,#39467,#39468,#39469,#39470,#39471,#39472,#39473,#39474,#39475,#39476,
#39477),.UNSPECIFIED.,.F.,.F.,(4,1,1,1,1,1,1,1,1,1,1,1,1,1,4),(0.,0.125,
0.1875,0.21875,0.25,0.28125,0.3125,0.375,0.5,0.625,0.6875,0.75,0.8125,0.875,
1.),.UNSPECIFIED.);
#985=B_SPLINE_CURVE_WITH_KNOTS('',3,(#39478,#39479,#39480,#39481),
 .UNSPECIFIED.,.F.,.F.,(4,4),(-1.13870206156022,-1.04613000297405),
 .UNSPECIFIED.);
#986=B_SPLINE_CURVE_WITH_KNOTS('',3,(#39485,#39486,#39487,#39488,#39489,
#39490,#39491,#39492,#39493,#39494,#39495,#39496,#39497,#39498,#39499,#39500,
#39501,#39502,#39503,#39504,#39505,#39506,#39507,#39508,#39509,#39510,#39511,
#39512,#39513,#39514,#39515,#39516,#39517,#39518,#39519,#39520,#39521,#39522,
#39523,#39524,#39525,#39526,#39527,#39528,#39529,#39530,#39531,#39532,#39533),
 .UNSPECIFIED.,.F.,.F.,(4,3,3,3,3,3,3,3,3,3,3,3,3,3,3,3,4),(5.88455490193989E-15,
0.125,0.1875,0.21875,0.25,0.28125,0.3125,0.375,0.5,0.625,0.6875,0.71875,
0.75,0.78125,0.8125,0.875,0.99999998726157),.UNSPECIFIED.);
#987=B_SPLINE_CURVE_WITH_KNOTS('',3,(#39535,#39536,#39537,#39538,#39539,
#39540,#39541,#39542,#39543,#39544,#39545,#39546,#39547,#39548,#39549,#39550,
#39551,#39552,#39553),.UNSPECIFIED.,.F.,.F.,(4,1,1,1,1,1,1,1,1,1,1,1,1,
1,1,1,4),(1.40925419990928E-7,0.125,0.1875,0.21875,0.25,0.28125,0.3125,
0.375,0.5,0.625,0.6875,0.71875,0.75,0.78125,0.8125,0.875,1.),
 .UNSPECIFIED.);
#988=B_SPLINE_CURVE_WITH_KNOTS('',3,(#39555,#39556,#39557,#39558),
 .UNSPECIFIED.,.F.,.F.,(4,4),(-1.13230492679919,-1.03947426144326),
 .UNSPECIFIED.);
#989=B_SPLINE_CURVE_WITH_KNOTS('',3,(#39560,#39561,#39562,#39563,#39564,
#39565,#39566,#39567,#39568,#39569,#39570,#39571,#39572,#39573,#39574,#39575,
#39576,#39577,#39578,#39579,#39580,#39581,#39582,#39583,#39584,#39585,#39586,
#39587,#39588,#39589,#39590,#39591,#39592,#39593,#39594,#39595,#39596,#39597,
#39598,#39599,#39600,#39601,#39602,#39603,#39604,#39605,#39606,#39607,#39608),
 .UNSPECIFIED.,.F.,.F.,(4,3,3,3,3,3,3,3,3,3,3,3,3,3,3,3,4),(0.,0.125,0.1875,
0.21875,0.25,0.28125,0.3125,0.375,0.5,0.625,0.6875,0.71875,0.75,0.78125,
0.8125,0.875,1.),.UNSPECIFIED.);
#990=B_SPLINE_CURVE_WITH_KNOTS('',3,(#39610,#39611,#39612,#39613,#39614,
#39615,#39616,#39617,#39618,#39619,#39620,#39621,#39622,#39623,#39624,#39625,
#39626,#39627,#39628,#39629,#39630,#39631,#39632,#39633,#39634,#39635,#39636,
#39637,#39638,#39639,#39640,#39641,#39642,#39643,#39644,#39645,#39646,#39647,
#39648,#39649,#39650,#39651,#39652,#39653,#39654,#39655,#39656,#39657,#39658),
 .UNSPECIFIED.,.F.,.F.,(4,3,3,3,3,3,3,3,3,3,3,3,3,3,3,3,4),(0.,0.125,0.1875,
0.21875,0.25,0.28125,0.3125,0.375,0.5,0.625,0.6875,0.71875,0.75,0.78125,
0.8125,0.875,1.),.UNSPECIFIED.);
#991=B_SPLINE_CURVE_WITH_KNOTS('',3,(#39659,#39660,#39661,#39662),
 .UNSPECIFIED.,.F.,.F.,(4,4),(-1.14623578895171,-1.0552604634692),
 .UNSPECIFIED.);
#992=B_SPLINE_CURVE_WITH_KNOTS('',3,(#39666,#39667,#39668,#39669,#39670,
#39671,#39672,#39673,#39674,#39675,#39676,#39677,#39678,#39679,#39680,#39681,
#39682),.UNSPECIFIED.,.F.,.F.,(4,1,1,1,1,1,1,1,1,1,1,1,1,1,4),(0.,0.125,
0.1875,0.25,0.3125,0.375,0.5,0.625,0.6875,0.71875,0.75,0.78125,0.8125,0.875,
1.),.UNSPECIFIED.);
#993=B_SPLINE_CURVE_WITH_KNOTS('',3,(#39684,#39685,#39686,#39687,#39688,
#39689,#39690,#39691,#39692,#39693,#39694,#39695,#39696,#39697,#39698,#39699,
#39700),.UNSPECIFIED.,.F.,.F.,(4,1,1,1,1,1,1,1,1,1,1,1,1,1,4),(8.0555447065195E-8,
0.125,0.1875,0.21875,0.25,0.28125,0.3125,0.375,0.5,0.625,0.6875,0.75,0.8125,
0.875,1.),.UNSPECIFIED.);
#994=B_SPLINE_CURVE_WITH_KNOTS('',3,(#39702,#39703,#39704,#39705,#39706,
#39707),.UNSPECIFIED.,.F.,.F.,(4,2,4),(-1.14515135463117,-1.06190814579394,
-1.04640883228602),.UNSPECIFIED.);
#995=B_SPLINE_CURVE_WITH_KNOTS('',3,(#39709,#39710,#39711,#39712,#39713,
#39714,#39715,#39716,#39717,#39718,#39719,#39720,#39721,#39722,#39723,#39724,
#39725),.UNSPECIFIED.,.F.,.F.,(4,1,1,1,1,1,1,1,1,1,1,1,1,1,4),(0.,0.125,
0.1875,0.25,0.3125,0.375,0.5,0.625,0.6875,0.71875,0.75,0.78125,0.8125,0.875,
0.999999978936368),.UNSPECIFIED.);
#996=B_SPLINE_CURVE_WITH_KNOTS('',3,(#39727,#39728,#39729,#39730,#39731,
#39732,#39733,#39734,#39735,#39736,#39737,#39738,#39739,#39740,#39741,#39742,
#39743),.UNSPECIFIED.,.F.,.F.,(4,1,1,1,1,1,1,1,1,1,1,1,1,1,4),(2.28361295605953E-8,
0.125,0.1875,0.21875,0.25,0.28125,0.3125,0.375,0.5,0.625,0.6875,0.75,0.8125,
0.875,1.),.UNSPECIFIED.);
#997=B_SPLINE_CURVE_WITH_KNOTS('',3,(#39744,#39745,#39746,#39747),
 .UNSPECIFIED.,.F.,.F.,(4,4),(-1.13911633111086,-1.04475206254057),
 .UNSPECIFIED.);
#998=B_SPLINE_CURVE_WITH_KNOTS('',3,(#39751,#39752,#39753,#39754,#39755,
#39756,#39757,#39758,#39759,#39760,#39761,#39762,#39763,#39764,#39765,#39766,
#39767,#39768,#39769),.UNSPECIFIED.,.F.,.F.,(4,1,1,1,1,1,1,1,1,1,1,1,1,
1,1,1,4),(0.,0.125,0.1875,0.21875,0.25,0.28125,0.3125,0.375,0.5,0.625,0.6875,
0.71875,0.75,0.78125,0.8125,0.875,0.999999987528574),.UNSPECIFIED.);
#999=B_SPLINE_CURVE_WITH_KNOTS('',3,(#39771,#39772,#39773,#39774,#39775,
#39776,#39777,#39778,#39779,#39780,#39781,#39782,#39783,#39784,#39785,#39786,
#39787,#39788,#39789),.UNSPECIFIED.,.F.,.F.,(4,1,1,1,1,1,1,1,1,1,1,1,1,
1,1,1,4),(1.7743161549064E-7,0.125,0.1875,0.21875,0.25,0.28125,0.3125,0.375,
0.5,0.625,0.6875,0.71875,0.75,0.78125,0.8125,0.875,1.),.UNSPECIFIED.);
#1000=B_SPLINE_CURVE_WITH_KNOTS('',3,(#39791,#39792,#39793,#39794),
 .UNSPECIFIED.,.F.,.F.,(4,4),(-1.13925469784202,-1.04825641978528),
 .UNSPECIFIED.);
#1001=B_SPLINE_CURVE_WITH_KNOTS('',3,(#39796,#39797,#39798,#39799,#39800,
#39801,#39802,#39803,#39804,#39805,#39806,#39807,#39808,#39809,#39810,#39811,
#39812,#39813,#39814,#39815,#39816,#39817,#39818,#39819,#39820,#39821,#39822,
#39823,#39824,#39825,#39826,#39827,#39828,#39829,#39830,#39831,#39832,#39833,
#39834,#39835,#39836,#39837,#39838,#39839,#39840,#39841,#39842,#39843,#39844),
 .UNSPECIFIED.,.F.,.F.,(4,3,3,3,3,3,3,3,3,3,3,3,3,3,3,3,4),(0.,0.125,0.1875,
0.21875,0.25,0.28125,0.3125,0.375,0.5,0.625,0.6875,0.71875,0.75,0.78125,
0.8125,0.875,1.),.UNSPECIFIED.);
#1002=B_SPLINE_CURVE_WITH_KNOTS('',3,(#39846,#39847,#39848,#39849,#39850,
#39851,#39852,#39853,#39854,#39855,#39856,#39857,#39858,#39859,#39860,#39861,
#39862,#39863,#39864,#39865,#39866,#39867,#39868,#39869,#39870,#39871,#39872,
#39873,#39874,#39875,#39876,#39877,#39878,#39879,#39880,#39881,#39882,#39883,
#39884,#39885,#39886,#39887,#39888,#39889,#39890,#39891,#39892,#39893,#39894),
 .UNSPECIFIED.,.F.,.F.,(4,3,3,3,3,3,3,3,3,3,3,3,3,3,3,3,4),(0.,0.125,0.1875,
0.21875,0.25,0.28125,0.3125,0.375,0.5,0.625,0.6875,0.71875,0.75,0.78125,
0.8125,0.875,1.),.UNSPECIFIED.);
#1003=B_SPLINE_CURVE_WITH_KNOTS('',3,(#39895,#39896,#39897,#39898),
 .UNSPECIFIED.,.F.,.F.,(4,4),(-1.15381330807476,-1.06213654023606),
 .UNSPECIFIED.);
#1004=B_SPLINE_CURVE_WITH_KNOTS('',3,(#39902,#39903,#39904,#39905,#39906,
#39907,#39908,#39909,#39910,#39911,#39912,#39913,#39914,#39915,#39916,#39917,
#39918,#39919),.UNSPECIFIED.,.F.,.F.,(4,1,1,1,1,1,1,1,1,1,1,1,1,1,1,4),
(0.,0.125,0.1875,0.25,0.3125,0.375,0.4375,0.5,0.625,0.6875,0.71875,0.75,
0.78125,0.8125,0.875,1.),.UNSPECIFIED.);
#1005=B_SPLINE_CURVE_WITH_KNOTS('',3,(#39921,#39922,#39923,#39924,#39925,
#39926,#39927,#39928,#39929,#39930,#39931,#39932,#39933,#39934,#39935,#39936,
#39937,#39938),.UNSPECIFIED.,.F.,.F.,(4,1,1,1,1,1,1,1,1,1,1,1,1,1,1,4),
(1.64962983094098E-7,0.125,0.1875,0.21875,0.25,0.28125,0.3125,0.375,0.5,
0.5625,0.625,0.6875,0.75,0.8125,0.875,0.999999279741807),.UNSPECIFIED.);
#1006=B_SPLINE_CURVE_WITH_KNOTS('',3,(#39940,#39941,#39942,#39943),
 .UNSPECIFIED.,.F.,.F.,(4,4),(-1.14333787758334,-1.05241548175551),
 .UNSPECIFIED.);
#1007=B_SPLINE_CURVE_WITH_KNOTS('',3,(#39945,#39946,#39947,#39948,#39949,
#39950,#39951,#39952,#39953,#39954,#39955,#39956,#39957,#39958,#39959,#39960,
#39961,#39962),.UNSPECIFIED.,.F.,.F.,(4,1,1,1,1,1,1,1,1,1,1,1,1,1,1,4),
(0.,0.125,0.1875,0.25,0.3125,0.375,0.4375,0.5,0.625,0.6875,0.71875,0.75,
0.78125,0.8125,0.875,0.999999803503463),.UNSPECIFIED.);
#1008=B_SPLINE_CURVE_WITH_KNOTS('',3,(#39964,#39965,#39966,#39967,#39968,
#39969,#39970,#39971,#39972,#39973,#39974,#39975,#39976,#39977,#39978,#39979,
#39980,#39981),.UNSPECIFIED.,.F.,.F.,(4,1,1,1,1,1,1,1,1,1,1,1,1,1,1,4),
(0.,0.125,0.1875,0.21875,0.25,0.28125,0.3125,0.375,0.5,0.5625,0.625,0.6875,
0.75,0.8125,0.875,1.),.UNSPECIFIED.);
#1009=B_SPLINE_CURVE_WITH_KNOTS('',3,(#39982,#39983,#39984,#39985),
 .UNSPECIFIED.,.F.,.F.,(4,4),(-1.16836067888312,-1.07743287791435),
 .UNSPECIFIED.);
#1010=B_SPLINE_CURVE_WITH_KNOTS('',3,(#39989,#39990,#39991,#39992,#39993,
#39994,#39995,#39996,#39997,#39998,#39999,#40000,#40001,#40002,#40003,#40004,
#40005,#40006,#40007),.UNSPECIFIED.,.F.,.F.,(4,1,1,1,1,1,1,1,1,1,1,1,1,
1,1,1,4),(0.,0.125,0.1875,0.21875,0.25,0.28125,0.3125,0.375,0.5,0.625,0.6875,
0.71875,0.75,0.78125,0.8125,0.875,1.),.UNSPECIFIED.);
#1011=B_SPLINE_CURVE_WITH_KNOTS('',3,(#40009,#40010,#40011,#40012,#40013,
#40014,#40015,#40016,#40017,#40018,#40019,#40020,#40021,#40022,#40023,#40024,
#40025,#40026,#40027),.UNSPECIFIED.,.F.,.F.,(4,1,1,1,1,1,1,1,1,1,1,1,1,
1,1,1,4),(1.71448431414438E-7,0.125,0.1875,0.21875,0.25,0.28125,0.3125,
0.375,0.5,0.625,0.6875,0.71875,0.75,0.78125,0.8125,0.875,1.),
 .UNSPECIFIED.);
#1012=B_SPLINE_CURVE_WITH_KNOTS('',3,(#40029,#40030,#40031,#40032),
 .UNSPECIFIED.,.F.,.F.,(4,4),(-1.13680001467877,-1.04572530935217),
 .UNSPECIFIED.);
#1013=B_SPLINE_CURVE_WITH_KNOTS('',3,(#40034,#40035,#40036,#40037,#40038,
#40039,#40040,#40041,#40042,#40043,#40044,#40045,#40046,#40047,#40048,#40049,
#40050,#40051,#40052,#40053,#40054,#40055,#40056,#40057,#40058,#40059,#40060,
#40061,#40062,#40063,#40064,#40065,#40066,#40067,#40068,#40069,#40070,#40071,
#40072,#40073,#40074,#40075,#40076,#40077,#40078,#40079,#40080,#40081,#40082),
 .UNSPECIFIED.,.F.,.F.,(4,3,3,3,3,3,3,3,3,3,3,3,3,3,3,3,4),(0.,0.125,0.1875,
0.21875,0.25,0.28125,0.3125,0.375,0.5,0.625,0.6875,0.71875,0.75,0.78125,
0.8125,0.875,1.),.UNSPECIFIED.);
#1014=B_SPLINE_CURVE_WITH_KNOTS('',3,(#40084,#40085,#40086,#40087,#40088,
#40089,#40090,#40091,#40092,#40093,#40094,#40095,#40096,#40097,#40098,#40099,
#40100,#40101,#40102,#40103,#40104,#40105,#40106,#40107,#40108,#40109,#40110,
#40111,#40112,#40113,#40114,#40115,#40116,#40117,#40118,#40119,#40120,#40121,
#40122,#40123,#40124,#40125,#40126,#40127,#40128,#40129,#40130,#40131,#40132),
 .UNSPECIFIED.,.F.,.F.,(4,3,3,3,3,3,3,3,3,3,3,3,3,3,3,3,4),(0.,0.125,0.1875,
0.21875,0.25,0.28125,0.3125,0.375,0.5,0.625,0.6875,0.71875,0.75,0.78125,
0.8125,0.875,1.),.UNSPECIFIED.);
#1015=B_SPLINE_CURVE_WITH_KNOTS('',3,(#40133,#40134,#40135,#40136),
 .UNSPECIFIED.,.F.,.F.,(4,4),(-1.14643591429736,-1.05546845872828),
 .UNSPECIFIED.);
#1016=B_SPLINE_CURVE_WITH_KNOTS('',3,(#40140,#40141,#40142,#40143,#40144,
#40145,#40146,#40147,#40148,#40149,#40150,#40151,#40152,#40153,#40154,#40155,
#40156),.UNSPECIFIED.,.F.,.F.,(4,1,1,1,1,1,1,1,1,1,1,1,1,1,4),(0.,0.125,
0.1875,0.25,0.3125,0.375,0.5,0.625,0.6875,0.71875,0.75,0.78125,0.8125,0.875,
0.999974157502117),.UNSPECIFIED.);
#1017=B_SPLINE_CURVE_WITH_KNOTS('',3,(#40158,#40159,#40160,#40161,#40162,
#40163,#40164,#40165,#40166,#40167,#40168,#40169,#40170,#40171,#40172,#40173,
#40174,#40175,#40176,#40177,#40178,#40179,#40180,#40181,#40182,#40183,#40184,
#40185,#40186,#40187,#40188,#40189,#40190,#40191,#40192,#40193,#40194,#40195,
#40196,#40197,#40198,#40199,#40200,#40201,#40202,#40203,#40204,#40205,#40206,
#40207),.UNSPECIFIED.,.F.,.F.,(4,2,2,2,2,2,2,2,2,2,2,2,2,2,2,2,2,2,2,2,
2,2,2,2,4),(2.4036706065768E-5,0.00977418865733799,0.0213000820686129,0.0228713448821847,
0.0245760487443449,0.028666855265285,0.0419488423804167,0.0819470875054392,
0.0874089326177544,0.116494431563777,0.155248703049381,0.176699028655761,
0.20033104560553,0.250819278402669,0.282215606032038,0.337127383171215,
0.420231565913135,0.422824375704096,0.427853052523601,0.465166977215536,
0.477606564650635,0.485039244387621,0.489575937579279,0.490429017673501,
0.503063262505017),.UNSPECIFIED.);
#1018=B_SPLINE_CURVE_WITH_KNOTS('',3,(#40209,#40210,#40211,#40212),
 .UNSPECIFIED.,.F.,.F.,(4,4),(-1.14946321606806,-1.05524237219014),
 .UNSPECIFIED.);
#1019=B_SPLINE_CURVE_WITH_KNOTS('',3,(#40214,#40215,#40216,#40217,#40218,
#40219,#40220,#40221,#40222,#40223,#40224,#40225,#40226,#40227,#40228,#40229,
#40230),.UNSPECIFIED.,.F.,.F.,(4,1,1,1,1,1,1,1,1,1,1,1,1,1,4),(0.,0.125,
0.1875,0.25,0.3125,0.375,0.5,0.625,0.6875,0.71875,0.75,0.78125,0.8125,0.875,
0.999999978619674),.UNSPECIFIED.);
#1020=B_SPLINE_CURVE_WITH_KNOTS('',3,(#40232,#40233,#40234,#40235,#40236,
#40237,#40238,#40239,#40240,#40241,#40242,#40243,#40244,#40245,#40246,#40247,
#40248),.UNSPECIFIED.,.F.,.F.,(4,1,1,1,1,1,1,1,1,1,1,1,1,1,4),(1.83706666942875E-8,
0.125,0.1875,0.21875,0.25,0.28125,0.3125,0.375,0.5,0.625,0.6875,0.75,0.8125,
0.875,1.),.UNSPECIFIED.);
#1021=B_SPLINE_CURVE_WITH_KNOTS('',3,(#40249,#40250,#40251,#40252),
 .UNSPECIFIED.,.F.,.F.,(4,4),(-1.14299247720633,-1.0519693017081),
 .UNSPECIFIED.);
#1022=B_SPLINE_CURVE_WITH_KNOTS('',3,(#40256,#40257,#40258,#40259,#40260,
#40261,#40262,#40263,#40264,#40265,#40266,#40267,#40268,#40269,#40270,#40271,
#40272),.UNSPECIFIED.,.F.,.F.,(4,1,1,1,1,1,1,1,1,1,1,1,1,1,4),(0.,0.125,
0.1875,0.25,0.3125,0.375,0.5,0.625,0.6875,0.71875,0.75,0.78125,0.8125,0.875,
0.999973904155701),.UNSPECIFIED.);
#1023=B_SPLINE_CURVE_WITH_KNOTS('',3,(#40274,#40275,#40276,#40277,#40278,
#40279,#40280,#40281,#40282,#40283,#40284,#40285,#40286,#40287,#40288,#40289,
#40290,#40291,#40292,#40293,#40294,#40295,#40296,#40297,#40298,#40299,#40300,
#40301,#40302,#40303,#40304,#40305,#40306,#40307,#40308,#40309,#40310,#40311,
#40312,#40313,#40314,#40315,#40316,#40317,#40318,#40319),.UNSPECIFIED.,
 .F.,.F.,(4,2,2,2,2,2,2,2,2,2,2,2,2,2,2,2,2,2,2,2,2,2,4),(2.47988659577903E-5,
0.00978202028211238,0.0213215802168401,0.0228946245359042,0.0246012949911653,
0.0286969595382463,0.0419977049211027,0.0820560797602515,0.0875251626699372,
0.116649382017729,0.155456996931585,0.17693206420461,0.200598959304169,
0.250883813270901,0.282287570163106,0.337211637910956,0.420331994699351,
0.430730860332875,0.466657227821203,0.47845661856984,0.485622048026449,
0.49444503678418,0.503140993568406),.UNSPECIFIED.);
#1024=B_SPLINE_CURVE_WITH_KNOTS('',3,(#40321,#40322,#40323,#40324),
 .UNSPECIFIED.,.F.,.F.,(4,4),(-1.14031632988646,-1.04922087046088),
 .UNSPECIFIED.);
#1025=B_SPLINE_CURVE_WITH_KNOTS('',3,(#40326,#40327,#40328,#40329,#40330,
#40331,#40332,#40333,#40334,#40335,#40336,#40337,#40338,#40339,#40340,#40341,
#40342),.UNSPECIFIED.,.F.,.F.,(4,1,1,1,1,1,1,1,1,1,1,1,1,1,4),(0.,0.125,
0.1875,0.25,0.3125,0.375,0.5,0.625,0.6875,0.71875,0.75,0.78125,0.8125,0.875,
0.999999976967435),.UNSPECIFIED.);
#1026=B_SPLINE_CURVE_WITH_KNOTS('',3,(#40344,#40345,#40346,#40347,#40348,
#40349,#40350,#40351,#40352,#40353,#40354,#40355,#40356,#40357,#40358,#40359,
#40360),.UNSPECIFIED.,.F.,.F.,(4,1,1,1,1,1,1,1,1,1,1,1,1,1,4),(1.69410983812543E-8,
0.125,0.1875,0.21875,0.25,0.28125,0.3125,0.375,0.5,0.625,0.6875,0.75,0.8125,
0.875,1.),.UNSPECIFIED.);
#1027=B_SPLINE_CURVE_WITH_KNOTS('',3,(#40361,#40362,#40363,#40364),
 .UNSPECIFIED.,.F.,.F.,(4,4),(-1.14138748856057,-1.05023984115422),
 .UNSPECIFIED.);
#1028=B_SPLINE_CURVE_WITH_KNOTS('',3,(#40368,#40369,#40370,#40371,#40372,
#40373,#40374,#40375,#40376,#40377,#40378,#40379,#40380,#40381,#40382,#40383,
#40384),.UNSPECIFIED.,.F.,.F.,(4,1,1,1,1,1,1,1,1,1,1,1,1,1,4),(0.,0.125,
0.1875,0.25,0.3125,0.375,0.5,0.625,0.6875,0.71875,0.75,0.78125,0.8125,0.875,
0.999999958992443),.UNSPECIFIED.);
#1029=B_SPLINE_CURVE_WITH_KNOTS('',3,(#40386,#40387,#40388,#40389,#40390,
#40391,#40392,#40393,#40394,#40395,#40396,#40397,#40398,#40399,#40400,#40401,
#40402),.UNSPECIFIED.,.F.,.F.,(4,1,1,1,1,1,1,1,1,1,1,1,1,1,4),(0.,0.125,
0.1875,0.21875,0.25,0.28125,0.3125,0.375,0.5,0.625,0.6875,0.75,0.8125,0.875,
1.),.UNSPECIFIED.);
#1030=B_SPLINE_CURVE_WITH_KNOTS('',3,(#40404,#40405,#40406,#40407),
 .UNSPECIFIED.,.F.,.F.,(4,4),(-1.14907451824135,-1.05612055222212),
 .UNSPECIFIED.);
#1031=B_SPLINE_CURVE_WITH_KNOTS('',3,(#40409,#40410,#40411,#40412,#40413,
#40414,#40415,#40416,#40417,#40418,#40419,#40420,#40421,#40422,#40423,#40424,
#40425),.UNSPECIFIED.,.F.,.F.,(4,1,1,1,1,1,1,1,1,1,1,1,1,1,4),(0.,0.125,
0.1875,0.25,0.3125,0.375,0.5,0.625,0.6875,0.71875,0.75,0.78125,0.8125,0.875,
0.999999976401986),.UNSPECIFIED.);
#1032=B_SPLINE_CURVE_WITH_KNOTS('',3,(#40427,#40428,#40429,#40430,#40431,
#40432,#40433,#40434,#40435,#40436,#40437,#40438,#40439,#40440,#40441,#40442,
#40443),.UNSPECIFIED.,.F.,.F.,(4,1,1,1,1,1,1,1,1,1,1,1,1,1,4),(1.69808900141672E-8,
0.125,0.1875,0.21875,0.25,0.28125,0.3125,0.375,0.5,0.625,0.6875,0.75,0.8125,
0.875,1.),.UNSPECIFIED.);
#1033=B_SPLINE_CURVE_WITH_KNOTS('',3,(#40444,#40445,#40446,#40447),
 .UNSPECIFIED.,.F.,.F.,(4,4),(-1.14206554603712,-1.05097269226909),
 .UNSPECIFIED.);
#1034=B_SPLINE_CURVE_WITH_KNOTS('',3,(#40451,#40452,#40453,#40454,#40455,
#40456,#40457,#40458,#40459,#40460,#40461,#40462,#40463,#40464,#40465,#40466,
#40467),.UNSPECIFIED.,.F.,.F.,(4,1,1,1,1,1,1,1,1,1,1,1,1,1,4),(0.,0.125,
0.1875,0.25,0.3125,0.375,0.5,0.625,0.6875,0.71875,0.75,0.78125,0.8125,0.875,
0.999999966016196),.UNSPECIFIED.);
#1035=B_SPLINE_CURVE_WITH_KNOTS('',3,(#40469,#40470,#40471,#40472,#40473,
#40474,#40475,#40476,#40477,#40478,#40479,#40480,#40481,#40482,#40483,#40484,
#40485),.UNSPECIFIED.,.F.,.F.,(4,1,1,1,1,1,1,1,1,1,1,1,1,1,4),(0.,0.125,
0.1875,0.21875,0.25,0.28125,0.3125,0.375,0.5,0.625,0.6875,0.75,0.8125,0.875,
1.),.UNSPECIFIED.);
#1036=B_SPLINE_CURVE_WITH_KNOTS('',3,(#40487,#40488,#40489,#40490),
 .UNSPECIFIED.,.F.,.F.,(4,4),(-1.14014949111156,-1.04925591765877),
 .UNSPECIFIED.);
#1037=B_SPLINE_CURVE_WITH_KNOTS('',3,(#40492,#40493,#40494,#40495,#40496,
#40497,#40498,#40499,#40500,#40501,#40502,#40503,#40504,#40505,#40506,#40507,
#40508),.UNSPECIFIED.,.F.,.F.,(4,1,1,1,1,1,1,1,1,1,1,1,1,1,4),(0.,0.125,
0.1875,0.25,0.3125,0.375,0.5,0.625,0.6875,0.71875,0.75,0.78125,0.8125,0.875,
0.999999978755288),.UNSPECIFIED.);
#1038=B_SPLINE_CURVE_WITH_KNOTS('',3,(#40510,#40511,#40512,#40513,#40514,
#40515,#40516,#40517,#40518,#40519,#40520,#40521,#40522,#40523,#40524,#40525,
#40526),.UNSPECIFIED.,.F.,.F.,(4,1,1,1,1,1,1,1,1,1,1,1,1,1,4),(2.33180965054172E-8,
0.125,0.1875,0.21875,0.25,0.28125,0.3125,0.375,0.5,0.625,0.6875,0.75,0.8125,
0.875,1.),.UNSPECIFIED.);
#1039=B_SPLINE_CURVE_WITH_KNOTS('',3,(#40527,#40528,#40529,#40530),
 .UNSPECIFIED.,.F.,.F.,(4,4),(-1.14020705449601,-1.04518868540341),
 .UNSPECIFIED.);
#1040=B_SPLINE_CURVE_WITH_KNOTS('',3,(#40534,#40535,#40536,#40537,#40538,
#40539,#40540,#40541,#40542,#40543,#40544,#40545,#40546,#40547,#40548,#40549,
#40550,#40551),.UNSPECIFIED.,.F.,.F.,(4,1,1,1,1,1,1,1,1,1,1,1,1,1,1,4),
(0.,0.125,0.1875,0.25,0.3125,0.375,0.4375,0.5,0.625,0.6875,0.71875,0.75,
0.78125,0.8125,0.875,1.),.UNSPECIFIED.);
#1041=B_SPLINE_CURVE_WITH_KNOTS('',3,(#40553,#40554,#40555,#40556,#40557,
#40558,#40559,#40560,#40561,#40562,#40563,#40564,#40565,#40566,#40567,#40568,
#40569,#40570),.UNSPECIFIED.,.F.,.F.,(4,1,1,1,1,1,1,1,1,1,1,1,1,1,1,4),
(9.65284522368403E-8,0.125,0.1875,0.21875,0.25,0.28125,0.3125,0.375,0.5,
0.5625,0.625,0.6875,0.75,0.8125,0.875,0.999999352149596),.UNSPECIFIED.);
#1042=B_SPLINE_CURVE_WITH_KNOTS('',3,(#40572,#40573,#40574,#40575),
 .UNSPECIFIED.,.F.,.F.,(4,4),(-1.14221789136096,-1.0513242695399),
 .UNSPECIFIED.);
#1043=B_SPLINE_CURVE_WITH_KNOTS('',3,(#40577,#40578,#40579,#40580,#40581,
#40582,#40583,#40584,#40585,#40586,#40587,#40588,#40589,#40590,#40591,#40592,
#40593,#40594),.UNSPECIFIED.,.F.,.F.,(4,1,1,1,1,1,1,1,1,1,1,1,1,1,1,4),
(0.,0.125,0.1875,0.25,0.3125,0.375,0.4375,0.5,0.625,0.6875,0.71875,0.75,
0.78125,0.8125,0.875,0.999999772281826),.UNSPECIFIED.);
#1044=B_SPLINE_CURVE_WITH_KNOTS('',3,(#40596,#40597,#40598,#40599,#40600,
#40601,#40602,#40603,#40604,#40605,#40606,#40607,#40608,#40609,#40610,#40611,
#40612,#40613),.UNSPECIFIED.,.F.,.F.,(4,1,1,1,1,1,1,1,1,1,1,1,1,1,1,4),
(0.,0.125,0.1875,0.21875,0.25,0.28125,0.3125,0.375,0.5,0.5625,0.625,0.6875,
0.75,0.8125,0.875,1.),.UNSPECIFIED.);
#1045=B_SPLINE_CURVE_WITH_KNOTS('',3,(#40614,#40615,#40616,#40617),
 .UNSPECIFIED.,.F.,.F.,(4,4),(-1.16809592630694,-1.07716888491671),
 .UNSPECIFIED.);
#1046=B_SPLINE_CURVE_WITH_KNOTS('',3,(#40621,#40622,#40623,#40624,#40625,
#40626,#40627,#40628,#40629,#40630,#40631,#40632,#40633,#40634,#40635,#40636,
#40637),.UNSPECIFIED.,.F.,.F.,(4,1,1,1,1,1,1,1,1,1,1,1,1,1,4),(1.05070398993036E-5,
0.125,0.1875,0.25,0.3125,0.375,0.5,0.625,0.6875,0.71875,0.75,0.78125,0.8125,
0.875,1.),.UNSPECIFIED.);
#1047=B_SPLINE_CURVE_WITH_KNOTS('',3,(#40639,#40640,#40641,#40642,#40643,
#40644,#40645,#40646,#40647,#40648,#40649,#40650,#40651,#40652,#40653,#40654,
#40655),.UNSPECIFIED.,.F.,.F.,(4,1,1,1,1,1,1,1,1,1,1,1,1,1,4),(1.68482309315291E-7,
0.125,0.1875,0.21875,0.25,0.28125,0.3125,0.375,0.5,0.625,0.6875,0.75,0.8125,
0.875,1.),.UNSPECIFIED.);
#1048=B_SPLINE_CURVE_WITH_KNOTS('',3,(#40657,#40658,#40659,#40660,#40661,
#40662,#40663,#40664,#40665,#40666,#40667,#40668,#40669,#40670,#40671,#40672,
#40673,#40674,#40675,#40676,#40677,#40678,#40679,#40680,#40681),
 .UNSPECIFIED.,.F.,.F.,(4,3,3,3,3,3,3,3,4),(9.0152389462332E-6,0.250000179528252,
0.375000149606877,0.500000119685501,0.539828000683998,0.625000089764126,
0.750000059842751,0.81706191736929,0.999996337578903),.UNSPECIFIED.);
#1049=B_SPLINE_CURVE_WITH_KNOTS('',3,(#40683,#40684,#40685,#40686,#40687,
#40688,#40689,#40690,#40691,#40692,#40693,#40694,#40695,#40696,#40697,#40698,
#40699,#40700),.UNSPECIFIED.,.F.,.F.,(4,1,1,1,1,1,1,1,1,1,1,1,1,1,1,4),
(0.,0.125,0.1875,0.25,0.3125,0.375,0.4375,0.5,0.625,0.6875,0.71875,0.75,
0.78125,0.8125,0.875,0.999999833967708),.UNSPECIFIED.);
#1050=B_SPLINE_CURVE_WITH_KNOTS('',3,(#40702,#40703,#40704,#40705,#40706,
#40707,#40708,#40709,#40710,#40711,#40712,#40713,#40714,#40715,#40716,#40717,
#40718),.UNSPECIFIED.,.F.,.F.,(4,1,1,1,1,1,1,1,1,1,1,1,1,1,4),(0.,0.125,
0.1875,0.21875,0.25,0.28125,0.3125,0.375,0.5,0.625,0.6875,0.75,0.8125,0.875,
1.),.UNSPECIFIED.);
#1051=B_SPLINE_CURVE_WITH_KNOTS('',3,(#40719,#40720,#40721,#40722,#40723,
#40724,#40725,#40726,#40727),.UNSPECIFIED.,.F.,.F.,(4,1,1,1,1,1,4),(5.75355075983042E-8,
0.249999939248312,0.374999908872468,0.499999878496624,0.62499984812078,
0.749999817744936,0.999999756993248),.UNSPECIFIED.);
#1052=B_SPLINE_CURVE_WITH_KNOTS('',3,(#40731,#40732,#40733,#40734,#40735,
#40736,#40737,#40738,#40739,#40740,#40741,#40742,#40743,#40744,#40745,#40746,
#40747),.UNSPECIFIED.,.F.,.F.,(4,1,1,1,1,1,1,1,1,1,1,1,1,1,4),(0.000130637014181663,
0.125,0.1875,0.25,0.3125,0.375,0.5,0.625,0.6875,0.71875,0.75,0.78125,0.8125,
0.875,0.999999986791086),.UNSPECIFIED.);
#1053=B_SPLINE_CURVE_WITH_KNOTS('',3,(#40749,#40750,#40751,#40752,#40753,
#40754,#40755,#40756,#40757,#40758,#40759,#40760,#40761,#40762,#40763,#40764,
#40765,#40766,#40767),.UNSPECIFIED.,.F.,.F.,(4,1,1,1,1,1,1,1,1,1,1,1,1,
1,1,1,4),(7.60606706307879E-8,0.125,0.1875,0.21875,0.25,0.28125,0.3125,
0.375,0.5,0.625,0.6875,0.71875,0.75,0.78125,0.8125,0.875,1.),
 .UNSPECIFIED.);
#1054=B_SPLINE_CURVE_WITH_KNOTS('',3,(#40769,#40770,#40771,#40772,#40773,
#40774),.UNSPECIFIED.,.F.,.F.,(4,2,4),(4.75084510343136E-5,0.0562772365901649,
0.106122687546361),.UNSPECIFIED.);
#1055=B_SPLINE_CURVE_WITH_KNOTS('',3,(#40776,#40777,#40778,#40779,#40780,
#40781,#40782,#40783),.UNSPECIFIED.,.F.,.F.,(4,2,2,4),(0.163849162898279,
0.18750836405779,0.272594094712416,0.355211229604226),.UNSPECIFIED.);
#1056=B_SPLINE_CURVE_WITH_KNOTS('',3,(#40785,#40786,#40787,#40788,#40789,
#40790,#40791,#40792,#40793,#40794,#40795,#40796,#40797,#40798,#40799,#40800,
#40801),.UNSPECIFIED.,.F.,.F.,(4,1,1,1,1,1,1,1,1,1,1,1,1,1,4),(0.,0.125,
0.1875,0.21875,0.25,0.28125,0.3125,0.375,0.5,0.625,0.6875,0.75,0.8125,0.875,
1.),.UNSPECIFIED.);
#1057=B_SPLINE_CURVE_WITH_KNOTS('',3,(#40802,#40803,#40804,#40805,#40806,
#40807,#40808,#40809,#40810,#40811,#40812,#40813,#40814,#40815,#40816,#40817,
#40818,#40819,#40820,#40821,#40822,#40823),.UNSPECIFIED.,.F.,.F.,(4,3,3,
3,3,3,3,4),(1.21073077537255E-7,0.25,0.375,0.477137911585377,0.5,0.625,
0.75,1.),.UNSPECIFIED.);
#1058=B_SPLINE_CURVE_WITH_KNOTS('',3,(#40827,#40828,#40829,#40830,#40831,
#40832,#40833,#40834,#40835,#40836,#40837,#40838,#40839,#40840,#40841,#40842,
#40843),.UNSPECIFIED.,.F.,.F.,(4,1,1,1,1,1,1,1,1,1,1,1,1,1,4),(0.,0.125,
0.1875,0.25,0.3125,0.375,0.5,0.625,0.6875,0.71875,0.75,0.78125,0.8125,0.875,
1.),.UNSPECIFIED.);
#1059=B_SPLINE_CURVE_WITH_KNOTS('',3,(#40845,#40846,#40847,#40848,#40849,
#40850,#40851,#40852,#40853,#40854,#40855,#40856,#40857,#40858,#40859,#40860,
#40861),.UNSPECIFIED.,.F.,.F.,(4,1,1,1,1,1,1,1,1,1,1,1,1,1,4),(9.8229068389049E-8,
0.125,0.1875,0.21875,0.25,0.28125,0.3125,0.375,0.5,0.625,0.6875,0.75,0.8125,
0.875,1.),.UNSPECIFIED.);
#1060=B_SPLINE_CURVE_WITH_KNOTS('',3,(#40863,#40864,#40865,#40866),
 .UNSPECIFIED.,.F.,.F.,(4,4),(8.86637280826242E-5,1.),.UNSPECIFIED.);
#1061=B_SPLINE_CURVE_WITH_KNOTS('',3,(#40868,#40869,#40870,#40871,#40872,
#40873,#40874,#40875,#40876,#40877,#40878,#40879,#40880,#40881,#40882,#40883,
#40884),.UNSPECIFIED.,.F.,.F.,(4,1,1,1,1,1,1,1,1,1,1,1,1,1,4),(0.,0.125,
0.1875,0.25,0.3125,0.375,0.5,0.625,0.6875,0.71875,0.75,0.78125,0.8125,0.875,
0.999999976690837),.UNSPECIFIED.);
#1062=B_SPLINE_CURVE_WITH_KNOTS('',3,(#40886,#40887,#40888,#40889,#40890,
#40891,#40892,#40893,#40894,#40895,#40896,#40897,#40898,#40899,#40900,#40901,
#40902),.UNSPECIFIED.,.F.,.F.,(4,1,1,1,1,1,1,1,1,1,1,1,1,1,4),(2.52343280623569E-8,
0.125,0.1875,0.21875,0.25,0.28125,0.3125,0.375,0.5,0.625,0.6875,0.75,0.8125,
0.875,1.),.UNSPECIFIED.);
#1063=B_SPLINE_CURVE_WITH_KNOTS('',3,(#40903,#40904,#40905,#40906),
 .UNSPECIFIED.,.F.,.F.,(4,4),(0.,0.999911620910334),.UNSPECIFIED.);
#1064=B_SPLINE_CURVE_WITH_KNOTS('',3,(#40910,#40911,#40912,#40913,#40914,
#40915,#40916,#40917,#40918,#40919,#40920,#40921,#40922,#40923,#40924,#40925,
#40926,#40927,#40928),.UNSPECIFIED.,.F.,.F.,(4,3,3,3,3,3,4),(0.,0.25,0.375,
0.5,0.625,0.75,1.),.UNSPECIFIED.);
#1065=B_SPLINE_CURVE_WITH_KNOTS('',3,(#40930,#40931,#40932,#40933,#40934,
#40935,#40936,#40937,#40938,#40939,#40940,#40941,#40942,#40943,#40944,#40945,
#40946),.UNSPECIFIED.,.F.,.F.,(4,1,1,1,1,1,1,1,1,1,1,1,1,1,4),(0.,0.125,
0.1875,0.25,0.3125,0.375,0.5,0.625,0.6875,0.71875,0.75,0.78125,0.8125,0.875,
0.999999985754337),.UNSPECIFIED.);
#1066=B_SPLINE_CURVE_WITH_KNOTS('',3,(#40948,#40949,#40950,#40951,#40952,
#40953,#40954,#40955),.UNSPECIFIED.,.F.,.F.,(4,2,2,4),(0.190745761082819,
0.195318232891979,0.294499389363961,0.344632001218864),.UNSPECIFIED.);
#1067=B_SPLINE_CURVE_WITH_KNOTS('',3,(#40957,#40958,#40959,#40960,#40961,
#40962,#40963,#40964,#40965,#40966,#40967,#40968,#40969,#40970,#40971,#40972,
#40973,#40974,#40975),.UNSPECIFIED.,.F.,.F.,(4,3,3,3,3,3,4),(0.00444335916602599,
0.25,0.375,0.5,0.625,0.75,1.),.UNSPECIFIED.);
#1068=B_SPLINE_CURVE_WITH_KNOTS('',3,(#40977,#40978,#40979,#40980,#40981,
#40982),.UNSPECIFIED.,.F.,.F.,(4,2,4),(0.695401129409354,0.724410509776768,
0.80598859149533),.UNSPECIFIED.);
#1069=B_SPLINE_CURVE_WITH_KNOTS('',3,(#40983,#40984,#40985,#40986,#40987,
#40988),.UNSPECIFIED.,.F.,.F.,(4,2,4),(0.663566354634175,0.697565900531653,
0.775630565396341),.UNSPECIFIED.);
#1070=B_SPLINE_CURVE_WITH_KNOTS('',3,(#41006,#41007,#41008,#41009,#41010,
#41011,#41012,#41013,#41014,#41015,#41016,#41017,#41018,#41019),
 .UNSPECIFIED.,.F.,.F.,(4,2,2,2,2,2,4),(-0.01507830543452,-0.0131185429662993,
-0.0110343515831027,-0.00717762894557236,-0.00331925504980651,-7.55493420441511E-7,
0.000663167325391246),.UNSPECIFIED.);
#1071=B_SPLINE_CURVE_WITH_KNOTS('',3,(#41020,#41021,#41022,#41023,#41024,
#41025,#41026,#41027,#41028,#41029,#41030,#41031,#41032,#41033,#41034),
 .UNSPECIFIED.,.F.,.F.,(4,2,2,2,2,2,1,4),(0.000110379421385148,0.00233264133731716,
0.00497678284857156,0.00924166096140105,0.0134515198447832,0.0196622706603402,
0.0205807311791432,0.0214991916979463),.UNSPECIFIED.);
#1072=B_SPLINE_CURVE_WITH_KNOTS('',3,(#41036,#41037,#41038,#41039,#41040,
#41041,#41042,#41043,#41044,#41045,#41046,#41047,#41048,#41049,#41050),
 .UNSPECIFIED.,.F.,.F.,(4,2,2,2,2,2,1,4),(-0.0107327112951072,-0.00932351786082577,
-0.00775928892532341,-0.00524294687388514,-0.00290996407673086,0.,0.000360584068865346,
0.000721168137730691),.UNSPECIFIED.);
#1073=B_SPLINE_CURVE_WITH_KNOTS('',3,(#41066,#41067,#41068,#41069,#41070,
#41071,#41072,#41073,#41074,#41075,#41076,#41077,#41078,#41079,#41080),
 .UNSPECIFIED.,.F.,.F.,(4,1,2,2,2,2,2,4),(-0.000831847091679277,-0.000415718710644378,
4.09670390521676E-7,0.0033967242603589,0.00614729864505439,0.00905447795736422,
0.0108472486697068,0.0123547719820523),.UNSPECIFIED.);
#1074=B_SPLINE_CURVE_WITH_KNOTS('',3,(#41096,#41097,#41098,#41099,#41100,
#41101,#41102,#41103,#41104,#41105,#41106),.UNSPECIFIED.,.F.,.F.,(4,2,2,
2,1,4),(-0.0100540276238623,-0.00756834425613214,-0.00473757454927083,-0.00188169994745774,
-9.55994444132124E-5,0.),.UNSPECIFIED.);
#1075=B_SPLINE_CURVE_WITH_KNOTS('',3,(#41108,#41109,#41110,#41111,#41112,
#41113,#41114,#41115,#41116,#41117,#41118,#41119,#41120,#41121,#41122,#41123),
 .UNSPECIFIED.,.F.,.F.,(4,2,2,2,2,2,2,4),(0.0109454996995501,0.0121640780030457,
0.0143626163448094,0.0170563730060771,0.0211889870954567,0.0237556002878168,
0.0248641156521573,0.0252222827077722),.UNSPECIFIED.);
#1076=B_SPLINE_CURVE_WITH_KNOTS('',3,(#41140,#41141,#41142,#41143,#41144,
#41145,#41146,#41147,#41148,#41149,#41150,#41151,#41152,#41153),
 .UNSPECIFIED.,.F.,.F.,(4,2,2,2,2,2,4),(-0.0150736213696635,-0.0131145281722507,
-0.0110310296272098,-0.00717567152716654,-0.0033185625050402,-7.27641435771531E-7,
0.000662519455103558),.UNSPECIFIED.);
#1077=B_SPLINE_CURVE_WITH_KNOTS('',3,(#41154,#41155,#41156,#41157,#41158,
#41159,#41160,#41161,#41162,#41163,#41164,#41165,#41166,#41167,#41168),
 .UNSPECIFIED.,.F.,.F.,(4,2,2,2,2,2,1,4),(0.000109277498535426,0.00233122821911415,
0.0049736263892055,0.00923726610637425,0.0133900437988086,0.0195564321408132,
0.0207410647190443,0.0219256972972754),.UNSPECIFIED.);
#1078=B_SPLINE_CURVE_WITH_KNOTS('',3,(#41170,#41171,#41172,#41173,#41174,
#41175,#41176,#41177,#41178,#41179,#41180,#41181,#41182,#41183,#41184),
 .UNSPECIFIED.,.F.,.F.,(4,2,2,2,2,2,1,4),(-0.0111927944725922,-0.00971535165057207,
-0.00807540492660865,-0.00543708380189962,-0.00299063929573346,0.,0.000367166839165872,
0.000734333678331744),.UNSPECIFIED.);
#1079=B_SPLINE_CURVE_WITH_KNOTS('',3,(#41200,#41201,#41202,#41203,#41204,
#41205,#41206,#41207,#41208,#41209,#41210,#41211,#41212,#41213,#41214),
 .UNSPECIFIED.,.F.,.F.,(4,1,2,2,2,2,2,4),(-0.000841606462170108,-0.000420623329405298,
3.59803359512067E-7,0.00341940295621038,0.00619678753011438,0.00913724210812968,
0.010951633465127,0.0124778685491557),.UNSPECIFIED.);
#1080=B_SPLINE_CURVE_WITH_KNOTS('',3,(#41230,#41231,#41232,#41233,#41234,
#41235,#41236,#41237,#41238,#41239,#41240,#41241,#41242,#41243),
 .UNSPECIFIED.,.F.,.F.,(4,2,2,2,2,2,4),(-0.0126310563478074,-0.0110402596235953,
-0.00932700685802013,-0.00615674109370743,-0.00298505983244596,0.,0.000652684360861046),
 .UNSPECIFIED.);
#1081=B_SPLINE_CURVE_WITH_KNOTS('',3,(#41245,#41246,#41247,#41248,#41249,
#41250,#41251,#41252,#41253,#41254,#41255,#41256,#41257,#41258),
 .UNSPECIFIED.,.F.,.F.,(4,2,2,2,2,2,4),(0.,0.00233205662631541,0.00492501613407614,
0.00904723499130749,0.0129234630237897,0.0187564284015468,0.0218496675394978),
 .UNSPECIFIED.);
#1082=B_SPLINE_CURVE_WITH_KNOTS('',3,(#41289,#41290,#41291,#41292,#41293,
#41294,#41295,#41296,#41297,#41298,#41299,#41300,#41301,#41302),
 .UNSPECIFIED.,.F.,.F.,(4,2,2,2,2,2,4),(-0.015067945938605,-0.0131096675981174,
-0.0110270176791167,-0.0071733025740434,-0.00331774097657231,-6.94603856923534E-7,
0.000661736637824425),.UNSPECIFIED.);
#1083=B_SPLINE_CURVE_WITH_KNOTS('',3,(#41303,#41304,#41305,#41306,#41307,
#41308,#41309,#41310,#41311,#41312,#41313,#41314,#41315,#41316),
 .UNSPECIFIED.,.F.,.F.,(4,2,2,2,2,2,4),(0.000108411815062279,0.00233046514898696,
0.00497190484499379,0.00923486963259684,0.0133609629567941,0.0174716316940529,
0.018064453437383),.UNSPECIFIED.);
#1084=B_SPLINE_CURVE_WITH_KNOTS('',3,(#41318,#41319,#41320,#41321,#41322,
#41323,#41324,#41325,#41326,#41327,#41328,#41329,#41330,#41331,#41332),
 .UNSPECIFIED.,.F.,.F.,(4,2,2,2,2,2,1,4),(-0.0112911210319579,-0.00979969372819557,
-0.00814422742212235,-0.00548091191237493,-0.00301110838872929,0.,0.000370911555962369,
0.000741823111924738),.UNSPECIFIED.);
#1085=B_SPLINE_CURVE_WITH_KNOTS('',3,(#41348,#41349,#41350,#41351,#41352,
#41353,#41354,#41355,#41356,#41357,#41358,#41359,#41360,#41361,#41362),
 .UNSPECIFIED.,.F.,.F.,(4,1,2,2,2,2,2,4),(-0.000845952505115191,-0.000422815860888459,
3.20783338272771E-7,0.00342787238279231,0.00621649248522469,0.0091738937142793,
0.0109998757388608,0.0125362536341693),.UNSPECIFIED.);
#1086=B_SPLINE_CURVE_WITH_KNOTS('',3,(#41378,#41379,#41380,#41381,#41382,
#41383,#41384,#41385,#41386,#41387,#41388,#41389,#41390,#41391),
 .UNSPECIFIED.,.F.,.F.,(4,2,2,2,2,2,4),(-0.0122863233744583,-0.0107429899947187,
-0.00908185001333585,-0.00600812479454555,-0.00293295547261242,0.,0.000649621328147838),
 .UNSPECIFIED.);
#1087=B_SPLINE_CURVE_WITH_KNOTS('',3,(#41393,#41394,#41395,#41396,#41397,
#41398,#41399,#41400,#41401,#41402,#41403,#41404,#41405,#41406),
 .UNSPECIFIED.,.F.,.F.,(4,2,2,2,2,2,4),(0.,0.00233208722840324,0.00492509994382487,
0.0090473081885449,0.012910133820222,0.0166890239584757,0.0172660039537804),
 .UNSPECIFIED.);
#1088=B_SPLINE_CURVE_WITH_KNOTS('',3,(#41437,#41438,#41439,#41440,#41441,
#41442,#41443,#41444,#41445,#41446,#41447,#41448,#41449,#41450),
 .UNSPECIFIED.,.F.,.F.,(4,2,2,2,2,2,4),(-0.0150618266103595,-0.0131044294361987,
-0.0110226997841704,-0.00717075164604429,-0.00331686670257359,-6.61750749050491E-7,
0.000660888945518815),.UNSPECIFIED.);
#1089=B_SPLINE_CURVE_WITH_KNOTS('',3,(#41451,#41452,#41453,#41454,#41455,
#41456,#41457,#41458,#41459,#41460,#41461,#41462,#41463,#41464),
 .UNSPECIFIED.,.F.,.F.,(4,2,2,2,2,2,4),(0.000107524573743238,0.00233075355229494,
0.00497250195749481,0.00923570004390666,0.0133716966279069,0.0197477605613191,
0.0233570440188243),.UNSPECIFIED.);
#1090=B_SPLINE_CURVE_WITH_KNOTS('',3,(#41466,#41467,#41468,#41469,#41470,
#41471,#41472,#41473,#41474,#41475,#41476,#41477,#41478,#41479,#41480),
 .UNSPECIFIED.,.F.,.F.,(4,2,2,2,2,2,1,4),(-0.0112689852378272,-0.00978070704858543,
-0.0081286839041701,-0.00547107361921424,-0.00300660551843908,0.,0.000370059615394522,
0.000740119230789043),.UNSPECIFIED.);
#1091=B_SPLINE_CURVE_WITH_KNOTS('',3,(#41496,#41497,#41498,#41499,#41500,
#41501,#41502,#41503,#41504,#41505,#41506,#41507,#41508,#41509,#41510),
 .UNSPECIFIED.,.F.,.F.,(4,1,2,2,2,2,2,4),(-0.000852309778855015,-0.000426014539963934,
2.80698927146807E-7,0.00344207743051125,0.00624846680252986,0.00922991249153885,
0.0110719050982193,0.0126221279026672),.UNSPECIFIED.);
#1092=B_SPLINE_CURVE_WITH_KNOTS('',3,(#41526,#41527,#41528,#41529,#41530,
#41531,#41532,#41533,#41534,#41535,#41536,#41537,#41538,#41539),
 .UNSPECIFIED.,.F.,.F.,(4,2,2,2,2,2,4),(-0.0112537356406148,-0.0098521206422284,
-0.00834440416079227,-0.0055546808585686,-0.0027635731133648,0.,0.000645987732377855),
 .UNSPECIFIED.);
#1093=B_SPLINE_CURVE_WITH_KNOTS('',3,(#41541,#41542,#41543,#41544,#41545,
#41546,#41547,#41548,#41549,#41550,#41551,#41552,#41553,#41554),
 .UNSPECIFIED.,.F.,.F.,(4,2,2,2,2,2,4),(0.,0.0023321032472572,0.0049251475977755,
0.00904732760149453,0.0128912897831174,0.0181134987013173,0.0197352105609782),
 .UNSPECIFIED.);
#1094=B_SPLINE_CURVE_WITH_KNOTS('',3,(#41585,#41586,#41587,#41588,#41589,
#41590,#41591,#41592,#41593,#41594,#41595,#41596,#41597),.UNSPECIFIED.,
 .F.,.F.,(4,2,2,2,2,1,4),(0.,0.00196346055139926,0.00405154240681477,0.00791565834815476,
0.011781209799845,0.0156720041993471,0.0157373755669737),.UNSPECIFIED.);
#1095=B_SPLINE_CURVE_WITH_KNOTS('',3,(#41598,#41599,#41600,#41601,#41602,
#41603,#41604,#41605,#41606,#41607,#41608,#41609,#41610,#41611,#41612),
 .UNSPECIFIED.,.F.,.F.,(4,2,2,2,2,2,1,4),(0.000114739303757549,0.0023334430315381,
0.00497816475940246,0.00924233839267071,0.013514656302117,0.01989139391585,
0.0206513029014127,0.0214112118869755),.UNSPECIFIED.);
#1096=B_SPLINE_CURVE_WITH_KNOTS('',3,(#41614,#41615,#41616,#41617,#41618,
#41619,#41620,#41621,#41622,#41623,#41624,#41625,#41626,#41627,#41628),
 .UNSPECIFIED.,.F.,.F.,(4,2,2,2,2,2,1,4),(-0.0103555407250338,-0.00899996641982785,
-0.00749506887131186,-0.00507443351976568,-0.00283082962523163,-2.71882089498271E-8,
0.000345077207643678,0.000690181603496307),.UNSPECIFIED.);
#1097=B_SPLINE_CURVE_WITH_KNOTS('',3,(#41644,#41645,#41646,#41647,#41648,
#41649,#41650,#41651,#41652,#41653,#41654,#41655,#41656,#41657,#41658),
 .UNSPECIFIED.,.F.,.F.,(4,1,2,2,2,2,2,4),(-0.000788977077809716,-0.000394173563697078,
6.29950415558791E-7,0.00329621038696056,0.00593031022203129,0.00869747301509253,
0.0104000877764451,0.0118299274704398),.UNSPECIFIED.);
#1098=B_SPLINE_CURVE_WITH_KNOTS('',3,(#41674,#41675,#41676,#41677,#41678,
#41679,#41680,#41681,#41682,#41683,#41684,#41685,#41686),.UNSPECIFIED.,
 .F.,.F.,(4,2,2,2,2,1,4),(3.14269389793808E-5,0.0019634367265874,0.00405149149102325,
0.00791568233580109,0.0117813314665308,0.0182072596508539,0.0189955540620671),
 .UNSPECIFIED.);
#1099=B_SPLINE_CURVE_WITH_KNOTS('',3,(#41688,#41689,#41690,#41691,#41692,
#41693,#41694,#41695,#41696,#41697,#41698,#41699,#41700,#41701,#41702),
 .UNSPECIFIED.,.F.,.F.,(4,2,2,2,2,2,1,4),(0.,0.00233324186650626,0.00492806572685197,
0.00905241385642049,0.0130581050133669,0.0189330953861274,0.0196729935413677,
0.020412891696608),.UNSPECIFIED.);
#1100=B_SPLINE_CURVE_WITH_KNOTS('',3,(#41733,#41734,#41735,#41736,#41737,
#41738,#41739,#41740,#41741,#41742,#41743,#41744,#41745,#41746),
 .UNSPECIFIED.,.F.,.F.,(4,2,2,2,2,2,4),(-0.0150495343999896,-0.0130939107218886,
-0.0110140328587893,-0.00716563542438969,-0.00331511579488975,-5.99773702798442E-7,
0.000659170132904621),.UNSPECIFIED.);
#1101=B_SPLINE_CURVE_WITH_KNOTS('',3,(#41747,#41748,#41749,#41750,#41751,
#41752,#41753,#41754,#41755,#41756,#41757,#41758,#41759,#41760,#41761),
 .UNSPECIFIED.,.F.,.F.,(4,2,2,2,2,2,1,4),(0.000106052581580669,0.00232820999548284,
0.00496681683786704,0.00922777203689892,0.0132846981695113,0.0188863847946317,
0.0192382229087076,0.0195900610227836),.UNSPECIFIED.);
#1102=B_SPLINE_CURVE_WITH_KNOTS('',3,(#41763,#41764,#41765,#41766,#41767,
#41768,#41769,#41770,#41771,#41772,#41773,#41774,#41775,#41776,#41777),
 .UNSPECIFIED.,.F.,.F.,(4,2,2,2,2,2,1,4),(-0.0115842429505587,-0.0100510264851629,
-0.00834917125888717,-0.00561121344317483,-0.00307176429142002,0.,0.000381702300701627,
0.000763404601403253),.UNSPECIFIED.);
#1103=B_SPLINE_CURVE_WITH_KNOTS('',3,(#41793,#41794,#41795,#41796,#41797,
#41798,#41799,#41800,#41801,#41802,#41803,#41804,#41805,#41806,#41807),
 .UNSPECIFIED.,.F.,.F.,(4,1,2,2,2,2,2,4),(-0.000880146681302628,-0.000439983912980285,
1.78855342058124E-7,0.00390653624110326,0.00730515376515244,0.0109221460955771,
0.0131581175541924,0.0150406638244627),.UNSPECIFIED.);
#1104=B_SPLINE_CURVE_WITH_KNOTS('',3,(#41823,#41824,#41825,#41826,#41827,
#41828,#41829,#41830,#41831,#41832,#41833,#41834,#41835,#41836,#41837),
 .UNSPECIFIED.,.F.,.F.,(4,2,2,2,2,2,1,4),(-0.0133513511352758,-0.011657592117576,
-0.00983788659285601,-0.00647112579959316,-0.00310254776237713,0.,0.000318746772545248,
0.000637493545090497),.UNSPECIFIED.);
#1105=B_SPLINE_CURVE_WITH_KNOTS('',3,(#41839,#41840,#41841,#41842,#41843,
#41844,#41845,#41846,#41847,#41848,#41849,#41850,#41851,#41852,#41853),
 .UNSPECIFIED.,.F.,.F.,(4,2,2,2,2,2,1,4),(0.,0.00233178099632009,0.00492433938161485,
0.0090459596421507,0.0128089241713556,0.0177017983313787,0.0182620427457793,
0.0188222871601798),.UNSPECIFIED.);
#1106=B_SPLINE_CURVE_WITH_KNOTS('',3,(#41887,#41888,#41889,#41890,#41891,
#41892,#41893,#41894,#41895,#41896,#41897,#41898,#41899),.UNSPECIFIED.,
 .F.,.F.,(4,2,2,2,2,1,4),(0.,0.00196326848972203,0.00405116207364883,0.00791555727476664,
0.0117816205713716,0.0181921635821883,0.0189428821816501),.UNSPECIFIED.);
#1107=B_SPLINE_CURVE_WITH_KNOTS('',3,(#41900,#41901,#41902,#41903,#41904,
#41905,#41906,#41907,#41908,#41909,#41910,#41911,#41912,#41913,#41914),
 .UNSPECIFIED.,.F.,.F.,(4,2,2,2,2,2,1,4),(0.000136572166951063,0.00247342851894918,
0.00532496585133604,0.00983368386008723,0.0137734612749379,0.0191740995937165,
0.0195771026144167,0.0199801056351169),.UNSPECIFIED.);
#1108=B_SPLINE_CURVE_WITH_KNOTS('',3,(#41916,#41917,#41918,#41919),
 .UNSPECIFIED.,.F.,.F.,(4,4),(8.3932008892544E-11,0.000180398243040848),
 .UNSPECIFIED.);
#1109=B_SPLINE_CURVE_WITH_KNOTS('',3,(#41938,#41939,#41940,#41941,#41942,
#41943,#41944,#41945,#41946,#41947,#41948,#41949,#41950,#41951,#41952,#41953,
#41954,#41955,#41956,#41957,#41958,#41959,#41960,#41961,#41962,#41963,#41964,
#41965),.UNSPECIFIED.,.F.,.F.,(4,2,2,2,2,2,2,2,2,2,2,2,2,4),(0.00894662764801732,
0.00909966464154512,0.00911121326348854,0.0091199542058202,0.00912623258445597,
0.00913058031359492,0.00929759041527048,0.0098850490504378,0.0106648416904178,
0.0139432102084079,0.0202273547328932,0.0255820468844395,0.0289792940110764,
0.0317584900748122),.UNSPECIFIED.);
#1110=B_SPLINE_CURVE_WITH_KNOTS('',3,(#41984,#41985,#41986,#41987,#41988,
#41989,#41990,#41991,#41992,#41993,#41994,#41995,#41996,#41997,#41998,#41999,
#42000),.UNSPECIFIED.,.F.,.F.,(4,2,2,2,2,2,2,1,4),(4.1951250921174E-5,0.00196435693919538,
0.00405344923205659,0.00791854639957213,0.0117851888818974,0.0158670573322602,
0.0160255880433537,0.0161000392070421,0.0162193043519429),.UNSPECIFIED.);
#1111=B_SPLINE_CURVE_WITH_KNOTS('',3,(#42002,#42003,#42004,#42005,#42006,
#42007,#42008,#42009,#42010,#42011,#42012,#42013,#42014,#42015,#42016),
 .UNSPECIFIED.,.F.,.F.,(4,2,2,2,2,2,1,4),(0.,0.00229420255473759,0.00482815180681898,
0.0090803315048094,0.013385498353122,0.0196056546104732,0.0205956034810639,
0.0215855523516545),.UNSPECIFIED.);
#1112=B_SPLINE_CURVE_WITH_KNOTS('',3,(#42050,#42051,#42052,#42053,#42054,
#42055,#42056,#42057,#42058,#42059,#42060,#42061,#42062,#42063),
 .UNSPECIFIED.,.F.,.F.,(4,2,2,2,2,2,4),(-0.015055943205555,-0.0130993943583035,
-0.0110185504070684,-0.0071683015355778,-0.00331602697752475,-6.31338995112432E-7,
0.000660068888145464),.UNSPECIFIED.);
#1113=B_SPLINE_CURVE_WITH_KNOTS('',3,(#42064,#42065,#42066,#42067,#42068,
#42069,#42070,#42071,#42072,#42073,#42074,#42075,#42076,#42077,#42078),
 .UNSPECIFIED.,.F.,.F.,(4,2,2,2,2,2,1,4),(0.000106892049855475,0.00233143420029682,
0.00497395335443926,0.00923768954676918,0.013398888189913,0.0195568925545534,
0.0206769167852616,0.0217969410159699),.UNSPECIFIED.);
#1114=B_SPLINE_CURVE_WITH_KNOTS('',3,(#42080,#42081,#42082,#42083,#42084,
#42085,#42086,#42087,#42088,#42089,#42090,#42091,#42092,#42093,#42094),
 .UNSPECIFIED.,.F.,.F.,(4,2,2,2,2,2,1,4),(-0.0111954009729321,-0.0097175856695965,
-0.00807710698695868,-0.00543830669534266,-0.00299142164096204,0.,0.000367280343763525,
0.000734560687527049),.UNSPECIFIED.);
#1115=B_SPLINE_CURVE_WITH_KNOTS('',3,(#42110,#42111,#42112,#42113,#42114,
#42115,#42116,#42117,#42118,#42119,#42120,#42121,#42122,#42123,#42124),
 .UNSPECIFIED.,.F.,.F.,(4,1,2,2,2,2,2,4),(-0.000861296926150031,-0.00043052882115021,
2.39283849611752E-7,0.0038927349112584,0.0072753761053844,0.0108691153816805,
0.0130893297188529,0.014958222467424),.UNSPECIFIED.);
#1116=B_SPLINE_CURVE_WITH_KNOTS('',3,(#42140,#42141,#42142,#42143,#42144,
#42145,#42146,#42147,#42148,#42149,#42150,#42151,#42152,#42153),
 .UNSPECIFIED.,.F.,.F.,(4,2,2,2,2,2,4),(-0.0111679208697887,-0.00977760366207731,
-0.0082830305279969,-0.00551771990195264,-0.0027509784102351,0.,0.000641921215264818),
 .UNSPECIFIED.);
#1117=B_SPLINE_CURVE_WITH_KNOTS('',3,(#42155,#42156,#42157,#42158,#42159,
#42160,#42161,#42162,#42163,#42164,#42165,#42166,#42167,#42168),
 .UNSPECIFIED.,.F.,.F.,(4,2,2,2,2,2,4),(0.,0.0023320376215534,0.00492498614474746,
0.00904702037128976,0.0128643072555835,0.0182355035241461,0.020352993324196),
 .UNSPECIFIED.);
#1118=B_SPLINE_CURVE_WITH_KNOTS('',3,(#42199,#42200,#42201,#42202,#42203,
#42204,#42205,#42206,#42207,#42208,#42209,#42210,#42211),.UNSPECIFIED.,
 .F.,.F.,(4,2,2,2,2,1,4),(-0.00785439775943529,-0.00694783516724324,-0.00598372616180969,
-0.00419962083761066,-0.00241481918361066,-4.02804812405996E-7,4.97241742472335E-5),
 .UNSPECIFIED.);
#1119=B_SPLINE_CURVE_WITH_KNOTS('',3,(#42212,#42213,#42214,#42215,#42216,
#42217,#42218,#42219,#42220,#42221,#42222,#42223,#42224,#42225,#42226),
 .UNSPECIFIED.,.F.,.F.,(4,2,2,2,2,2,1,4),(0.000111276481820315,0.00233269010494002,
0.00497708127010691,0.00924237493668451,0.0134510062558102,0.0196593549777347,
0.0205845154023894,0.0215096758270441),.UNSPECIFIED.);
#1120=B_SPLINE_CURVE_WITH_KNOTS('',3,(#42228,#42229,#42230,#42231,#42232,
#42233,#42234,#42235,#42236,#42237,#42238,#42239,#42240,#42241,#42242),
 .UNSPECIFIED.,.F.,.F.,(4,2,2,2,2,2,1,4),(-0.0105397741274358,-0.0091581563716996,
-0.00762462685010155,-0.00515737932018193,-0.00286969551484454,-8.51844338470298E-9,
0.000352910589692364,0.000705829697828113),.UNSPECIFIED.);
#1121=B_SPLINE_CURVE_WITH_KNOTS('',3,(#42258,#42259,#42260,#42261,#42262,
#42263,#42264,#42265,#42266,#42267,#42268,#42269,#42270,#42271,#42272),
 .UNSPECIFIED.,.F.,.F.,(4,1,2,2,2,2,2,4),(-0.000811689830736768,-0.000405547746171915,
5.94338392938157E-7,0.00333387706802661,0.00601768004150032,0.0088698255226293,
0.0106324256073501,0.0121139768793991),.UNSPECIFIED.);
#1122=B_SPLINE_CURVE_WITH_KNOTS('',3,(#42288,#42289,#42290,#42291,#42292,
#42293,#42294,#42295,#42296,#42297,#42298,#42299,#42300),.UNSPECIFIED.,
 .F.,.F.,(4,2,2,2,2,1,4),(-0.0105931122047967,-0.00934770902821425,-0.00800490542156122,
-0.0055199269461594,-0.00303397666856782,0.,6.34168513411634E-5),
 .UNSPECIFIED.);
#1123=B_SPLINE_CURVE_WITH_KNOTS('',3,(#42302,#42303,#42304,#42305,#42306,
#42307,#42308,#42309,#42310,#42311,#42312,#42313,#42314,#42315,#42316),
 .UNSPECIFIED.,.F.,.F.,(4,2,2,2,2,2,1,4),(0.,0.00232779176441591,0.00491551587469812,
0.00903475405431627,0.0129741800549623,0.0186882063450052,0.019607760317714,
0.0205273142904227),.UNSPECIFIED.);
#1124=B_SPLINE_CURVE_WITH_KNOTS('',3,(#42347,#42348,#42349,#42350,#42351,
#42352,#42353,#42354,#42355,#42356,#42357,#42358,#42359),.UNSPECIFIED.,
 .F.,.F.,(4,2,2,2,2,1,4),(-0.0085716535892449,-0.00757466960194273,-0.00651440028288434,
-0.0045523430563402,-0.00258952361985675,-4.44344898067189E-7,5.49800542840583E-5),
 .UNSPECIFIED.);
#1125=B_SPLINE_CURVE_WITH_KNOTS('',3,(#42360,#42361,#42362,#42363,#42364,
#42365,#42366,#42367,#42368,#42369,#42370,#42371,#42372,#42373,#42374),
 .UNSPECIFIED.,.F.,.F.,(4,2,2,2,2,2,1,4),(0.000112127479441767,0.00233289939706983,
0.00497738360754069,0.00924236727099269,0.0134674534094052,0.0197117179381725,
0.0205879706113953,0.0214642232846181),.UNSPECIFIED.);
#1126=B_SPLINE_CURVE_WITH_KNOTS('',3,(#42376,#42377,#42378,#42379,#42380,
#42381,#42382,#42383,#42384,#42385,#42386,#42387,#42388,#42389,#42390),
 .UNSPECIFIED.,.F.,.F.,(4,2,2,2,2,2,1,4),(-0.0104881836929382,-0.00911386915215036,
-0.00758836984497876,-0.00513419361121672,-0.00285886238502574,-1.287952204089E-8,
0.000350823059822679,0.0007016589991674),.UNSPECIFIED.);
#1127=B_SPLINE_CURVE_WITH_KNOTS('',3,(#42406,#42407,#42408,#42409,#42410,
#42411,#42412,#42413,#42414,#42415,#42416,#42417,#42418,#42419,#42420),
 .UNSPECIFIED.,.F.,.F.,(4,1,2,2,2,2,2,4),(-0.000792937822276422,-0.000396163246703989,
6.11328868443299E-7,0.00328748317884194,0.00591926510315487,0.00871205474317156,
0.0104370897693979,0.0118870329010417),.UNSPECIFIED.);
#1128=B_SPLINE_CURVE_WITH_KNOTS('',3,(#42436,#42437,#42438,#42439,#42440,
#42441,#42442,#42443,#42444,#42445,#42446,#42447,#42448),.UNSPECIFIED.,
 .F.,.F.,(4,2,2,2,2,1,4),(-0.00632636884576775,-0.00561706452187852,-0.00485183122085223,
-0.00343569349346982,-0.00201900471914639,0.,3.19199699655112E-5),
 .UNSPECIFIED.);
#1129=B_SPLINE_CURVE_WITH_KNOTS('',3,(#42450,#42451,#42452,#42453,#42454,
#42455,#42456,#42457,#42458,#42459,#42460,#42461,#42462,#42463,#42464),
 .UNSPECIFIED.,.F.,.F.,(4,2,2,2,2,2,1,4),(0.,0.00232848787311146,0.00491736409388601,
0.00903785504559387,0.013060779628687,0.0189785945344682,0.0196952694771613,
0.0204119444198545),.UNSPECIFIED.);
#1130=B_SPLINE_CURVE_WITH_KNOTS('',3,(#42495,#42496,#42497,#42498,#42499,
#42500,#42501,#42502,#42503,#42504,#42505,#42506,#42507),.UNSPECIFIED.,
 .F.,.F.,(4,2,2,2,2,1,4),(-0.0156746030251293,-0.0137108965814205,-0.0116225427742933,
-0.0077579753523329,-0.00389191820682102,-4.8072468667934E-7,6.54569592049717E-5),
 .UNSPECIFIED.);
#1131=B_SPLINE_CURVE_WITH_KNOTS('',3,(#42508,#42509,#42510,#42511,#42512,
#42513,#42514,#42515,#42516,#42517,#42518,#42519,#42520,#42521,#42522),
 .UNSPECIFIED.,.F.,.F.,(4,2,2,2,2,2,1,4),(0.00011297725140699,0.00233326265007159,
0.00497803831869269,0.00924288561238248,0.0134933353480553,0.0198043992888978,
0.0206163190377781,0.0214282387866584),.UNSPECIFIED.);
#1132=B_SPLINE_CURVE_WITH_KNOTS('',3,(#42524,#42525,#42526,#42527,#42528,
#42529,#42530,#42531,#42532,#42533,#42534,#42535,#42536,#42537,#42538),
 .UNSPECIFIED.,.F.,.F.,(4,2,2,2,2,2,1,4),(-0.0104230568527555,-0.00905794707620465,
-0.00754258263594496,-0.00510489078265507,-0.0028451140281092,-1.83565382009393E-8,
0.000348073673261863,0.000696165703061926),.UNSPECIFIED.);
#1133=B_SPLINE_CURVE_WITH_KNOTS('',3,(#42554,#42555,#42556,#42557,#42558,
#42559,#42560,#42561,#42562,#42563,#42564,#42565,#42566,#42567,#42568),
 .UNSPECIFIED.,.F.,.F.,(4,1,2,2,2,2,2,4),(-0.000796385399367999,-0.00039789197282334,
6.01453721317817E-7,0.00330857856143206,0.00595907914351395,0.00875202157016118,
0.0104725301786227,0.0119190167735485),.UNSPECIFIED.);
#1134=B_SPLINE_CURVE_WITH_KNOTS('',3,(#42584,#42585,#42586,#42587,#42588,
#42589,#42590,#42591,#42592,#42593,#42594,#42595,#42596),.UNSPECIFIED.,
 .F.,.F.,(4,2,2,2,2,1,4),(-0.00114042523245899,-0.00101957547515334,-0.000889119527853727,
-0.00064769685874317,-0.000406180953020858,0.,6.52267443316575E-5),
 .UNSPECIFIED.);
#1135=B_SPLINE_CURVE_WITH_KNOTS('',3,(#42598,#42599,#42600,#42601,#42602,
#42603,#42604,#42605,#42606,#42607,#42608,#42609,#42610,#42611,#42612),
 .UNSPECIFIED.,.F.,.F.,(4,2,2,2,2,2,1,4),(0.,0.00233245052595259,0.00492601376639143,
0.009049051688289,0.0130249488395919,0.0188184019519407,0.0196232789088459,
0.0204281558657512),.UNSPECIFIED.);
#1136=B_SPLINE_CURVE_WITH_KNOTS('',3,(#42643,#42644,#42645,#42646,#42647,
#42648,#42649,#42650,#42651,#42652,#42653,#42654,#42655),.UNSPECIFIED.,
 .F.,.F.,(4,2,2,2,2,1,4),(0.,0.00196351159177689,0.00405165736140035,0.00791583594583384,
0.0117814988291894,0.015672372049312,0.015737753906218),.UNSPECIFIED.);
#1137=B_SPLINE_CURVE_WITH_KNOTS('',3,(#42656,#42657,#42658,#42659,#42660,
#42661,#42662,#42663,#42664,#42665,#42666,#42667,#42668,#42669,#42670),
 .UNSPECIFIED.,.F.,.F.,(4,2,2,2,2,2,1,4),(0.000113883995237668,0.00233233712716634,
0.00497583829970885,0.00923940492023475,0.0134494508874806,0.0196608351532728,
0.0205767816286905,0.0214927281041083),.UNSPECIFIED.);
#1138=B_SPLINE_CURVE_WITH_KNOTS('',3,(#42672,#42673,#42674,#42675,#42676,
#42677,#42678,#42679,#42680,#42681,#42682,#42683,#42684,#42685,#42686),
 .UNSPECIFIED.,.F.,.F.,(4,2,2,2,2,2,1,4),(-0.0105033578550783,-0.0091269097672519,
-0.00759894321490606,-0.00514090077078628,-0.00286219709327909,-1.13168538602715E-8,
0.000351419063789825,0.000702849444433509),.UNSPECIFIED.);
#1139=B_SPLINE_CURVE_WITH_KNOTS('',3,(#42702,#42703,#42704,#42705,#42706,
#42707,#42708,#42709,#42710,#42711,#42712,#42713,#42714,#42715,#42716),
 .UNSPECIFIED.,.F.,.F.,(4,1,2,2,2,2,2,4),(-0.000760560840304545,-0.00037994807411008,
6.64692084385941E-7,0.00319739705683137,0.00571058681035043,0.00835475150748551,
0.00998261483882353,0.0113501898484002),.UNSPECIFIED.);
#1140=B_SPLINE_CURVE_WITH_KNOTS('',3,(#42732,#42733,#42734,#42735,#42736,
#42737,#42738,#42739,#42740,#42741,#42742,#42743,#42744),.UNSPECIFIED.,
 .F.,.F.,(4,2,2,2,2,1,4),(3.02719502833942E-5,0.00196345017130929,0.00405152224974051,
0.00791573660758486,0.0117814260340998,0.018211181166248,0.0190097167577563),
 .UNSPECIFIED.);
#1141=B_SPLINE_CURVE_WITH_KNOTS('',3,(#42746,#42747,#42748,#42749,#42750,
#42751,#42752,#42753,#42754,#42755),.UNSPECIFIED.,.F.,.F.,(4,3,3,4),(0.,
0.5,0.954472009937235,1.),.UNSPECIFIED.);
#1142=B_SPLINE_CURVE_WITH_KNOTS('',3,(#42789,#42790,#42791,#42792,#42793,
#42794,#42795,#42796,#42797,#42798,#42799,#42800,#42801),.UNSPECIFIED.,
 .F.,.F.,(4,2,2,2,2,1,4),(0.,0.00196327068521397,0.00405116683518219,0.00791556264156159,
0.0117816276323522,0.0182150743305803,0.0190236917019835),.UNSPECIFIED.);
#1143=B_SPLINE_CURVE_WITH_KNOTS('',3,(#42802,#42803,#42804,#42805,#42806,
#42807,#42808,#42809,#42810,#42811,#42812,#42813,#42814,#42815),
 .UNSPECIFIED.,.F.,.F.,(4,2,2,2,2,2,4),(0.000139162384345064,0.0024762649742147,
0.00533153906455379,0.00984378785210221,0.0137939163567501,0.0193287305983979,
0.0196872216305737),.UNSPECIFIED.);
#1144=B_SPLINE_CURVE_WITH_KNOTS('',3,(#42817,#42818,#42819,#42820),
 .UNSPECIFIED.,.F.,.F.,(4,4),(8.32473598532599E-11,0.000180393203869309),
 .UNSPECIFIED.);
#1145=B_SPLINE_CURVE_WITH_KNOTS('',3,(#42839,#42840,#42841,#42842,#42843,
#42844,#42845,#42846,#42847,#42848,#42849,#42850,#42851,#42852,#42853,#42854,
#42855,#42856),.UNSPECIFIED.,.F.,.F.,(4,2,2,2,2,2,2,2,4),(0.00769785679708774,
0.00802820462699518,0.00843145134922816,0.00899044509204644,0.0111243442863434,
0.0153131578831398,0.0188817433759505,0.0211457734297869,0.0229957599552858),
 .UNSPECIFIED.);
#1146=B_SPLINE_CURVE_WITH_KNOTS('',3,(#42875,#42876,#42877,#42878,#42879,
#42880,#42881,#42882,#42883,#42884,#42885,#42886,#42887,#42888,#42889,#42890,
#42891),.UNSPECIFIED.,.F.,.F.,(4,2,2,2,2,2,2,1,4),(-0.0060395950713934,
-0.00533643385535489,-0.00457161010811536,-0.00315658316525502,-0.00174099050172359,
-0.00017573884332551,-0.000110297877347887,-7.85738128386753E-5,-2.35863647916582E-5),
 .UNSPECIFIED.);
#1147=B_SPLINE_CURVE_WITH_KNOTS('',3,(#42893,#42894,#42895,#42896,#42897,
#42898,#42899,#42900,#42901,#42902,#42903,#42904,#42905,#42906,#42907),
 .UNSPECIFIED.,.F.,.F.,(4,2,2,2,2,2,1,4),(0.,0.00229368739167764,0.00482687780864931,
0.00907820400782217,0.0132315563727989,0.0189068992119232,0.0192249547905654,
0.0195430103692075),.UNSPECIFIED.);
#1148=B_SPLINE_CURVE_WITH_KNOTS('',3,(#42944,#42945,#42946,#42947,#42948,
#42949,#42950,#42951,#42952,#42953,#42954,#42955,#42956),.UNSPECIFIED.,
 .F.,.F.,(4,2,2,2,2,1,4),(0.,0.00196328295888409,0.00405119382129033,0.00791560040373507,
0.0117816828145636,0.0181787290681755,0.0189003258766864),.UNSPECIFIED.);
#1149=B_SPLINE_CURVE_WITH_KNOTS('',3,(#42957,#42958,#42959,#42960,#42961,
#42962,#42963,#42964,#42965,#42966,#42967,#42968,#42969,#42970,#42971,#42972,
#42973,#42974,#42975,#42976,#42977,#42978),.UNSPECIFIED.,.F.,.F.,(4,2,2,
2,2,2,2,2,2,2,4),(0.000140180528062204,0.00225584941024912,0.00477761261246817,
0.00890918499620693,0.013273463805397,0.015463798412026,0.0165317709770468,
0.0170651823497595,0.0173442289099364,0.0175722509086272,0.0178410054929824),
 .UNSPECIFIED.);
#1150=B_SPLINE_CURVE_WITH_KNOTS('',3,(#42997,#42998,#42999,#43000,#43001,
#43002,#43003,#43004,#43005,#43006,#43007,#43008,#43009,#43010),
 .UNSPECIFIED.,.F.,.F.,(4,2,2,2,2,2,4),(0.,0.00207941973197339,0.00431488716400025,
0.00832511413568298,0.0124961317069963,0.0167503250398471,0.0180491597892712),
 .UNSPECIFIED.);
#1151=B_SPLINE_CURVE_WITH_KNOTS('',3,(#43029,#43030,#43031,#43032,#43033,
#43034,#43035,#43036,#43037,#43038,#43039,#43040,#43041,#43042,#43043,#43044,
#43045,#43046,#43047,#43048,#43049,#43050),.UNSPECIFIED.,.F.,.F.,(4,2,2,
2,2,2,2,2,2,2,4),(-0.00520512896532105,-0.0047254121597404,-0.00384306945129063,
-0.0026259626535781,-0.00135029183013414,-0.000702398299474361,-0.000385625313690802,
-0.000227584692409082,-0.000144536400628624,-7.66530613735417E-5,0.),
 .UNSPECIFIED.);
#1152=B_SPLINE_CURVE_WITH_KNOTS('',3,(#43069,#43070,#43071,#43072,#43073,
#43074,#43075,#43076,#43077,#43078,#43079,#43080,#43081,#43082),
 .UNSPECIFIED.,.F.,.F.,(4,2,2,2,2,2,4),(-0.0149861184273252,-0.0130782901080037,
-0.0110008733235856,-0.00715736810866992,-0.0033122548327467,-5.78553775021709E-7,
0.000656745899211298),.UNSPECIFIED.);
#1153=B_SPLINE_CURVE_WITH_KNOTS('',3,(#43101,#43102,#43103,#43104,#43105,
#43106,#43107,#43108,#43109,#43110,#43111,#43112,#43113,#43114),
 .UNSPECIFIED.,.F.,.F.,(4,2,2,2,2,2,4),(-0.0155094238033158,-0.0134904514688655,
-0.0113307135610571,-0.00736843882793857,-0.00334201943138028,0.,0.000700784549264495),
 .UNSPECIFIED.);
#1154=B_SPLINE_CURVE_WITH_KNOTS('',3,(#43151,#43152,#43153,#43154,#43155,
#43156,#43157),.UNSPECIFIED.,.F.,.F.,(4,3,4),(4.63335483447215E-5,0.576904555942714,
1.),.UNSPECIFIED.);
#1155=B_SPLINE_CURVE_WITH_KNOTS('',3,(#43158,#43159,#43160,#43161,#43162,
#43163,#43164,#43165,#43166,#43167,#43168,#43169,#43170,#43171),
 .UNSPECIFIED.,.F.,.F.,(4,2,2,2,2,2,4),(0.00011713384202571,0.00225864572668593,
0.00478192661937105,0.00891724353890262,0.0128312590854899,0.0167147431913389,
0.017525068949556),.UNSPECIFIED.);
#1156=B_SPLINE_CURVE_WITH_KNOTS('',3,(#43190,#43191,#43192,#43193,#43194,
#43195,#43196,#43197,#43198,#43199,#43200,#43201,#43202,#43203),
 .UNSPECIFIED.,.F.,.F.,(4,2,2,2,2,2,4),(0.,0.00213082043024386,0.00443313724537573,
0.00848007384794817,0.012794220088842,0.0161393809355339,0.0168933269801154),
 .UNSPECIFIED.);
#1157=B_SPLINE_CURVE_WITH_KNOTS('',3,(#43205,#43206,#43207,#43208,#43209,
#43210,#43211,#43212,#43213,#43214,#43215,#43216,#43217,#43218,#43219,#43220,
#43221,#43222,#43223,#43224,#43225,#43226,#43227,#43228,#43229,#43230,#43231,
#43232),.UNSPECIFIED.,.F.,.F.,(4,2,2,2,2,2,2,2,2,2,2,2,2,4),(0.000174134990213334,
0.00187427244956009,0.00396421279048467,0.00796453993799608,0.0131627439566036,
0.0171335149626361,0.0189518130231438,0.0193835279188768,0.0196250377516676,
0.0196751501926279,0.0196996611938061,0.0197117721364523,0.0199235080293271,
0.0203275207337434),.UNSPECIFIED.);
#1158=B_SPLINE_CURVE_WITH_KNOTS('',3,(#43248,#43249,#43250,#43251,#43252,
#43253,#43254,#43255,#43256,#43257,#43258,#43259,#43260,#43261,#43262),
 .UNSPECIFIED.,.F.,.F.,(4,2,2,2,2,2,1,4),(-0.0088943782310824,-0.00781596641048315,
-0.0066515240749629,-0.00449643047488731,-0.00234060802490015,-7.76918320130951E-7,
0.000287494473515859,0.000575765865351848),.UNSPECIFIED.);
#1159=B_SPLINE_CURVE_WITH_KNOTS('',3,(#43278,#43279,#43280,#43281,#43282,
#43283,#43284,#43285,#43286,#43287,#43288,#43289,#43290,#43291),
 .UNSPECIFIED.,.F.,.F.,(4,2,2,2,2,2,4),(-0.0158043920350505,-0.0137354422361253,
-0.0115133073678156,-0.00749815840910723,-0.00334302701322283,-6.298460010698E-7,
0.000722872722575174),.UNSPECIFIED.);
#1160=B_SPLINE_CURVE_WITH_KNOTS('',3,(#43322,#43323,#43324,#43325,#43326,
#43327,#43328,#43329,#43330,#43331,#43332,#43333,#43334,#43335,#43336),
 .UNSPECIFIED.,.F.,.F.,(4,2,2,2,2,2,1,4),(0.,0.0019632699431003,0.00405114150044124,
0.00791493916943235,0.0117801488263792,0.0162003287979513,0.0168797194475004,
0.0175591100970496),.UNSPECIFIED.);
#1161=B_SPLINE_CURVE_WITH_KNOTS('',3,(#43337,#43338,#43339,#43340,#43341,
#43342,#43343,#43344,#43345,#43346,#43347,#43348,#43349),.UNSPECIFIED.,
 .F.,.F.,(4,3,3,3,4),(0.00643398620750897,0.459308200273434,0.500000335643866,
0.949872720004008,0.99999999998043),.UNSPECIFIED.);
#1162=B_SPLINE_CURVE_WITH_KNOTS('',3,(#43351,#43352,#43353,#43354,#43355,
#43356,#43357,#43358,#43359,#43360),.UNSPECIFIED.,.F.,.F.,(4,3,3,4),(0.,
0.451687166473715,0.5,1.),.UNSPECIFIED.);
#1163=B_SPLINE_CURVE_WITH_KNOTS('',3,(#43376,#43377,#43378,#43379,#43380,
#43381,#43382,#43383,#43384,#43385,#43386,#43387,#43388),.UNSPECIFIED.,
 .F.,.F.,(4,3,3,3,4),(6.243301773739E-9,0.452960189921173,0.5,0.953477189168755,
0.993525782404942),.UNSPECIFIED.);
#1164=B_SPLINE_CURVE_WITH_KNOTS('',3,(#43404,#43405,#43406,#43407,#43408,
#43409,#43410,#43411,#43412,#43413,#43414,#43415,#43416,#43417,#43418),
 .UNSPECIFIED.,.F.,.F.,(4,2,2,2,2,2,1,4),(2.13732516168125E-5,0.00196337715740596,
0.00405135866965422,0.00791551885237747,0.0117810712401529,0.0159267936047945,
0.0164430910383506,0.0169593884719067),.UNSPECIFIED.);
#1165=B_SPLINE_CURVE_WITH_KNOTS('',3,(#43420,#43421,#43422,#43423,#43424,
#43425,#43426,#43427,#43428,#43429),.UNSPECIFIED.,.F.,.F.,(4,3,3,4),(4.26803766547994E-9,
0.5,0.948505579092606,1.),.UNSPECIFIED.);
#1166=B_SPLINE_CURVE_WITH_KNOTS('',3,(#43460,#43461,#43462,#43463,#43464,
#43465,#43466,#43467,#43468,#43469,#43470,#43471,#43472,#43473,#43474,#43475),
 .UNSPECIFIED.,.F.,.F.,(4,2,2,2,2,2,2,4),(0.000728504471755486,0.000939141210919874,
0.00177033038102613,0.00320263890334485,0.00692959899102407,0.0107850896424002,
0.0140478837404244,0.0170344679497315),.UNSPECIFIED.);
#1167=B_SPLINE_CURVE_WITH_KNOTS('',3,(#43476,#43477,#43478,#43479,#43480,
#43481,#43482,#43483,#43484,#43485,#43486,#43487,#43488,#43489),
 .UNSPECIFIED.,.F.,.F.,(4,2,2,2,2,2,4),(0.00010160769219427,0.00122102113075305,
0.0025441425093596,0.00564882016696292,0.0110992314938815,0.018557172207377,
0.01940107775831),.UNSPECIFIED.);
#1168=B_SPLINE_CURVE_WITH_KNOTS('',3,(#43505,#43506,#43507,#43508,#43509,
#43510,#43511),.UNSPECIFIED.,.F.,.F.,(4,3,4),(0.,0.649593716766449,0.999996170084436),
 .UNSPECIFIED.);
#1169=B_SPLINE_CURVE_WITH_KNOTS('',3,(#43513,#43514,#43515,#43516,#43517,
#43518,#43519),.UNSPECIFIED.,.F.,.F.,(4,3,4),(0.00152959430806593,0.750813994531579,
0.999868145301564),.UNSPECIFIED.);
#1170=B_SPLINE_CURVE_WITH_KNOTS('',3,(#43521,#43522,#43523,#43524,#43525,
#43526,#43527,#43528,#43529,#43530,#43531,#43532,#43533,#43534,#43535,#43536,
#43537,#43538,#43539,#43540,#43541,#43542,#43543,#43544),.UNSPECIFIED.,
 .F.,.F.,(4,2,2,2,2,2,2,2,2,2,2,4),(0.00204715033410867,0.00214131685417548,
0.00214328334720006,0.00214525441504065,0.00218111916521674,0.00226943891369271,
0.00246440256884611,0.0064636073563424,0.010547188883976,0.0137087254753622,
0.0153157764781132,0.0166006569605146),.UNSPECIFIED.);
#1171=B_SPLINE_CURVE_WITH_KNOTS('',3,(#43546,#43547,#43548,#43549),
 .UNSPECIFIED.,.F.,.F.,(4,4),(6.83292023692837E-9,0.99943821988792),
 .UNSPECIFIED.);
#1172=B_SPLINE_CURVE_WITH_KNOTS('',3,(#43580,#43581,#43582,#43583,#43584,
#43585,#43586,#43587,#43588,#43589,#43590,#43591,#43592,#43593,#43594),
 .UNSPECIFIED.,.F.,.F.,(4,1,2,2,2,2,2,4),(-0.000721085007192466,-0.000360542503596233,
0.,0.00287183524996394,0.00517719429213056,0.00771610262833221,0.009312961775071,
0.0107491030887171),.UNSPECIFIED.);
#1173=B_SPLINE_CURVE_WITH_KNOTS('',3,(#43595,#43596,#43597,#43598,#43599,
#43600,#43601,#43602,#43603,#43604),.UNSPECIFIED.,.F.,.F.,(4,2,2,2,4),(-0.00965817669299273,
-0.0074786447771315,-0.00464773278744681,-0.00179228406875512,0.),
 .UNSPECIFIED.);
#1174=B_SPLINE_CURVE_WITH_KNOTS('',3,(#43606,#43607,#43608,#43609,#43610,
#43611,#43612,#43613,#43614,#43615,#43616,#43617,#43618,#43619,#43620,#43621),
 .UNSPECIFIED.,.F.,.F.,(4,2,2,2,2,2,2,4),(0.0109402855774774,0.0121575085049054,
0.0143534546456024,0.0170434917438361,0.0211697549569896,0.0237315274442865,
0.0248381170476492,0.0251943850241165),.UNSPECIFIED.);
#1175=B_SPLINE_CURVE_WITH_KNOTS('',3,(#43623,#43624,#43625,#43626,#43627,
#43628,#43629,#43630,#43631,#43632,#43633,#43634,#43635,#43636,#43637),
 .UNSPECIFIED.,.F.,.F.,(4,2,2,2,2,2,1,4),(0.000110756842378222,0.00245081867056697,
0.00524680256100879,0.00963989788679471,0.0136782996277394,0.0195995990701057,
0.0204950744567913,0.0213905498434769),.UNSPECIFIED.);
#1176=B_SPLINE_CURVE_WITH_KNOTS('',3,(#43639,#43640,#43641,#43642,#43643,
#43644,#43645,#43646,#43647,#43648,#43649,#43650,#43651,#43652,#43653),
 .UNSPECIFIED.,.F.,.F.,(4,2,2,2,2,2,1,4),(-0.012412672104359,-0.0108466451671881,
-0.00897946215730165,-0.00600237082743812,-0.00331077857606189,-4.09349858813621E-7,
0.000415773934254383,0.000831957218367579),.UNSPECIFIED.);
#1177=B_SPLINE_CURVE_WITH_KNOTS('',3,(#43669,#43670,#43671,#43672,#43673,
#43674,#43675,#43676,#43677,#43678,#43679,#43680,#43681,#43682),
 .UNSPECIFIED.,.F.,.F.,(4,2,2,2,2,2,4),(-0.015078381833914,-0.0131186091331513,
-0.0110344068594359,-0.00717766413762145,-0.00331927009469946,-7.58587308438002E-7,
0.000663174204454999),.UNSPECIFIED.);
#1178=B_SPLINE_CURVE_WITH_KNOTS('',3,(#43713,#43714,#43715,#43716,#43717,
#43718,#43719,#43720,#43721,#43722,#43723,#43724,#43725,#43726,#43727),
 .UNSPECIFIED.,.F.,.F.,(4,1,2,2,2,2,2,4),(-0.000734317183253655,-0.000367158591626828,
0.,0.00295316648201105,0.00537349468880681,0.00803885665043543,0.00971523565928993,
0.0112229190958255),.UNSPECIFIED.);
#1179=B_SPLINE_CURVE_WITH_KNOTS('',3,(#43728,#43729,#43730,#43731,#43732,
#43733,#43734,#43735,#43736,#43737,#43738,#43739,#43740,#43741),
 .UNSPECIFIED.,.F.,.F.,(4,2,2,2,2,2,4),(-0.0126319361261658,-0.0110411624711013,
-0.00932775041915123,-0.00615718988741039,-0.00298521368956833,0.,0.000652693410532094),
 .UNSPECIFIED.);
#1180=B_SPLINE_CURVE_WITH_KNOTS('',3,(#43757,#43758,#43759,#43760,#43761,
#43762,#43763,#43764,#43765,#43766,#43767,#43768,#43769,#43770),
 .UNSPECIFIED.,.F.,.F.,(4,2,2,2,2,2,4),(0.,0.0022508673695075,0.0047447068702816,
0.00880824860212537,0.012793275955846,0.0188290600607819,0.0220919733094374),
 .UNSPECIFIED.);
#1181=B_SPLINE_CURVE_WITH_KNOTS('',3,(#43772,#43773,#43774,#43775,#43776,
#43777,#43778,#43779,#43780,#43781,#43782,#43783,#43784,#43785,#43786),
 .UNSPECIFIED.,.F.,.F.,(4,2,2,2,2,2,1,4),(0.000109583238215975,0.00245093435459509,
0.00524713881000084,0.00964068384981554,0.0136193432454163,0.0194845949868915,
0.0206313249998054,0.0217780550127193),.UNSPECIFIED.);
#1182=B_SPLINE_CURVE_WITH_KNOTS('',3,(#43788,#43789,#43790,#43791,#43792,
#43793,#43794,#43795,#43796,#43797,#43798,#43799,#43800,#43801,#43802),
 .UNSPECIFIED.,.F.,.F.,(4,2,2,2,2,2,1,4),(-0.0125380391583743,-0.0109543469897537,
-0.00906695797544928,-0.00605748119240737,-0.00333652356516311,-3.59896165919374E-7,
0.000420640062250262,0.000841640020666443),.UNSPECIFIED.);
#1183=B_SPLINE_CURVE_WITH_KNOTS('',3,(#43818,#43819,#43820,#43821,#43822,
#43823,#43824,#43825,#43826,#43827,#43828,#43829,#43830,#43831),
 .UNSPECIFIED.,.F.,.F.,(4,2,2,2,2,2,4),(-0.0150733797038266,-0.0131143211030396,
-0.011030859344339,-0.00717556933822455,-0.00331852841954188,-7.25644891112764E-7,
0.000662487949083671),.UNSPECIFIED.);
#1184=B_SPLINE_CURVE_WITH_KNOTS('',3,(#43862,#43863,#43864,#43865,#43866,
#43867,#43868,#43869,#43870,#43871,#43872,#43873,#43874,#43875,#43876),
 .UNSPECIFIED.,.F.,.F.,(4,1,2,2,2,2,2,4),(-0.000741878016633449,-0.000370939008316724,
0.,0.00297259893383558,0.0054147943408359,0.00810416070365053,0.00979566612229234,
0.0113169507490356),.UNSPECIFIED.);
#1185=B_SPLINE_CURVE_WITH_KNOTS('',3,(#43877,#43878,#43879,#43880,#43881,
#43882,#43883,#43884,#43885,#43886,#43887,#43888,#43889,#43890),
 .UNSPECIFIED.,.F.,.F.,(4,2,2,2,2,2,4),(-0.0122871688845248,-0.0107438701097029,
-0.00908257557294534,-0.00600856433681326,-0.00293310884332506,0.,0.000649631234003708),
 .UNSPECIFIED.);
#1186=B_SPLINE_CURVE_WITH_KNOTS('',3,(#43906,#43907,#43908,#43909,#43910,
#43911,#43912,#43913,#43914,#43915,#43916,#43917,#43918,#43919),
 .UNSPECIFIED.,.F.,.F.,(4,2,2,2,2,2,4),(0.,0.00225039966924556,0.00474368416702002,
0.00880685738624697,0.0127791302606063,0.0166740141105481,0.0172515126691911),
 .UNSPECIFIED.);
#1187=B_SPLINE_CURVE_WITH_KNOTS('',3,(#43921,#43922,#43923,#43924,#43925,
#43926,#43927,#43928,#43929,#43930,#43931,#43932,#43933,#43934),
 .UNSPECIFIED.,.F.,.F.,(4,2,2,2,2,2,4),(0.000108721996107286,0.0024509596667275,
0.00524721540031518,0.00964094075402568,0.0135914837293887,0.017507436081882,
0.0180994566480111),.UNSPECIFIED.);
#1188=B_SPLINE_CURVE_WITH_KNOTS('',3,(#43936,#43937,#43938,#43939,#43940,
#43941,#43942,#43943,#43944,#43945,#43946,#43947,#43948,#43949,#43950),
 .UNSPECIFIED.,.F.,.F.,(4,2,2,2,2,2,1,4),(-0.0149129193286548,-0.0129965664222115,
-0.0107134808259071,-0.00707293891052898,-0.00378143624454696,-3.24086999198975E-7,
0.000422829226243187,0.000845982539485573),.UNSPECIFIED.);
#1189=B_SPLINE_CURVE_WITH_KNOTS('',3,(#43966,#43967,#43968,#43969,#43970,
#43971,#43972,#43973,#43974,#43975,#43976,#43977,#43978,#43979),
 .UNSPECIFIED.,.F.,.F.,(4,2,2,2,2,2,4),(-0.0150676149456439,-0.0131093839672474,
-0.0110267844150414,-0.00717316249718917,-0.003317694134226,-6.91760243556189E-7,
0.000661693396741128),.UNSPECIFIED.);
#1190=B_SPLINE_CURVE_WITH_KNOTS('',3,(#44010,#44011,#44012,#44013,#44014,
#44015,#44016,#44017,#44018,#44019,#44020,#44021,#44022,#44023,#44024),
 .UNSPECIFIED.,.F.,.F.,(4,1,2,2,2,2,2,4),(-0.000740226615683101,-0.00037011330784155,
0.,0.00296825453891254,0.00540526633452328,0.008088977356173,0.00977702223183042,
0.0112951461282497),.UNSPECIFIED.);
#1191=B_SPLINE_CURVE_WITH_KNOTS('',3,(#44025,#44026,#44027,#44028,#44029,
#44030,#44031,#44032,#44033,#44034,#44035,#44036,#44037,#44038),
 .UNSPECIFIED.,.F.,.F.,(4,2,2,2,2,2,4),(-0.011254734338536,-0.00985313094765622,
-0.00834524071717542,-0.00555519590875847,-0.0027637664637976,0.,0.000645994893972402),
 .UNSPECIFIED.);
#1192=B_SPLINE_CURVE_WITH_KNOTS('',3,(#44054,#44055,#44056,#44057,#44058,
#44059,#44060,#44061,#44062,#44063,#44064,#44065,#44066,#44067),
 .UNSPECIFIED.,.F.,.F.,(4,2,2,2,2,2,4),(0.,0.00224971467737683,0.00474217676161104,
0.008804821918669,0.0127594425323947,0.018558425141178,0.0211568201917662),
 .UNSPECIFIED.);
#1193=B_SPLINE_CURVE_WITH_KNOTS('',3,(#44069,#44070,#44071,#44072,#44073,
#44074,#44075,#44076,#44077,#44078,#44079,#44080,#44081,#44082),
 .UNSPECIFIED.,.F.,.F.,(4,2,2,2,2,2,4),(0.000107838954687328,0.00245083687006141,
0.00524686551857072,0.00964032925791452,0.0136011718567849,0.0196371711489655,
0.0229339743667445),.UNSPECIFIED.);
#1194=B_SPLINE_CURVE_WITH_KNOTS('',3,(#44084,#44085,#44086,#44087,#44088,
#44089,#44090,#44091,#44092,#44093,#44094,#44095,#44096,#44097,#44098),
 .UNSPECIFIED.,.F.,.F.,(4,2,2,2,2,2,1,4),(-0.014939291320971,-0.0130188828362878,
-0.0107316995046581,-0.00708448598111002,-0.00378695827246614,-2.83689470114909E-7,
0.000425980206607165,0.000852244102684445),.UNSPECIFIED.);
#1195=B_SPLINE_CURVE_WITH_KNOTS('',3,(#44114,#44115,#44116,#44117,#44118,
#44119,#44120,#44121,#44122,#44123,#44124,#44125,#44126,#44127),
 .UNSPECIFIED.,.F.,.F.,(4,2,2,2,2,2,4),(-0.0150614059516756,-0.0131040689956594,
-0.0110224033904192,-0.00717057369300718,-0.00331680728711196,-6.58184886700303E-7,
0.000660833663601821),.UNSPECIFIED.);
#1196=B_SPLINE_CURVE_WITH_KNOTS('',3,(#44158,#44159,#44160,#44161,#44162,
#44163,#44164,#44165,#44166,#44167,#44168,#44169,#44170,#44171,#44172),
 .UNSPECIFIED.,.F.,.F.,(4,1,2,2,2,2,2,4),(-0.000691739067306629,-0.000345856578478131,
2.59103503667726E-8,0.0027975315775318,0.00501871624556568,0.00746569969276276,
0.00900487309295416,0.0103889571762724),.UNSPECIFIED.);
#1197=B_SPLINE_CURVE_WITH_KNOTS('',3,(#44173,#44174,#44175,#44176,#44177,
#44178,#44179,#44180,#44181,#44182,#44183,#44184,#44185),.UNSPECIFIED.,
 .F.,.F.,(4,2,2,2,2,1,4),(3.16211434698517E-5,0.00196343737821928,0.00405149290676457,
0.00791568419994298,0.0117813340088185,0.0182067510991605,0.0189937367781405),
 .UNSPECIFIED.);
#1198=B_SPLINE_CURVE_WITH_KNOTS('',3,(#44201,#44202,#44203,#44204,#44205,
#44206,#44207,#44208,#44209,#44210,#44211,#44212,#44213,#44214,#44215),
 .UNSPECIFIED.,.F.,.F.,(4,2,2,2,2,2,1,4),(0.,0.00225539508390829,0.0047551224758348,
0.00882290010525813,0.012929760761633,0.0189658855667421,0.0197228197031485,
0.0204797538395548),.UNSPECIFIED.);
#1199=B_SPLINE_CURVE_WITH_KNOTS('',3,(#44217,#44218,#44219,#44220,#44221,
#44222,#44223,#44224,#44225,#44226,#44227,#44228,#44229,#44230,#44231),
 .UNSPECIFIED.,.F.,.F.,(4,2,2,2,2,2,1,4),(0.000114847568641728,0.00244997042572085,
0.00524435790927852,0.00963463871755652,0.0137272589487558,0.01978697300403,
0.0205522261776815,0.021317479351333),.UNSPECIFIED.);
#1200=B_SPLINE_CURVE_WITH_KNOTS('',3,(#44233,#44234,#44235,#44236,#44237,
#44238,#44239,#44240,#44241,#44242,#44243,#44244,#44245,#44246,#44247),
 .UNSPECIFIED.,.F.,.F.,(4,2,2,2,2,2,1,4),(-0.0118947324656203,-0.0104010198964424,
-0.00861751596243538,-0.00577422353032262,-0.00320311792038097,-6.29187275549489E-7,
0.000394523774615498,0.000789676736506546),.UNSPECIFIED.);
#1201=B_SPLINE_CURVE_WITH_KNOTS('',3,(#44263,#44264,#44265,#44266,#44267,
#44268,#44269,#44270,#44271,#44272,#44273,#44274,#44275),.UNSPECIFIED.,
 .F.,.F.,(4,2,2,2,2,1,4),(0.,0.0019634605910373,0.00405154255300626,0.00791565857793337,
0.0117812104822195,0.0156720023551305,0.0157373790506278),.UNSPECIFIED.);
#1202=B_SPLINE_CURVE_WITH_KNOTS('',3,(#44306,#44307,#44308,#44309,#44310,
#44311,#44312,#44313,#44314,#44315,#44316,#44317,#44318,#44319,#44320),
 .UNSPECIFIED.,.F.,.F.,(4,1,2,2,2,2,2,4),(-0.000763541080028175,-0.000381770540014087,
0.,0.0030327047674076,0.00554422819304898,0.00830974549903936,0.0100492407392823,
0.0116136695759151),.UNSPECIFIED.);
#1203=B_SPLINE_CURVE_WITH_KNOTS('',3,(#44321,#44322,#44323,#44324,#44325,
#44326,#44327,#44328,#44329,#44330,#44331,#44332,#44333,#44334,#44335),
 .UNSPECIFIED.,.F.,.F.,(4,2,2,2,2,2,1,4),(-0.0133315230507839,-0.011640861096409,
-0.009824081620331,-0.00646273446012228,-0.0030995729707021,0.,0.000318751292783897,
0.000637502585567794),.UNSPECIFIED.);
#1204=B_SPLINE_CURVE_WITH_KNOTS('',3,(#44351,#44352,#44353,#44354,#44355,
#44356,#44357,#44358,#44359,#44360,#44361,#44362,#44363,#44364,#44365),
 .UNSPECIFIED.,.F.,.F.,(4,2,2,2,2,2,1,4),(0.,0.0022461630475493,0.00473421914177116,
0.0087940687030795,0.0126718295068081,0.01772896307951,0.0182910875229529,
0.0188532119663958),.UNSPECIFIED.);
#1205=B_SPLINE_CURVE_WITH_KNOTS('',3,(#44367,#44368,#44369,#44370,#44371,
#44372,#44373,#44374,#44375,#44376,#44377,#44378,#44379,#44380,#44381),
 .UNSPECIFIED.,.F.,.F.,(4,2,2,2,2,2,1,4),(0.000106100181661028,0.00245103004290281,
0.00524743088659168,0.00964166827403447,0.0135194054565417,0.0188461184288979,
0.0191995608126034,0.019553003196309),.UNSPECIFIED.);
#1206=B_SPLINE_CURVE_WITH_KNOTS('',3,(#44383,#44384,#44385,#44386,#44387,
#44388,#44389,#44390,#44391,#44392,#44393,#44394,#44395,#44396,#44397),
 .UNSPECIFIED.,.F.,.F.,(4,2,2,2,2,2,1,4),(-0.0150589537599889,-0.0131215304824762,
-0.010815435264458,-0.00713770971273073,-0.00381261252897884,-1.7897945260581E-7,
0.000439962560525125,0.000880104100502855),.UNSPECIFIED.);
#1207=B_SPLINE_CURVE_WITH_KNOTS('',3,(#44413,#44414,#44415,#44416,#44417,
#44418,#44419,#44420,#44421,#44422,#44423,#44424,#44425,#44426),
 .UNSPECIFIED.,.F.,.F.,(4,2,2,2,2,2,4),(-0.0150490520073303,-0.0130934976202166,
-0.011013693455221,-0.00716543230475343,-0.0033150490758814,-5.96494445290544E-7,
0.000659105180738562),.UNSPECIFIED.);
#1208=B_SPLINE_CURVE_WITH_KNOTS('',3,(#44460,#44461,#44462,#44463,#44464,
#44465,#44466,#44467,#44468,#44469),.UNSPECIFIED.,.F.,.F.,(4,3,3,4),(4.76676660675416E-11,
0.458512147724096,0.5,0.99999948372105),.UNSPECIFIED.);
#1209=B_SPLINE_CURVE_WITH_KNOTS('',3,(#44470,#44471,#44472,#44473,#44474,
#44475,#44476,#44477,#44478,#44479,#44480,#44481,#44482,#44483,#44484,#44485,
#44486),.UNSPECIFIED.,.F.,.F.,(4,2,2,2,2,2,2,1,4),(4.25743825136903E-5,
0.00196427209076551,0.00405327225761388,0.00791819907389034,0.0117846711271358,
0.0158752614297264,0.0160346040583549,0.016109286249132,0.0162294355263165),
 .UNSPECIFIED.);
#1210=B_SPLINE_CURVE_WITH_KNOTS('',3,(#44505,#44506,#44507,#44508,#44509,
#44510,#44511,#44512,#44513,#44514,#44515,#44516,#44517,#44518,#44519),
 .UNSPECIFIED.,.F.,.F.,(4,2,2,2,2,2,1,4),(0.,0.00229420957926068,0.00482817002974407,
0.00908036440822177,0.0133874783015933,0.0196108582088963,0.0205947571667744,
0.0215786561246526),.UNSPECIFIED.);
#1211=B_SPLINE_CURVE_WITH_KNOTS('',3,(#44521,#44522,#44523,#44524,#44525,
#44526,#44527,#44528,#44529,#44530,#44531,#44532,#44533,#44534,#44535),
 .UNSPECIFIED.,.F.,.F.,(4,2,2,2,2,2,1,4),(0.000136707832181995,0.00249232514602642,
0.00536880437866845,0.00990130746918292,0.0138102490017995,0.0191471415464468,
0.0195724563892528,0.0199977712320588),.UNSPECIFIED.);
#1212=B_SPLINE_CURVE_WITH_KNOTS('',3,(#44537,#44538,#44539,#44540,#44541,
#44542,#44543,#44544,#44545,#44546,#44547,#44548,#44549,#44550,#44551,#44552,
#44553,#44554,#44555,#44556,#44557,#44558,#44559,#44560,#44561,#44562,#44563,
#44564),.UNSPECIFIED.,.F.,.F.,(4,2,2,2,2,2,2,2,2,2,2,2,2,4),(0.00898954517258166,
0.00914281246490069,0.00915480318218891,0.00916394223308905,0.009170539070818,
0.00917512298254225,0.00934376075639942,0.00993773086056826,0.0107255979885816,
0.0140390495835903,0.0203898888919342,0.0258014279076157,0.0292347438173574,
0.0320432823289119),.UNSPECIFIED.);
#1213=B_SPLINE_CURVE_WITH_KNOTS('',3,(#44583,#44584,#44585,#44586,#44587,
#44588,#44589,#44590,#44591,#44592,#44593,#44594,#44595),.UNSPECIFIED.,
 .F.,.F.,(4,2,2,2,2,1,4),(0.,0.00196326831438807,0.00405116172141169,0.00791555685180518,
0.0117816204128086,0.0182121807887324,0.0190127006546827),.UNSPECIFIED.);
#1214=B_SPLINE_CURVE_WITH_KNOTS('',3,(#44629,#44630,#44631,#44632,#44633,
#44634,#44635,#44636,#44637,#44638,#44639,#44640,#44641,#44642,#44643),
 .UNSPECIFIED.,.F.,.F.,(4,1,2,2,2,2,2,4),(-0.000734686664483305,-0.000367343332241652,
0.,0.00295428728510061,0.005375468594744,0.00804183895503185,0.00971909263264639,
0.0112274500128319),.UNSPECIFIED.);
#1215=B_SPLINE_CURVE_WITH_KNOTS('',3,(#44644,#44645,#44646,#44647,#44648,
#44649,#44650,#44651,#44652,#44653,#44654,#44655,#44656,#44657),
 .UNSPECIFIED.,.F.,.F.,(4,2,2,2,2,2,4),(-0.0111679813135756,-0.00977782326874345,
-0.00828321187638799,-0.0055178304310841,-0.00275101805988158,0.,0.000641924036864499),
 .UNSPECIFIED.);
#1216=B_SPLINE_CURVE_WITH_KNOTS('',3,(#44673,#44674,#44675,#44676,#44677,
#44678,#44679,#44680,#44681,#44682,#44683,#44684,#44685,#44686),
 .UNSPECIFIED.,.F.,.F.,(4,2,2,2,2,2,4),(0.,0.00224862323800864,0.00473974267430908,
0.00880152583573068,0.0127307468244572,0.0182732791623988,0.0204025687641099),
 .UNSPECIFIED.);
#1217=B_SPLINE_CURVE_WITH_KNOTS('',3,(#44688,#44689,#44690,#44691,#44692,
#44693,#44694,#44695,#44696,#44697,#44698,#44699,#44700,#44701,#44702),
 .UNSPECIFIED.,.F.,.F.,(4,2,2,2,2,2,1,4),(0.000107182900594769,0.0024506374855744,
0.00524629582418313,0.00963926824962338,0.0136265182058118,0.0194869643633496,
0.0205771760420138,0.021667387720678),.UNSPECIFIED.);
#1218=B_SPLINE_CURVE_WITH_KNOTS('',3,(#44704,#44705,#44706,#44707,#44708,
#44709,#44710,#44711,#44712,#44713,#44714,#44715,#44716,#44717,#44718),
 .UNSPECIFIED.,.F.,.F.,(4,2,2,2,2,2,1,4),(-0.0149775721862555,-0.0130517244210142,
-0.0107585030750918,-0.00710150465772868,-0.00379514746711448,-2.39497760071844E-7,
0.000430503915153775,0.000861247328067622),.UNSPECIFIED.);
#1219=B_SPLINE_CURVE_WITH_KNOTS('',3,(#44734,#44735,#44736,#44737,#44738,
#44739,#44740,#44741,#44742,#44743,#44744,#44745,#44746,#44747),
 .UNSPECIFIED.,.F.,.F.,(4,2,2,2,2,2,4),(-0.0150554445787514,-0.0130989671617,
-0.0110181991831687,-0.00716809080361883,-0.00331595685734504,-6.27284798819516E-7,
0.000660002856751512),.UNSPECIFIED.);
#1220=B_SPLINE_CURVE_WITH_KNOTS('',3,(#44778,#44779,#44780,#44781,#44782,
#44783,#44784,#44785,#44786,#44787,#44788,#44789,#44790,#44791,#44792),
 .UNSPECIFIED.,.F.,.F.,(4,1,2,2,2,2,2,4),(-0.000705657006003329,-0.000352824269207572,
8.46758818422687E-9,0.00283187350914316,0.00509218516814216,0.00758124097390481,
0.00914657677669795,0.0105544503558209),.UNSPECIFIED.);
#1221=B_SPLINE_CURVE_WITH_KNOTS('',3,(#44793,#44794,#44795,#44796),
 .UNSPECIFIED.,.F.,.F.,(4,4),(2.52662111139725E-7,0.000156519894285502),
 .UNSPECIFIED.);
#1222=B_SPLINE_CURVE_WITH_KNOTS('',3,(#44842,#44843,#44844,#44845,#44846,
#44847,#44848),.UNSPECIFIED.,.F.,.F.,(4,3,4),(0.,8.0731985910313E-5,0.000184468015134139),
 .UNSPECIFIED.);
#1223=B_SPLINE_CURVE_WITH_KNOTS('',3,(#44850,#44851,#44852,#44853,#44854,
#44855,#44856,#44857,#44858,#44859,#44860,#44861,#44862,#44863,#44864),
 .UNSPECIFIED.,.F.,.F.,(4,2,2,2,2,2,1,4),(0.000111698808826464,0.00245119018910623,
0.00524786599351128,0.00964187816046448,0.0136789300227376,0.0195975813525889,
0.0204982843709798,0.0213989873893708),.UNSPECIFIED.);
#1224=B_SPLINE_CURVE_WITH_KNOTS('',3,(#44866,#44867,#44868,#44869,#44870,
#44871,#44872,#44873,#44874,#44875,#44876,#44877,#44878,#44879,#44880),
 .UNSPECIFIED.,.F.,.F.,(4,2,2,2,2,2,1,4),(-0.0121689856441338,-0.0106303509242525,
-0.00879541739039853,-0.00587521095579035,-0.00324935971193159,-5.94103874715715E-7,
0.000405611248584354,0.000811816601043423),.UNSPECIFIED.);
#1225=B_SPLINE_CURVE_WITH_KNOTS('',3,(#44896,#44897,#44898,#44899,#44900,
#44901,#44902,#44903,#44904,#44905,#44906,#44907,#44908),.UNSPECIFIED.,
 .F.,.F.,(4,2,2,2,2,1,4),(-0.00734641636438769,-0.00650314695269393,-0.00560634882285633,
-0.00394680380774528,-0.00228661105698405,-4.0314916701506E-7,4.49899914394729E-5),
 .UNSPECIFIED.);
#1226=B_SPLINE_CURVE_WITH_KNOTS('',3,(#44939,#44940,#44941,#44942,#44943,
#44944,#44945,#44946,#44947,#44948,#44949,#44950,#44951,#44952,#44953),
 .UNSPECIFIED.,.F.,.F.,(4,1,2,2,2,2,2,4),(-0.000701295402296016,-0.000350641164626568,
1.30730428811931E-8,0.00282096645904851,0.00506882011954181,0.00754443484759998,
0.00910140169713002,0.0105016764816241),.UNSPECIFIED.);
#1227=B_SPLINE_CURVE_WITH_KNOTS('',3,(#44954,#44955,#44956,#44957),
 .UNSPECIFIED.,.F.,.F.,(4,4),(2.63661137154546E-7,0.000156519267932661),
 .UNSPECIFIED.);
#1228=B_SPLINE_CURVE_WITH_KNOTS('',3,(#45003,#45004,#45005,#45006,#45007,
#45008,#45009),.UNSPECIFIED.,.F.,.F.,(4,3,4),(0.,0.000143865342517527,0.000184570540086384),
 .UNSPECIFIED.);
#1229=B_SPLINE_CURVE_WITH_KNOTS('',3,(#45011,#45012,#45013,#45014,#45015,
#45016,#45017,#45018,#45019,#45020,#45021,#45022,#45023,#45024,#45025),
 .UNSPECIFIED.,.F.,.F.,(4,2,2,2,2,2,1,4),(0.000112557705947448,0.00245085244664319,
0.00524689426873268,0.0096398676966151,0.0136952476221313,0.0196544422019704,
0.0205060043367664,0.0213575664715625),.UNSPECIFIED.);
#1230=B_SPLINE_CURVE_WITH_KNOTS('',3,(#45027,#45028,#45029,#45030,#45031,
#45032,#45033,#45034,#45035,#45036,#45037,#45038,#45039,#45040,#45041),
 .UNSPECIFIED.,.F.,.F.,(4,2,2,2,2,2,1,4),(-0.011944752020003,-0.0104366177918527,
-0.00863786788440518,-0.00577558334657159,-0.00320190562003143,-6.11066602646329E-7,
0.000396248533472148,0.000793108133546943),.UNSPECIFIED.);
#1231=B_SPLINE_CURVE_WITH_KNOTS('',3,(#45057,#45058,#45059,#45060,#45061,
#45062,#45063,#45064,#45065,#45066,#45067,#45068,#45069),.UNSPECIFIED.,
 .F.,.F.,(4,2,2,2,2,1,4),(-0.00909175237345571,-0.00802830991517297,-0.00689736354987959,
-0.00480451655714594,-0.00271085651475671,-4.46707455368026E-7,5.80232275783389E-5),
 .UNSPECIFIED.);
#1232=B_SPLINE_CURVE_WITH_KNOTS('',3,(#45100,#45101,#45102,#45103,#45104,
#45105,#45106,#45107,#45108,#45109,#45110,#45111,#45112,#45113,#45114),
 .UNSPECIFIED.,.F.,.F.,(4,1,2,2,2,2,2,4),(-0.000694944197987434,-0.000347462280626568,
1.96367342977484E-8,0.00280536701289039,0.00503556246214006,0.00749203226490682,
0.00903705415467283,0.0104265061881677),.UNSPECIFIED.);
#1233=B_SPLINE_CURVE_WITH_KNOTS('',3,(#45115,#45116,#45117,#45118,#45119,
#45120,#45121,#45122,#45123,#45124,#45125,#45126,#45127),.UNSPECIFIED.,
 .F.,.F.,(4,2,2,2,2,1,4),(-0.00115302603191237,-0.00103082771804171,-0.000898911217383983,
-0.000654785644988868,-0.000410565788246101,0.,6.52261959239386E-5),
 .UNSPECIFIED.);
#1234=B_SPLINE_CURVE_WITH_KNOTS('',3,(#45143,#45144,#45145,#45146,#45147,
#45148,#45149,#45150,#45151,#45152,#45153,#45154,#45155,#45156,#45157),
 .UNSPECIFIED.,.F.,.F.,(4,2,2,2,2,2,1,4),(0.,0.00225413674326502,0.00475206800918924,
0.00881838664702737,0.0128986238151764,0.0188615545702435,0.0196792162708141,
0.0204968779713847),.UNSPECIFIED.);
#1235=B_SPLINE_CURVE_WITH_KNOTS('',3,(#45159,#45160,#45161,#45162,#45163,
#45164,#45165,#45166,#45167,#45168,#45169,#45170,#45171,#45172,#45173),
 .UNSPECIFIED.,.F.,.F.,(4,2,2,2,2,2,1,4),(0.000113387852022085,0.00245050920907356,
0.00524590629665468,0.00963782864983612,0.0137251491146221,0.0197690904467667,
0.0205469566713966,0.0213248228960264),.UNSPECIFIED.);
#1236=B_SPLINE_CURVE_WITH_KNOTS('',3,(#45175,#45176,#45177,#45178,#45179,
#45180,#45181,#45182,#45183,#45184,#45185,#45186,#45187,#45188,#45189),
 .UNSPECIFIED.,.F.,.F.,(4,2,2,2,2,2,1,4),(-0.0119786407496759,-0.0104721508238425,
-0.00867539394979939,-0.00581086664521615,-0.00322028623970441,-6.01136300057425E-7,
0.000398005967340617,0.000796613070981292),.UNSPECIFIED.);
#1237=B_SPLINE_CURVE_WITH_KNOTS('',3,(#45205,#45206,#45207,#45208,#45209,
#45210,#45211,#45212,#45213,#45214,#45215,#45216,#45217),.UNSPECIFIED.,
 .F.,.F.,(4,2,2,2,2,1,4),(-0.0156746082238113,-0.0137108816572334,-0.0116225064475064,
-0.00775789938403069,-0.00389180253681144,-3.19960164023303E-7,6.49564316540085E-5),
 .UNSPECIFIED.);
#1238=B_SPLINE_CURVE_WITH_KNOTS('',3,(#45248,#45249,#45250,#45251,#45252,
#45253,#45254,#45255,#45256,#45257,#45258,#45259,#45260,#45261,#45262),
 .UNSPECIFIED.,.F.,.F.,(4,1,2,2,2,2,2,4),(-0.000698046171675193,-0.000349014683457108,
1.68047609766433E-8,0.00281280649313789,0.00505118485493888,0.00751684215155518,
0.00906767756137545,0.0104623198843236),.UNSPECIFIED.);
#1239=B_SPLINE_CURVE_WITH_KNOTS('',3,(#45263,#45264,#45265,#45266,#45267,
#45268,#45269,#45270,#45271,#45272,#45273,#45274,#45275),.UNSPECIFIED.,
 .F.,.F.,(4,2,2,2,2,1,4),(3.0391652138187E-5,0.00196345031052539,0.00405152254689268,
0.00791573701057382,0.0117814265638152,0.0182103569252899,0.0190067212118065),
 .UNSPECIFIED.);
#1240=B_SPLINE_CURVE_WITH_KNOTS('',3,(#45291,#45292,#45293,#45294,#45295,
#45296,#45297,#45298,#45299,#45300),.UNSPECIFIED.,.F.,.F.,(4,3,3,4),(5.32625458252635E-7,
0.5,0.949950994221564,1.),.UNSPECIFIED.);
#1241=B_SPLINE_CURVE_WITH_KNOTS('',3,(#45302,#45303,#45304,#45305,#45306,
#45307,#45308,#45309,#45310,#45311,#45312,#45313,#45314,#45315,#45316),
 .UNSPECIFIED.,.F.,.F.,(4,2,2,2,2,2,1,4),(0.000114161305703342,0.00245028339395967,
0.00524525789255604,0.00963648905518044,0.0136996265586751,0.0196783118744954,
0.0205098152580543,0.0213413186416131),.UNSPECIFIED.);
#1242=B_SPLINE_CURVE_WITH_KNOTS('',3,(#45318,#45319,#45320,#45321,#45322,
#45323,#45324,#45325,#45326,#45327,#45328,#45329,#45330,#45331,#45332),
 .UNSPECIFIED.,.F.,.F.,(4,2,2,2,2,2,1,4),(-0.0112033757935951,-0.00984002274620014,
-0.00821566493097737,-0.00559369133845644,-0.00314184043085325,-6.63547733275108E-7,
0.000380127551360547,0.000760918650454369),.UNSPECIFIED.);
#1243=B_SPLINE_CURVE_WITH_KNOTS('',3,(#45348,#45349,#45350,#45351,#45352,
#45353,#45354,#45355,#45356,#45357,#45358,#45359,#45360,#45361),
 .UNSPECIFIED.,.F.,.F.,(4,2,2,2,2,2,4),(0.,0.00196294041915341,0.0040504787236346,
0.00791353350279755,0.0117780719871774,0.0183010045113864,0.0194590076073073),
 .UNSPECIFIED.);
#1244=B_SPLINE_CURVE_WITH_KNOTS('',3,(#45395,#45396,#45397,#45398,#45399,
#45400,#45401,#45402,#45403,#45404),.UNSPECIFIED.,.F.,.F.,(4,3,3,4),(6.40907306791326E-11,
0.458515632471353,0.5,0.999999486493091),.UNSPECIFIED.);
#1245=B_SPLINE_CURVE_WITH_KNOTS('',3,(#45405,#45406,#45407,#45408,#45409,
#45410,#45411,#45412,#45413,#45414,#45415,#45416,#45417,#45418,#45419,#45420,
#45421),.UNSPECIFIED.,.F.,.F.,(4,2,2,2,2,2,2,1,4),(-0.00582306471465524,
-0.00514676617698311,-0.00441095358738275,-0.00304960117926079,-0.00168770449944653,
-0.000171851700537288,-0.000107756089167128,-7.67827602927109E-5,-2.33062135913729E-5),
 .UNSPECIFIED.);
#1246=B_SPLINE_CURVE_WITH_KNOTS('',3,(#45440,#45441,#45442,#45443,#45444,
#45445,#45446,#45447,#45448,#45449,#45450,#45451,#45452,#45453,#45454),
 .UNSPECIFIED.,.F.,.F.,(4,2,2,2,2,2,1,4),(0.,0.00229369021876058,0.00482688557884032,
0.00907821922334884,0.0132316982713349,0.0189081068967721,0.0192243067083783,
0.0195405065199846),.UNSPECIFIED.);
#1247=B_SPLINE_CURVE_WITH_KNOTS('',3,(#45456,#45457,#45458,#45459,#45460,
#45461,#45462,#45463,#45464,#45465,#45466,#45467,#45468,#45469),
 .UNSPECIFIED.,.F.,.F.,(4,2,2,2,2,2,4),(0.000139385723503641,0.00249232539405233,
0.00536879945512003,0.00990126583114861,0.013826095010537,0.0193135105629825,
0.0197181924043684),.UNSPECIFIED.);
#1248=B_SPLINE_CURVE_WITH_KNOTS('',3,(#45471,#45472,#45473,#45474,#45475,
#45476,#45477),.UNSPECIFIED.,.F.,.F.,(4,3,4),(1.38512065397935E-6,0.0001113045099149,
0.000205256311026677),.UNSPECIFIED.);
#1249=B_SPLINE_CURVE_WITH_KNOTS('',3,(#45496,#45497,#45498,#45499,#45500,
#45501,#45502,#45503,#45504,#45505,#45506,#45507,#45508,#45509),
 .UNSPECIFIED.,.F.,.F.,(4,2,2,2,2,2,4),(0.,0.0019632705087533,0.00405116647296006,
0.00791556217502423,0.0117816273183626,0.0182744236276762,0.019285136254072),
 .UNSPECIFIED.);
#1250=B_SPLINE_CURVE_WITH_KNOTS('',3,(#45546,#45547,#45548,#45549,#45550,
#45551,#45552,#45553,#45554,#45555,#45556,#45557,#45558,#45559,#45560),
 .UNSPECIFIED.,.F.,.F.,(4,2,2,2,2,2,1,4),(0.,0.0020229803815632,0.00418692089039347,
0.00815726963453743,0.0121915813971656,0.0166403965411901,0.017358260390738,
0.0180761242402859),.UNSPECIFIED.);
#1251=B_SPLINE_CURVE_WITH_KNOTS('',3,(#45561,#45562,#45563,#45564,#45565,
#45566,#45567,#45568,#45569,#45570,#45571,#45572,#45573,#45574),
 .UNSPECIFIED.,.F.,.F.,(4,2,2,2,2,2,4),(4.62436974762622E-5,0.00196401966885003,
0.00405275852979369,0.00791719712913681,0.0117832769425412,0.0151123677737135,
0.0157730744381205),.UNSPECIFIED.);
#1252=B_SPLINE_CURVE_WITH_KNOTS('',3,(#45593,#45594,#45595,#45596,#45597,
#45598,#45599,#45600,#45601,#45602,#45603,#45604,#45605,#45606),
 .UNSPECIFIED.,.F.,.F.,(4,2,2,2,2,2,4),(-0.0158607099539636,-0.0137795764643132,
-0.0115422026804368,-0.00752912881153854,-0.0033549345003105,0.,0.000732369038597041),
 .UNSPECIFIED.);
#1253=B_SPLINE_CURVE_WITH_KNOTS('',3,(#45625,#45626,#45627,#45628,#45629,
#45630,#45631,#45632,#45633,#45634,#45635,#45636,#45637,#45638,#45639,#45640,
#45641,#45642,#45643,#45644,#45645,#45646),.UNSPECIFIED.,.F.,.F.,(4,2,2,
2,2,2,2,2,2,2,4),(0.000142338524652503,0.00184865257695027,0.00498757950643991,
0.00931561943583813,0.0138531791463855,0.0161575781939442,0.0172842269029924,
0.0178463672894087,0.018141812938064,0.0183816429813561,0.0186440263445286),
 .UNSPECIFIED.);
#1254=B_SPLINE_CURVE_WITH_KNOTS('',3,(#45665,#45666,#45667,#45668,#45669,
#45670,#45671,#45672,#45673,#45674,#45675,#45676,#45677,#45678,#45679,#45680,
#45681,#45682,#45683,#45684,#45685,#45686),.UNSPECIFIED.,.F.,.F.,(4,2,2,
2,2,2,2,2,2,2,4),(-0.0068296052231379,-0.00597794006538437,-0.00496179891473326,
-0.00329714673454892,-0.00111628877984325,-0.000579964236240451,-0.000316955826123173,
-0.00017927861012683,-0.000102681547137399,-5.83428845580563E-5,0.),
 .UNSPECIFIED.);
#1255=B_SPLINE_CURVE_WITH_KNOTS('',3,(#45705,#45706,#45707,#45708,#45709,
#45710,#45711,#45712,#45713,#45714,#45715,#45716,#45717),.UNSPECIFIED.,
 .F.,.F.,(4,2,2,2,2,1,4),(-0.0016025831250653,-0.0014296062846439,-0.00124564901181184,
-0.000905171694053628,-0.000564546716948114,0.,6.55513366705103E-5),
 .UNSPECIFIED.);
#1256=B_SPLINE_CURVE_WITH_KNOTS('',3,(#45751,#45752,#45753,#45754,#45755,
#45756,#45757,#45758,#45759,#45760,#45761,#45762,#45763,#45764),
 .UNSPECIFIED.,.F.,.F.,(4,2,2,2,2,2,4),(0.,0.00204631942275302,0.00424282204863565,
0.0082900825930658,0.0124353698077687,0.015775425206853,0.0164871129587233),
 .UNSPECIFIED.);
#1257=B_SPLINE_CURVE_WITH_KNOTS('',3,(#45765,#45766,#45767,#45768,#45769,
#45770,#45771,#45772,#45773,#45774,#45775,#45776,#45777,#45778,#45779),
 .UNSPECIFIED.,.F.,.F.,(4,2,2,2,2,2,1,4),(3.00484944896589E-5,0.00196306173968375,
0.00405067439867342,0.00791436594380513,0.011779298111804,0.0156048294251666,
0.0159903174909155,0.0163758055566643),.UNSPECIFIED.);
#1258=B_SPLINE_CURVE_WITH_KNOTS('',3,(#45795,#45796,#45797,#45798,#45799,
#45800,#45801,#45802,#45803,#45804,#45805,#45806,#45807,#45808),
 .UNSPECIFIED.,.F.,.F.,(4,2,2,2,2,2,4),(-0.00167205754200539,-0.0014878923674375,
-0.00128888885938142,-0.000939159922998387,-0.000566173695576969,0.,7.3929919955415E-5),
 .UNSPECIFIED.);
#1259=B_SPLINE_CURVE_WITH_KNOTS('',3,(#45824,#45825,#45826,#45827,#45828,
#45829,#45830,#45831,#45832,#45833,#45834,#45835,#45836,#45837),
 .UNSPECIFIED.,.F.,.F.,(4,2,2,2,2,2,4),(0.000118272099701553,0.00232295608069569,
0.00497082584063325,0.00927746644325167,0.0133382712947269,0.0174273312026365,
0.0182983902025005),.UNSPECIFIED.);
#1260=B_SPLINE_CURVE_WITH_KNOTS('',3,(#45853,#45854,#45855,#45856),
 .UNSPECIFIED.,.F.,.F.,(4,4),(0.00559373542229181,0.999482228601385),
 .UNSPECIFIED.);
#1261=B_SPLINE_CURVE_WITH_KNOTS('',3,(#45875,#45876,#45877,#45878,#45879,
#45880,#45881),.UNSPECIFIED.,.F.,.F.,(4,3,4),(4.6736355815065E-5,0.576883414132736,
1.),.UNSPECIFIED.);
#1262=B_SPLINE_CURVE_WITH_KNOTS('',3,(#45898,#45899,#45900,#45901,#45902,
#45903,#45904,#45905,#45906,#45907),.UNSPECIFIED.,.F.,.F.,(4,3,3,4),(0.,
0.451687035355523,0.5,0.999999498615503),.UNSPECIFIED.);
#1263=B_SPLINE_CURVE_WITH_KNOTS('',3,(#45908,#45909,#45910,#45911,#45912,
#45913,#45914,#45915,#45916,#45917,#45918,#45919,#45920,#45921,#45922),
 .UNSPECIFIED.,.F.,.F.,(4,2,2,2,2,2,1,4),(2.1727933380804E-5,0.0019633771796468,
0.00405135872367098,0.00791551897190362,0.0117810714665637,0.0159268438952171,
0.0164431479993082,0.0169594521033993),.UNSPECIFIED.);
#1264=B_SPLINE_CURVE_WITH_KNOTS('',3,(#45938,#45939,#45940,#45941,#45942,
#45943,#45944,#45945,#45946,#45947),.UNSPECIFIED.,.F.,.F.,(4,3,3,4),(5.51904757954955E-7,
0.5,0.948505736358945,1.),.UNSPECIFIED.);
#1265=B_SPLINE_CURVE_WITH_KNOTS('',3,(#45949,#45950,#45951,#45952,#45953,
#45954,#45955,#45956,#45957,#45958,#45959,#45960,#45961),.UNSPECIFIED.,
 .F.,.F.,(4,3,3,3,4),(0.00644697767278411,0.459320221896434,0.5,0.949871368012603,
0.999999999972781),.UNSPECIFIED.);
#1266=B_SPLINE_CURVE_WITH_KNOTS('',3,(#45963,#45964,#45965,#45966,#45967,
#45968,#45969,#45970,#45971,#45972,#45973,#45974,#45975),.UNSPECIFIED.,
 .F.,.F.,(4,3,3,3,4),(6.24353372205677E-9,0.452961086122329,0.5,0.953477723055937,
0.993513142879381),.UNSPECIFIED.);
#1267=B_SPLINE_CURVE_WITH_KNOTS('',3,(#45991,#45992,#45993,#45994,#45995,
#45996,#45997,#45998,#45999,#46000,#46001,#46002,#46003,#46004,#46005),
 .UNSPECIFIED.,.F.,.F.,(4,2,2,2,2,2,1,4),(0.,0.00196334098438198,0.00405128809761397,
0.00791522560527698,0.0117805752183942,0.0153693852933397,0.0157369807117346,
0.0161045761301295),.UNSPECIFIED.);
#1268=B_SPLINE_CURVE_WITH_KNOTS('',3,(#46036,#46037,#46038,#46039,#46040,
#46041,#46042,#46043,#46044,#46045,#46046,#46047,#46048,#46049,#46050,#46051),
 .UNSPECIFIED.,.F.,.F.,(4,2,2,2,2,2,2,4),(0.000722180881357717,0.000952514205597523,
0.00178841244962457,0.00322807978575928,0.0069807773394597,0.0108844917476973,
0.0141878961748357,0.0172120373492915),.UNSPECIFIED.);
#1269=B_SPLINE_CURVE_WITH_KNOTS('',3,(#46052,#46053,#46054,#46055,#46056,
#46057,#46058,#46059,#46060,#46061,#46062,#46063,#46064,#46065),
 .UNSPECIFIED.,.F.,.F.,(4,2,2,2,2,2,4),(0.000101808612729993,0.00122101813875672,
0.00254413922241313,0.00564882750579106,0.0110994395641791,0.0185573990395054,
0.0194013094863756),.UNSPECIFIED.);
#1270=B_SPLINE_CURVE_WITH_KNOTS('',3,(#46081,#46082,#46083,#46084,#46085,
#46086,#46087),.UNSPECIFIED.,.F.,.F.,(4,3,4),(0.,0.64959466758675,0.99999619133487),
 .UNSPECIFIED.);
#1271=B_SPLINE_CURVE_WITH_KNOTS('',3,(#46089,#46090,#46091,#46092),
 .UNSPECIFIED.,.F.,.F.,(4,4),(0.,0.999938556780183),.UNSPECIFIED.);
#1272=B_SPLINE_CURVE_WITH_KNOTS('',3,(#46094,#46095,#46096,#46097,#46098,
#46099,#46100,#46101,#46102,#46103,#46104,#46105,#46106,#46107,#46108,#46109,
#46110,#46111,#46112,#46113,#46114,#46115),.UNSPECIFIED.,.F.,.F.,(4,2,2,
2,2,2,2,2,2,2,4),(0.0020350607393473,0.00212844484945634,0.00213147934112845,
0.0021671948648844,0.00225515824413027,0.0024494424110281,0.00643252326101599,
0.0104961302197796,0.0136428306082811,0.0152424631856715,0.01652133042803),
 .UNSPECIFIED.);
#1273=B_SPLINE_CURVE_WITH_KNOTS('',3,(#46117,#46118,#46119,#46120,#46121,
#46122,#46123),.UNSPECIFIED.,.F.,.F.,(4,3,4),(0.000310842092326198,0.644205206716935,
1.),.UNSPECIFIED.);
#1274=B_SPLINE_CURVE_WITH_KNOTS('',3,(#46140,#46141,#46142,#46143,#46144,
#46145,#46146),.UNSPECIFIED.,.F.,.F.,(4,3,4),(0.00202397953287585,0.684966626555327,
0.999983023180911),.UNSPECIFIED.);
#1275=B_SPLINE_CURVE_WITH_KNOTS('',3,(#46147,#46148,#46149,#46150,#46151,
#46152,#46153),.UNSPECIFIED.,.F.,.F.,(4,3,4),(2.09197363928788E-6,0.658100868662447,
0.999283474902518),.UNSPECIFIED.);
#1276=B_SPLINE_CURVE_WITH_KNOTS('',3,(#46155,#46156,#46157,#46158,#46159,
#46160,#46161,#46162,#46163,#46164),.UNSPECIFIED.,.F.,.F.,(4,3,3,4),(5.72594025237121E-7,
0.5,0.959255595777748,0.99999999765769),.UNSPECIFIED.);
#1277=B_SPLINE_CURVE_WITH_KNOTS('',3,(#46166,#46167,#46168,#46169,#46170,
#46171,#46172),.UNSPECIFIED.,.F.,.F.,(4,3,4),(0.,0.666190232468981,0.999999997883627),
 .UNSPECIFIED.);
#1278=B_SPLINE_CURVE_WITH_KNOTS('',3,(#46174,#46175,#46176,#46177,#46178,
#46179,#46180,#46181,#46182,#46183,#46184,#46185,#46186),.UNSPECIFIED.,
 .F.,.F.,(4,3,3,3,4),(4.22191385656518E-7,0.451253718316959,0.5,0.949460142126203,
0.999999851640557),.UNSPECIFIED.);
#1279=B_SPLINE_CURVE_WITH_KNOTS('',3,(#46199,#46200,#46201,#46202,#46203,
#46204,#46205,#46206,#46207,#46208,#46209,#46210,#46211,#46212,#46213,#46214),
 .UNSPECIFIED.,.F.,.F.,(4,2,2,2,2,2,2,4),(0.,0.00196384398390232,0.00405236912385508,
0.00791685933181361,0.0117828564538374,0.017303424189852,0.0182095740570904,
0.0188188355030872),.UNSPECIFIED.);
#1280=B_SPLINE_CURVE_WITH_KNOTS('',3,(#46216,#46217,#46218,#46219,#46220,
#46221,#46222,#46223,#46224,#46225,#46226,#46227,#46228),.UNSPECIFIED.,
 .F.,.F.,(4,3,3,3,4),(9.26612717775814E-7,0.443369457603659,0.5,0.94042683514852,
1.),.UNSPECIFIED.);
#1281=B_SPLINE_CURVE_WITH_KNOTS('',3,(#46244,#46245,#46246,#46247,#46248,
#46249,#46250),.UNSPECIFIED.,.F.,.F.,(4,3,4),(2.84623535879637E-8,0.585567534871793,
1.),.UNSPECIFIED.);
#1282=B_SPLINE_CURVE_WITH_KNOTS('',3,(#46252,#46253,#46254,#46255,#46256,
#46257,#46258,#46259,#46260,#46261),.UNSPECIFIED.,.F.,.F.,(4,3,3,4),(1.61060839561296E-7,
0.432923028701991,0.5,1.),.UNSPECIFIED.);
#1283=B_SPLINE_CURVE_WITH_KNOTS('',3,(#46263,#46264,#46265,#46266,#46267,
#46268,#46269),.UNSPECIFIED.,.F.,.F.,(4,3,4),(9.06643405643E-7,0.651743429231903,
0.999981902721839),.UNSPECIFIED.);
#1284=B_SPLINE_CURVE_WITH_KNOTS('',3,(#46288,#46289,#46290,#46291),
 .UNSPECIFIED.,.F.,.F.,(4,4),(2.36129832897646E-7,0.000200843834661843),
 .UNSPECIFIED.);
#1285=B_SPLINE_CURVE_WITH_KNOTS('',3,(#46293,#46294,#46295,#46296),
 .UNSPECIFIED.,.F.,.F.,(4,4),(7.44913368333112E-6,0.999999690593774),
 .UNSPECIFIED.);
#1286=B_SPLINE_CURVE_WITH_KNOTS('',3,(#46357,#46358,#46359,#46360,#46361,
#46362,#46363,#46364,#46365,#46366,#46367,#46368,#46369,#46370,#46371),
 .UNSPECIFIED.,.F.,.F.,(4,2,2,2,2,2,1,4),(-0.00778271397382138,-0.00683466317105913,
-0.00582123844929078,-0.00396333406938175,-0.00207855114507763,0.,0.000250637049053843,
0.000501274098107686),.UNSPECIFIED.);
#1287=B_SPLINE_CURVE_WITH_KNOTS('',3,(#46373,#46374,#46375,#46376,#46377,
#46378,#46379,#46380,#46381,#46382,#46383,#46384,#46385,#46386,#46387,#46388,
#46389,#46390,#46391,#46392,#46393,#46394),.UNSPECIFIED.,.F.,.F.,(4,2,2,
2,2,2,2,2,2,2,4),(-0.00014392415925499,0.,0.000143447984501406,0.000221109744414235,
0.00037269299334882,0.00066348171332673,0.00123679142420446,0.00338009045823901,
0.00507124205404184,0.00641905230452008,0.00701747059813978),
 .UNSPECIFIED.);
#1288=B_SPLINE_CURVE_WITH_KNOTS('',3,(#46452,#46453,#46454,#46455),
 .UNSPECIFIED.,.F.,.F.,(4,4),(2.37150890517029E-7,0.000201167851821411),
 .UNSPECIFIED.);
#1289=B_SPLINE_CURVE_WITH_KNOTS('',3,(#46457,#46458,#46459,#46460,#46461,
#46462,#46463,#46464,#46465,#46466,#46467,#46468,#46469,#46470),
 .UNSPECIFIED.,.F.,.F.,(4,2,2,2,2,2,4),(0.0135158126676436,0.014973489136333,
0.0171160883848495,0.0201226995874232,0.0244078688421797,0.0257108161548246,
0.026156838373642),.UNSPECIFIED.);
#1290=B_SPLINE_CURVE_WITH_KNOTS('',3,(#46489,#46490,#46491,#46492,#46493,
#46494,#46495,#46496,#46497,#46498),.UNSPECIFIED.,.F.,.F.,(4,3,3,4),(3.54217342568251E-7,
0.5,0.932995637830957,1.),.UNSPECIFIED.);
#1291=B_SPLINE_CURVE_WITH_KNOTS('',3,(#46500,#46501,#46502,#46503,#46504,
#46505,#46506,#46507,#46508,#46509,#46510,#46511,#46512,#46513,#46514),
 .UNSPECIFIED.,.F.,.F.,(4,2,2,2,2,2,1,4),(0.0113718137346511,0.0125803262387957,
0.0142088530539494,0.0166548137430588,0.0214923420820296,0.02224678217811,
0.0224951901254519,0.0226872803324734),.UNSPECIFIED.);
#1292=B_SPLINE_CURVE_WITH_KNOTS('',3,(#46516,#46517,#46518,#46519,#46520,
#46521,#46522,#46523,#46524,#46525,#46526,#46527,#46528,#46529,#46530,#46531),
 .UNSPECIFIED.,.F.,.F.,(4,2,2,2,2,2,2,4),(0.0340922557365839,0.0343333033692608,
0.0346628514377239,0.0356154235520354,0.038017654942319,0.0396060348908877,
0.0406978337520487,0.0414157425803844),.UNSPECIFIED.);
#1293=B_SPLINE_CURVE_WITH_KNOTS('',3,(#46533,#46534,#46535,#46536,#46537,
#46538,#46539,#46540,#46541,#46542,#46543,#46544,#46545,#46546,#46547),
 .UNSPECIFIED.,.F.,.F.,(4,2,2,2,2,2,1,4),(0.,0.00222424191990565,0.00465511287046728,
0.00879447482255024,0.0133938157884664,0.0178039143331782,0.0182880999169529,
0.0187722855007277),.UNSPECIFIED.);
#1294=B_SPLINE_CURVE_WITH_KNOTS('',3,(#46549,#46550,#46551,#46552,#46553,
#46554,#46555,#46556,#46557,#46558,#46559,#46560,#46561,#46562),
 .UNSPECIFIED.,.F.,.F.,(4,2,2,2,2,2,4),(0.0156003477411163,0.0172855752039469,
0.0197606565720376,0.023234278347158,0.0281861916552709,0.029684187273598,
0.0301983776561063),.UNSPECIFIED.);
#1295=B_SPLINE_CURVE_WITH_KNOTS('',3,(#46584,#46585,#46586,#46587,#46588,
#46589,#46590,#46591,#46592,#46593,#46594,#46595,#46596,#46597),
 .UNSPECIFIED.,.F.,.F.,(4,2,2,2,2,2,4),(-0.0205682128831986,-0.017816287435113,
-0.0146537481341808,-0.00960273674078747,-0.00481443689872726,0.,0.00102941491059151),
 .UNSPECIFIED.);
#1296=B_SPLINE_CURVE_WITH_KNOTS('',3,(#46599,#46600,#46601,#46602,#46603,
#46604,#46605,#46606,#46607,#46608,#46609,#46610,#46611,#46612,#46613,#46614,
#46615,#46616,#46617,#46618,#46619,#46620),.UNSPECIFIED.,.F.,.F.,(4,2,2,
2,2,2,2,2,2,2,4),(-0.000143830183900261,0.,0.000143597679787919,0.000221235739118977,
0.000372775263706832,0.000663460743001667,0.0012365400442185,0.00337954254859572,
0.00507043814008076,0.00641801410969039,0.00701649344940931),
 .UNSPECIFIED.);
#1297=B_SPLINE_CURVE_WITH_KNOTS('',3,(#46684,#46685,#46686,#46687,#46688,
#46689,#46690,#46691,#46692,#46693,#46694,#46695,#46696,#46697),
 .UNSPECIFIED.,.F.,.F.,(4,2,2,2,2,2,4),(2.99246733186488E-6,0.00201249960757762,
0.0041632863175498,0.00810591663337533,0.0121030557146972,0.0158488156731948,
0.016732647820978),.UNSPECIFIED.);
#1298=B_SPLINE_CURVE_WITH_KNOTS('',3,(#46699,#46700,#46701,#46702,#46703,
#46704,#46705),.UNSPECIFIED.,.F.,.F.,(4,3,4),(5.48439606298742E-7,0.5,0.999997140301748),
 .UNSPECIFIED.);
#1299=B_SPLINE_CURVE_WITH_KNOTS('',3,(#46763,#46764,#46765,#46766),
 .UNSPECIFIED.,.F.,.F.,(4,4),(2.30992785970066E-7,0.000202736252405272),
 .UNSPECIFIED.);
#1300=B_SPLINE_CURVE_WITH_KNOTS('',3,(#46768,#46769,#46770,#46771,#46772,
#46773,#46774),.UNSPECIFIED.,.F.,.F.,(4,3,4),(0.,0.546479382302658,1.),
 .UNSPECIFIED.);
#1301=B_SPLINE_CURVE_WITH_KNOTS('',3,(#46793,#46794,#46795,#46796,#46797,
#46798,#46799,#46800,#46801,#46802,#46803,#46804,#46805,#46806,#46807,#46808,
#46809,#46810,#46811,#46812,#46813,#46814,#46815,#46816,#46817,#46818,#46819,
#46820,#46821,#46822,#46823,#46824,#46825,#46826,#46827,#46828,#46829),
 .UNSPECIFIED.,.F.,.F.,(4,1,2,2,2,2,2,2,2,2,2,2,2,2,2,2,2,2,4),(0.0059034039032535,
0.00649662725925484,0.00656341819149157,0.00658448987750684,0.00660487226112149,
0.00663152428214414,0.00665679213150518,0.00670867157264048,0.00728399544932138,
0.00780646930469712,0.00856811246381833,0.00980419850919031,0.0121806465476813,
0.0191679676383439,0.041410165517959,0.0802961750511084,0.115456796415773,
0.136085623600931,0.154936455995216),.UNSPECIFIED.);
#1302=B_SPLINE_CURVE_WITH_KNOTS('',3,(#46831,#46832,#46833,#46834,#46835,
#46836,#46837),.UNSPECIFIED.,.F.,.F.,(4,3,4),(2.86657951474293E-8,0.591763262396974,
1.),.UNSPECIFIED.);
#1303=B_SPLINE_CURVE_WITH_KNOTS('',3,(#46839,#46840,#46841,#46842,#46843,
#46844,#46845,#46846,#46847,#46848),.UNSPECIFIED.,.F.,.F.,(4,3,3,4),(5.87574713772567E-7,
0.500000293787357,0.930259890397214,0.999999731521238),.UNSPECIFIED.);
#1304=B_SPLINE_CURVE_WITH_KNOTS('',3,(#46864,#46865,#46866,#46867,#46868,
#46869,#46870,#46871,#46872,#46873,#46874,#46875,#46876,#46877,#46878,#46879),
 .UNSPECIFIED.,.F.,.F.,(4,2,2,2,2,2,2,4),(-0.00390306697050034,-0.00352231899423164,
-0.00311739545282296,-0.00236817122813141,-0.00161861983209088,-0.000555049807796949,
-0.000416527677959817,-0.000252358784354016),.UNSPECIFIED.);
#1305=B_SPLINE_CURVE_WITH_KNOTS('',3,(#46881,#46882,#46883,#46884,#46885,
#46886,#46887,#46888,#46889,#46890,#46891,#46892,#46893),.UNSPECIFIED.,
 .F.,.F.,(4,3,3,3,4),(0.,0.451351771143798,0.499999612007475,0.952090754403713,
0.999999223904282),.UNSPECIFIED.);
#1306=B_SPLINE_CURVE_WITH_KNOTS('',3,(#46906,#46907,#46908,#46909,#46910,
#46911,#46912),.UNSPECIFIED.,.F.,.F.,(4,3,4),(0.,0.663177241834219,0.999999999703733),
 .UNSPECIFIED.);
#1307=B_SPLINE_CURVE_WITH_KNOTS('',3,(#46914,#46915,#46916,#46917,#46918,
#46919,#46920,#46921,#46922,#46923),.UNSPECIFIED.,.F.,.F.,(4,3,3,4),(4.05016758157343E-7,
0.5,0.95857558711876,0.999999999242644),.UNSPECIFIED.);
#1308=B_SPLINE_CURVE_WITH_KNOTS('',3,(#46925,#46926,#46927,#46928,#46929,
#46930,#46931),.UNSPECIFIED.,.F.,.F.,(4,3,4),(1.19975828902745E-5,0.575510273364395,
0.99815504015047),.UNSPECIFIED.);
#1309=B_SPLINE_CURVE_WITH_KNOTS('',3,(#46933,#46934,#46935,#46936,#46937,
#46938,#46939),.UNSPECIFIED.,.F.,.F.,(4,3,4),(0.000609342180978295,0.5,
0.99999969898345),.UNSPECIFIED.);
#1310=B_SPLINE_CURVE_WITH_KNOTS('',3,(#46992,#46993,#46994,#46995,#46996,
#46997,#46998),.UNSPECIFIED.,.F.,.F.,(4,3,4),(1.62696442369048E-8,0.000133938713825017,
0.000161353569749288),.UNSPECIFIED.);
#1311=B_SPLINE_CURVE_WITH_KNOTS('',3,(#46999,#47000,#47001,#47002,#47003,
#47004,#47005,#47006,#47007,#47008,#47009,#47010,#47011,#47012,#47013,#47014,
#47015,#47016,#47017,#47018,#47019,#47020),.UNSPECIFIED.,.F.,.F.,(4,2,2,
2,2,2,2,2,2,2,4),(-0.0121117789361161,-0.0105531999363958,-0.00882659923363592,
-0.00598279969381208,-0.00275319141802341,-0.00142567726470279,-0.000757158957527394,
-0.000425414570489878,-0.000260434122667489,-0.000159073980362508,-2.05838487038443E-5),
 .UNSPECIFIED.);
#1312=B_SPLINE_CURVE_WITH_KNOTS('',3,(#47069,#47070,#47071,#47072,#47073,
#47074,#47075),.UNSPECIFIED.,.F.,.F.,(4,3,4),(1.65353367717499E-8,0.000133977101550613,
0.000161445935848968),.UNSPECIFIED.);
#1313=B_SPLINE_CURVE_WITH_KNOTS('',3,(#47127,#47128,#47129,#47130,#47131,
#47132,#47133,#47134,#47135,#47136,#47137,#47138,#47139,#47140,#47141,#47142,
#47143,#47144,#47145,#47146,#47147),.UNSPECIFIED.,.F.,.F.,(4,2,2,2,2,2,
2,2,2,1,4),(0.,0.00222984288937753,0.00469946423214668,0.00876653081177419,
0.0133799493316473,0.0153650476469126,0.0163343894682131,0.0168305855295093,
0.0171007793566801,0.0172993328283054,0.01748691231476),.UNSPECIFIED.);
#1314=B_SPLINE_CURVE_WITH_KNOTS('',3,(#47239,#47240,#47241,#47242,#47243,
#47244,#47245,#47246,#47247,#47248,#47249),.UNSPECIFIED.,.F.,.F.,(4,1,1,
1,1,1,1,1,4),(3.17007800203674E-7,0.00137241382077849,0.00274482764155697,
0.00411724146233546,0.00548965528311394,0.00686206910389242,0.00823448292467091,
0.00960689674544939,0.0108038290876045),.UNSPECIFIED.);
#1315=B_SPLINE_CURVE_WITH_KNOTS('',3,(#47255,#47256,#47257,#47258,#47259,
#47260,#47261,#47262,#47263,#47264,#47265,#47266,#47267,#47268,#47269,#47270),
 .UNSPECIFIED.,.F.,.F.,(4,3,3,3,3,4),(0.5,0.51594481978154,0.641195140394408,
0.766134114390843,0.890913197743559,1.),.UNSPECIFIED.);
#1316=B_SPLINE_CURVE_WITH_KNOTS('',3,(#47271,#47272,#47273,#47274,#47275,
#47276,#47277,#47278,#47279,#47280,#47281,#47282,#47283),.UNSPECIFIED.,
 .F.,.F.,(4,3,3,3,4),(0.01606865131382,0.141192218026199,0.265882467388624,
0.390722415283828,0.5),.UNSPECIFIED.);
#1317=B_SPLINE_CURVE_WITH_KNOTS('',3,(#47323,#47324,#47325,#47326,#47327,
#47328,#47329,#47330,#47331,#47332,#47333,#47334,#47335),.UNSPECIFIED.,
 .F.,.F.,(4,3,3,3,4),(0.844373201093006,0.868421052636719,0.901315789477539,
0.934210526318359,0.956585831262424),.UNSPECIFIED.);
#1318=B_SPLINE_CURVE_WITH_KNOTS('',3,(#47337,#47338,#47339,#47340,#47341,
#47342,#47343,#47344,#47345,#47346,#47347,#47348,#47349,#47350,#47351,#47352,
#47353,#47354,#47355,#47356,#47357,#47358),.UNSPECIFIED.,.F.,.F.,(4,3,3,
3,3,3,3,4),(0.595152011141008,0.6184210546875,0.649671054199219,0.680921053710937,
0.743421052734375,0.774671052709961,0.805921052685547,0.844373201093006),
 .UNSPECIFIED.);
#1319=B_SPLINE_CURVE_WITH_KNOTS('',3,(#47360,#47361,#47362,#47363,#47364,
#47365,#47366,#47367,#47368,#47369),.UNSPECIFIED.,.F.,.F.,(4,3,3,4),(0.499571204578003,
0.524671083984375,0.55592107421875,0.595152011141008),.UNSPECIFIED.);
#1320=B_SPLINE_CURVE_WITH_KNOTS('',3,(#47371,#47372,#47373,#47374,#47375,
#47376,#47377,#47378,#47379,#47380,#47381,#47382,#47383,#47384,#47385,#47386),
 .UNSPECIFIED.,.F.,.F.,(4,3,3,3,3,4),(0.344377029418945,0.368421875,0.3996716796875,
0.430921484375,0.49342109375,0.499571204578003),.UNSPECIFIED.);
#1321=B_SPLINE_CURVE_WITH_KNOTS('',3,(#47388,#47389,#47390,#47391,#47392,
#47393,#47394,#47395,#47396,#47397,#47398,#47399,#47400,#47401,#47402,#47403,
#47404,#47405,#47406,#47407,#47408,#47409),.UNSPECIFIED.,.F.,.F.,(4,3,3,
3,3,3,3,4),(0.0951513536663715,0.11875,0.149921875,0.18109375,0.2434375,
0.27468359375,0.3059296875,0.344377029418945),.UNSPECIFIED.);
#1322=B_SPLINE_CURVE_WITH_KNOTS('',3,(#47411,#47412,#47413,#47414,#47415,
#47416,#47417),.UNSPECIFIED.,.F.,.F.,(4,3,4),(0.,0.059375,0.0951513536663715),
 .UNSPECIFIED.);
#1323=B_SPLINE_CURVE_WITH_KNOTS('',3,(#47422,#47423,#47424,#47425,#47426,
#47427,#47428,#47429,#47430,#47431,#47432,#47433,#47434,#47435,#47436,#47437,
#47438,#47439,#47440,#47441,#47442,#47443,#47444,#47445,#47446,#47447,#47448,
#47449),.UNSPECIFIED.,.F.,.F.,(4,3,3,3,3,3,3,3,3,4),(0.000439637419233018,
0.00197475622652821,0.00351361546357811,0.00505249384731604,0.00658820808674074,
0.00812412382728726,0.00966469812314125,0.0112015348521649,0.0122952440085163,
0.0122953616167891),.UNSPECIFIED.);
#1324=B_SPLINE_CURVE_WITH_KNOTS('',3,(#47498,#47499,#47500,#47501,#47502,
#47503,#47504,#47505,#47506,#47507,#47508,#47509,#47510,#47511,#47512,#47513,
#47514,#47515),.UNSPECIFIED.,.F.,.F.,(4,2,2,2,2,2,2,2,4),(0.0531545443972438,
0.0539804531362699,0.0553833366067717,0.063256430848433,0.0837219286225868,
0.0893954400242927,0.0917963407013744,0.109557936372639,0.132545890778438),
 .UNSPECIFIED.);
#1325=B_SPLINE_CURVE_WITH_KNOTS('',3,(#47519,#47520,#47521,#47522,#47523,
#47524,#47525,#47526,#47527,#47528,#47529,#47530,#47531,#47532,#47533,#47534,
#47535,#47536,#47537,#47538),.UNSPECIFIED.,.F.,.F.,(4,2,2,2,2,2,2,2,2,4),
(-0.158319955435896,-0.133815137850197,-0.106658138126813,-0.1025999008806,
-0.10032932226052,-0.0927408284757264,-0.079200925255067,-0.0410108789329117,
-0.0204087370161667,-3.15727931039809E-5),.UNSPECIFIED.);
#1326=B_SPLINE_CURVE_WITH_KNOTS('',3,(#47540,#47541,#47542,#47543,#47544,
#47545,#47546,#47547,#47548,#47549,#47550,#47551,#47552,#47553,#47554,#47555,
#47556,#47557,#47558,#47559,#47560,#47561,#47562,#47563,#47564,#47565,#47566,
#47567),.UNSPECIFIED.,.F.,.F.,(4,2,2,2,2,2,2,2,2,2,2,2,2,4),(-0.159255089654321,
-0.157276407559694,-0.15499281392426,-0.150445878334476,-0.141416102996633,
-0.123174516039657,-0.120748346467183,-0.118169256846349,-0.110388837257784,
-0.0973026115125197,-0.0773140984503772,-0.0425520341965917,-0.0212391987124548,
-0.00028544784231343),.UNSPECIFIED.);
#1327=B_SPLINE_CURVE_WITH_KNOTS('',3,(#47569,#47570,#47571,#47572,#47573,
#47574,#47575,#47576,#47577,#47578,#47579,#47580,#47581,#47582,#47583,#47584,
#47585,#47586,#47587,#47588,#47589,#47590,#47591,#47592,#47593,#47594,#47595,
#47596,#47597,#47598),.UNSPECIFIED.,.F.,.F.,(4,2,2,2,2,2,2,2,2,2,2,2,2,
2,4),(-0.159252699730232,-0.138336557138345,-0.117015600794963,-0.0822235719847124,
-0.0627557354776325,-0.0495418275572358,-0.0416948308426409,-0.0390988462294192,
-0.0341970288432549,-0.0170804313544768,-0.00858037755543813,-0.00430003517675335,
-0.00215149799157384,-0.00107591423944001,-0.000284742483905729),
 .UNSPECIFIED.);
#1328=B_SPLINE_CURVE_WITH_KNOTS('',3,(#47600,#47601,#47602,#47603,#47604,
#47605,#47606,#47607,#47608,#47609,#47610,#47611,#47612,#47613,#47614,#47615,
#47616,#47617,#47618,#47619,#47620,#47621),.UNSPECIFIED.,.F.,.F.,(4,2,2,
2,2,2,2,2,2,2,4),(-0.158572104573442,-0.138210910124321,-0.117619222785882,
-0.0794253157638306,-0.0659793598497864,-0.0584299861442276,-0.0561593995498526,
-0.0551566920948119,-0.0533519008406549,-0.0276603098885798,-0.000285004372809575),
 .UNSPECIFIED.);
#1329=B_SPLINE_CURVE_WITH_KNOTS('',3,(#47629,#47630,#47631,#47632),
 .UNSPECIFIED.,.F.,.F.,(4,4),(0.00694070085523101,0.00719068424449337),
 .UNSPECIFIED.);
#1330=B_SPLINE_CURVE_WITH_KNOTS('',3,(#47634,#47635,#47636,#47637,#47638,
#47639,#47640),.UNSPECIFIED.,.F.,.F.,(4,3,4),(0.00495768279518325,0.00594874941015533,
0.00694020764518122),.UNSPECIFIED.);
#1331=B_SPLINE_CURVE_WITH_KNOTS('',3,(#47642,#47643,#47644,#47645),
 .UNSPECIFIED.,.F.,.F.,(4,4),(0.00396583294010356,0.00495729117512944),
 .UNSPECIFIED.);
#1332=B_SPLINE_CURVE_WITH_KNOTS('',3,(#47647,#47648,#47649,#47650),
 .UNSPECIFIED.,.F.,.F.,(4,4),(0.00297486717136914,0.00396583294010356),
 .UNSPECIFIED.);
#1333=B_SPLINE_CURVE_WITH_KNOTS('',3,(#47652,#47653,#47654,#47655,#47656,
#47657,#47658),.UNSPECIFIED.,.F.,.F.,(4,3,4),(0.000991836196938153,0.00198291647005178,
0.00297437470507767),.UNSPECIFIED.);
#1334=B_SPLINE_CURVE_WITH_KNOTS('',3,(#47659,#47660,#47661,#47662),
 .UNSPECIFIED.,.F.,.F.,(4,4),(0.,0.000991458235025889),.UNSPECIFIED.);
#1335=B_SPLINE_CURVE_WITH_KNOTS('',3,(#47714,#47715,#47716,#47717),
 .UNSPECIFIED.,.F.,.F.,(4,4),(1.17608272849176E-7,0.000439637419233018),
 .UNSPECIFIED.);
#1336=B_SPLINE_CURVE_WITH_KNOTS('',3,(#47752,#47753,#47754,#47755),
 .UNSPECIFIED.,.F.,.F.,(4,4),(0.,0.01606865131382),.UNSPECIFIED.);
#1337=B_SPLINE_CURVE_WITH_KNOTS('',3,(#47756,#47757,#47758,#47759,#47760,
#47761,#47762),.UNSPECIFIED.,.F.,.F.,(4,3,4),(0.956585831262424,0.96710526315918,
1.),.UNSPECIFIED.);
#1338=B_SPLINE_CURVE_WITH_KNOTS('',3,(#47769,#47770,#47771,#47772,#47773,
#47774,#47775,#47776,#47777,#47778,#47779,#47780),.UNSPECIFIED.,.F.,.F.,
(4,2,2,2,2,4),(5.52024392907501E-5,0.0144625442992462,0.0165414513429709,
0.0327826202138422,0.0527118689517175,0.0531545443972438),.UNSPECIFIED.);
#1339=B_SPLINE_CURVE_WITH_KNOTS('',3,(#47785,#47786,#47787,#47788),
 .UNSPECIFIED.,.F.,.F.,(4,4),(8.74111736584338E-18,3.17007800203674E-7),
 .UNSPECIFIED.);
#1340=B_SPLINE_CURVE_WITH_KNOTS('',3,(#47789,#47790,#47791,#47792),
 .UNSPECIFIED.,.F.,.F.,(4,4),(0.0108038290876045,0.0109793105662279),
 .UNSPECIFIED.);
#1341=B_SPLINE_CURVE_WITH_KNOTS('',3,(#47795,#47796,#47797,#47798,#47799,
#47800,#47801),.UNSPECIFIED.,.F.,.F.,(4,3,4),(0.,0.059375,0.12171875),
 .UNSPECIFIED.);
#1342=B_SPLINE_CURVE_WITH_KNOTS('',3,(#47803,#47804,#47805,#47806,#47807,
#47808,#47809,#47810,#47811,#47812,#47813,#47814,#47815,#47816,#47817,#47818,
#47819,#47820,#47821),.UNSPECIFIED.,.F.,.F.,(4,3,3,3,3,3,4),(0.12171875,
0.1545234375,0.185851171875,0.21710505859375,0.248355252929687,0.309292762646484,
0.371714638132324),.UNSPECIFIED.);
#1343=B_SPLINE_CURVE_WITH_KNOTS('',3,(#47823,#47824,#47825,#47826,#47827,
#47828,#47829,#47830,#47831,#47832),.UNSPECIFIED.,.F.,.F.,(4,3,3,4),(0.371714638132324,
0.434210731906616,0.496710536595331,0.500091425325073),.UNSPECIFIED.);
#1344=B_SPLINE_CURVE_WITH_KNOTS('',3,(#47834,#47835,#47836,#47837,#47838,
#47839,#47840),.UNSPECIFIED.,.F.,.F.,(4,3,4),(0.500091425325073,0.559210526829766,
0.621710526341488),.UNSPECIFIED.);
#1345=B_SPLINE_CURVE_WITH_KNOTS('',3,(#47842,#47843,#47844,#47845,#47846,
#47847,#47848,#47849,#47850,#47851,#47852,#47853,#47854,#47855,#47856,#47857,
#47858,#47859,#47860),.UNSPECIFIED.,.F.,.F.,(4,3,3,3,3,3,4),(0.621710526341488,
0.684210526317074,0.746710526315854,0.779523026315793,0.81085115131579,
0.842105057565789,0.873355252878289),.UNSPECIFIED.);
#1346=B_SPLINE_CURVE_WITH_KNOTS('',3,(#47861,#47862,#47863,#47864,#47865,
#47866,#47867),.UNSPECIFIED.,.F.,.F.,(4,3,4),(0.873355252878289,0.934292762643914,
1.),.UNSPECIFIED.);
#1347=B_SPLINE_CURVE_WITH_KNOTS('',3,(#47873,#47874,#47875,#47876),
 .UNSPECIFIED.,.F.,.F.,(4,4),(0.00719068424449337,0.00793166588020711),
 .UNSPECIFIED.);
#1348=B_SPLINE_CURVE_WITH_KNOTS('',3,(#48811,#48812,#48813,#48814,#48815,
#48816,#48817,#48818,#48819,#48820,#48821,#48822,#48823,#48824),
 .UNSPECIFIED.,.F.,.F.,(4,2,2,2,2,2,4),(-0.0166502448320504,-0.0131502648660712,
-0.00944645224428793,-0.0052854765179261,-0.00265904695122474,0.,0.000159874250087339),
 .UNSPECIFIED.);
#1349=B_SPLINE_CURVE_WITH_KNOTS('',3,(#48825,#48826,#48827,#48828,#48829,
#48830,#48831,#48832,#48833,#48834,#48835,#48836,#48837,#48838),
 .UNSPECIFIED.,.F.,.F.,(4,2,2,2,2,2,4),(0.0166502448320816,0.0201502247980731,
0.0238540374198661,0.0280150131462326,0.0306414427129375,0.0333004896641681,
0.0334603639142559),.UNSPECIFIED.);
#1350=B_SPLINE_CURVE_WITH_KNOTS('',3,(#48849,#48850,#48851,#48852,#48853,
#48854,#48855,#48856,#48857,#48858,#48859,#48860,#48861,#48862),
 .UNSPECIFIED.,.F.,.F.,(4,2,2,2,2,2,4),(0.016650244832051,0.0201502247980302,
0.0238540374198133,0.0280150131461748,0.0306414427128761,0.0333004896641017,
0.033460363914188),.UNSPECIFIED.);
#1351=B_SPLINE_CURVE_WITH_KNOTS('',3,(#48863,#48864,#48865,#48866,#48867,
#48868,#48869,#48870,#48871,#48872,#48873,#48874,#48875,#48876),
 .UNSPECIFIED.,.F.,.F.,(4,2,2,2,2,2,4),(-0.0166502448320804,-0.0131502648660892,
-0.00944645224429652,-0.00528547651792783,-0.00265904695122334,0.,0.000159874250087547),
 .UNSPECIFIED.);
#1352=B_SPLINE_CURVE_WITH_KNOTS('',3,(#48950,#48951,#48952,#48953),
 .UNSPECIFIED.,.F.,.F.,(4,4),(2.77758216759816E-8,0.0598155593219101),
 .UNSPECIFIED.);
#1353=B_SPLINE_CURVE_WITH_KNOTS('',3,(#48955,#48956,#48957,#48958,#48959,
#48960,#48961,#48962,#48963,#48964),.UNSPECIFIED.,.F.,.F.,(4,3,3,4),(0.0598155593219101,
0.400094789280781,0.882156340214427,1.),.UNSPECIFIED.);
#1354=B_SPLINE_CURVE_WITH_KNOTS('',3,(#48989,#48990,#48991,#48992),
 .UNSPECIFIED.,.F.,.F.,(4,4),(2.77758270156303E-8,0.0598155595006793),
 .UNSPECIFIED.);
#1355=B_SPLINE_CURVE_WITH_KNOTS('',3,(#48994,#48995,#48996,#48997,#48998,
#48999,#49000,#49001,#49002,#49003),.UNSPECIFIED.,.F.,.F.,(4,3,3,4),(0.0598155595006793,
0.400094789276241,0.882156340205139,1.),.UNSPECIFIED.);
#1356=B_SPLINE_CURVE_WITH_KNOTS('',3,(#49031,#49032,#49033,#49034,#49035,
#49036,#49037),.UNSPECIFIED.,.F.,.F.,(4,3,4),(0.,0.811097963900528,0.999989357516093),
 .UNSPECIFIED.);
#1357=B_SPLINE_CURVE_WITH_KNOTS('',3,(#49045,#49046,#49047,#49048,#49049,
#49050,#49051),.UNSPECIFIED.,.F.,.F.,(4,3,4),(0.,0.851452914537907,0.999998335389822),
 .UNSPECIFIED.);
#1358=B_SPLINE_CURVE_WITH_KNOTS('',3,(#49060,#49061,#49062,#49063,#49064,
#49065,#49066),.UNSPECIFIED.,.F.,.F.,(4,3,4),(0.000148834785990088,0.811264189000227,
1.),.UNSPECIFIED.);
#1359=B_SPLINE_CURVE_WITH_KNOTS('',3,(#49074,#49075,#49076,#49077,#49078,
#49079,#49080),.UNSPECIFIED.,.F.,.F.,(4,3,4),(1.66717332357201E-6,0.851450337612495,
1.),.UNSPECIFIED.);
#1360=B_SPLINE_CURVE_WITH_KNOTS('',3,(#49082,#49083,#49084,#49085,#49086,
#49087,#49088),.UNSPECIFIED.,.F.,.F.,(4,3,4),(0.00014883478557751,0.81126418904293,
1.),.UNSPECIFIED.);
#1361=B_SPLINE_CURVE_WITH_KNOTS('',3,(#49109,#49110,#49111,#49112,#49113,
#49114,#49115),.UNSPECIFIED.,.F.,.F.,(4,3,4),(0.,0.811097963770035,0.999989357516),
 .UNSPECIFIED.);
#1362=B_SPLINE_CURVE_WITH_KNOTS('',3,(#49171,#49172,#49173,#49174,#49175,
#49176,#49177,#49178,#49179,#49180,#49181),.UNSPECIFIED.,.F.,.F.,(4,1,1,
1,1,1,1,1,4),(2.16840434497101E-19,0.00133638350122092,0.00267276700244183,
0.00400915050366275,0.00534553400488367,0.00668191750610458,0.0080183010073255,
0.00935468450854642,0.0106661079505718),.UNSPECIFIED.);
#1363=B_SPLINE_CURVE_WITH_KNOTS('',3,(#49187,#49188,#49189,#49190),
 .UNSPECIFIED.,.F.,.F.,(4,4),(0.0082109079468729,0.00936873648796082),
 .UNSPECIFIED.);
#1364=B_SPLINE_CURVE_WITH_KNOTS('',3,(#49192,#49193,#49194,#49195,#49196),
 .UNSPECIFIED.,.F.,.F.,(4,1,4),(0.00704598836791066,0.00819764442696572,
0.0082109079468729),.UNSPECIFIED.);
#1365=B_SPLINE_CURVE_WITH_KNOTS('',3,(#49198,#49199,#49200,#49201,#49202),
 .UNSPECIFIED.,.F.,.F.,(4,1,4),(0.00585546030497552,0.00702655236597062,
0.00704598836791066),.UNSPECIFIED.);
#1366=B_SPLINE_CURVE_WITH_KNOTS('',3,(#49204,#49205,#49206,#49207,#49208),
 .UNSPECIFIED.,.F.,.F.,(4,1,4),(0.00352617550117164,0.00468436824398041,
0.00585546030497552),.UNSPECIFIED.);
#1367=B_SPLINE_CURVE_WITH_KNOTS('',3,(#49210,#49211,#49212,#49213,#49214),
 .UNSPECIFIED.,.F.,.F.,(4,1,4),(0.00236041305988056,0.00351327618298531,
0.00352617550117164),.UNSPECIFIED.);
#1368=B_SPLINE_CURVE_WITH_KNOTS('',3,(#49216,#49217,#49218,#49219,#49220),
 .UNSPECIFIED.,.F.,.F.,(4,1,4),(0.0011710920609951,0.00234218412199021,
0.00236041305988056),.UNSPECIFIED.);
#1369=B_SPLINE_CURVE_WITH_KNOTS('',3,(#49221,#49222,#49223,#49224),
 .UNSPECIFIED.,.F.,.F.,(4,4),(2.22095063237474E-5,0.0011710920609951),
 .UNSPECIFIED.);
#1370=B_SPLINE_CURVE_WITH_KNOTS('',3,(#49264,#49265,#49266,#49267,#49268,
#49269,#49270,#49271,#49272,#49273,#49274),.UNSPECIFIED.,.F.,.F.,(4,1,1,
1,1,1,1,1,4),(2.16840434497101E-19,0.00133638350122092,0.00267276700244184,
0.00400915050366276,0.00534553400488369,0.00668191750610461,0.00801830100732553,
0.00935468450854645,0.0106661079505719),.UNSPECIFIED.);
#1371=B_SPLINE_CURVE_WITH_KNOTS('',3,(#49280,#49281,#49282,#49283),
 .UNSPECIFIED.,.F.,.F.,(4,4),(0.00821090794687196,0.00936873648796082),
 .UNSPECIFIED.);
#1372=B_SPLINE_CURVE_WITH_KNOTS('',3,(#49285,#49286,#49287,#49288,#49289),
 .UNSPECIFIED.,.F.,.F.,(4,1,4),(0.00704598836790975,0.00819764442696572,
0.00821090794687196),.UNSPECIFIED.);
#1373=B_SPLINE_CURVE_WITH_KNOTS('',3,(#49291,#49292,#49293,#49294,#49295),
 .UNSPECIFIED.,.F.,.F.,(4,1,4),(0.00585546030497551,0.00702655236597062,
0.00704598836790975),.UNSPECIFIED.);
#1374=B_SPLINE_CURVE_WITH_KNOTS('',3,(#49297,#49298,#49299,#49300,#49301),
 .UNSPECIFIED.,.F.,.F.,(4,1,4),(0.00352617550117226,0.00468436824398041,
0.00585546030497551),.UNSPECIFIED.);
#1375=B_SPLINE_CURVE_WITH_KNOTS('',3,(#49303,#49304,#49305,#49306,#49307),
 .UNSPECIFIED.,.F.,.F.,(4,1,4),(0.00236041305988015,0.00351327618298531,
0.00352617550117226),.UNSPECIFIED.);
#1376=B_SPLINE_CURVE_WITH_KNOTS('',3,(#49309,#49310,#49311,#49312,#49313),
 .UNSPECIFIED.,.F.,.F.,(4,1,4),(0.0011710920609951,0.00234218412199021,
0.00236041305988015),.UNSPECIFIED.);
#1377=B_SPLINE_CURVE_WITH_KNOTS('',3,(#49314,#49315,#49316,#49317),
 .UNSPECIFIED.,.F.,.F.,(4,4),(2.22095063236846E-5,0.0011710920609951),
 .UNSPECIFIED.);
#1378=B_SPLINE_CURVE_WITH_KNOTS('',3,(#49357,#49358,#49359,#49360,#49361,
#49362,#49363,#49364,#49365,#49366,#49367),.UNSPECIFIED.,.F.,.F.,(4,1,1,
1,1,1,1,1,4),(2.16840434497101E-19,0.00133638350122092,0.00267276700244184,
0.00400915050366277,0.00534553400488369,0.00668191750610461,0.00801830100732553,
0.00935468450854646,0.0106661079505718),.UNSPECIFIED.);
#1379=B_SPLINE_CURVE_WITH_KNOTS('',3,(#49373,#49374,#49375,#49376),
 .UNSPECIFIED.,.F.,.F.,(4,4),(0.00821090794687294,0.00936873648796081),
 .UNSPECIFIED.);
#1380=B_SPLINE_CURVE_WITH_KNOTS('',3,(#49378,#49379,#49380,#49381,#49382),
 .UNSPECIFIED.,.F.,.F.,(4,1,4),(0.00704598836791145,0.00819764442696571,
0.00821090794687294),.UNSPECIFIED.);
#1381=B_SPLINE_CURVE_WITH_KNOTS('',3,(#49384,#49385,#49386,#49387,#49388),
 .UNSPECIFIED.,.F.,.F.,(4,1,4),(0.00585546030497551,0.00702655236597061,
0.00704598836791145),.UNSPECIFIED.);
#1382=B_SPLINE_CURVE_WITH_KNOTS('',3,(#49390,#49391,#49392,#49393,#49394),
 .UNSPECIFIED.,.F.,.F.,(4,1,4),(0.00352617550117169,0.00468436824398041,
0.00585546030497551),.UNSPECIFIED.);
#1383=B_SPLINE_CURVE_WITH_KNOTS('',3,(#49396,#49397,#49398,#49399,#49400),
 .UNSPECIFIED.,.F.,.F.,(4,1,4),(0.00236041305987884,0.00351327618298531,
0.00352617550117169),.UNSPECIFIED.);
#1384=B_SPLINE_CURVE_WITH_KNOTS('',3,(#49402,#49403,#49404,#49405,#49406),
 .UNSPECIFIED.,.F.,.F.,(4,1,4),(0.0011710920609951,0.0023421841219902,0.00236041305987884),
 .UNSPECIFIED.);
#1385=B_SPLINE_CURVE_WITH_KNOTS('',3,(#49407,#49408,#49409,#49410),
 .UNSPECIFIED.,.F.,.F.,(4,4),(2.2209506323702E-5,0.0011710920609951),
 .UNSPECIFIED.);
#1386=B_SPLINE_CURVE_WITH_KNOTS('',3,(#49450,#49451,#49452,#49453,#49454,
#49455,#49456,#49457,#49458,#49459,#49460),.UNSPECIFIED.,.F.,.F.,(4,1,1,
1,1,1,1,1,4),(2.16840434497101E-19,0.00133638350122092,0.00267276700244185,
0.00400915050366277,0.0053455340048837,0.00668191750610462,0.00801830100732555,
0.00935468450854647,0.0106661079505723),.UNSPECIFIED.);
#1387=B_SPLINE_CURVE_WITH_KNOTS('',3,(#49466,#49467,#49468,#49469),
 .UNSPECIFIED.,.F.,.F.,(4,4),(0.00821090794688191,0.00936873648796083),
 .UNSPECIFIED.);
#1388=B_SPLINE_CURVE_WITH_KNOTS('',3,(#49471,#49472,#49473,#49474,#49475),
 .UNSPECIFIED.,.F.,.F.,(4,1,4),(0.00704598836790659,0.00819764442696573,
0.00821090794688191),.UNSPECIFIED.);
#1389=B_SPLINE_CURVE_WITH_KNOTS('',3,(#49477,#49478,#49479,#49480,#49481),
 .UNSPECIFIED.,.F.,.F.,(4,1,4),(0.00585546030497552,0.00702655236597062,
0.00704598836790659),.UNSPECIFIED.);
#1390=B_SPLINE_CURVE_WITH_KNOTS('',3,(#49483,#49484,#49485,#49486,#49487),
 .UNSPECIFIED.,.F.,.F.,(4,1,4),(0.00352617550117701,0.00468436824398042,
0.00585546030497552),.UNSPECIFIED.);
#1391=B_SPLINE_CURVE_WITH_KNOTS('',3,(#49489,#49490,#49491,#49492,#49493),
 .UNSPECIFIED.,.F.,.F.,(4,1,4),(0.00236041305988171,0.00351327618298531,
0.00352617550117701),.UNSPECIFIED.);
#1392=B_SPLINE_CURVE_WITH_KNOTS('',3,(#49495,#49496,#49497,#49498,#49499),
 .UNSPECIFIED.,.F.,.F.,(4,1,4),(0.0011710920609951,0.00234218412199021,
0.00236041305988171),.UNSPECIFIED.);
#1393=B_SPLINE_CURVE_WITH_KNOTS('',3,(#49500,#49501,#49502,#49503),
 .UNSPECIFIED.,.F.,.F.,(4,4),(2.22095063237639E-5,0.0011710920609951),
 .UNSPECIFIED.);
#1394=B_SPLINE_CURVE_WITH_KNOTS('',3,(#49543,#49544,#49545,#49546,#49547,
#49548,#49549,#49550,#49551,#49552,#49553),.UNSPECIFIED.,.F.,.F.,(4,1,1,
1,1,1,1,1,4),(2.16840434497101E-19,0.00133638350122091,0.00267276700244182,
0.00400915050366274,0.00534553400488365,0.00668191750610456,0.00801830100732547,
0.00935468450854638,0.0106661079505722),.UNSPECIFIED.);
#1395=B_SPLINE_CURVE_WITH_KNOTS('',3,(#49559,#49560,#49561,#49562),
 .UNSPECIFIED.,.F.,.F.,(4,4),(0.00821090794688314,0.00936873648796083),
 .UNSPECIFIED.);
#1396=B_SPLINE_CURVE_WITH_KNOTS('',3,(#49564,#49565,#49566,#49567,#49568),
 .UNSPECIFIED.,.F.,.F.,(4,1,4),(0.00704598836790498,0.00819764442696573,
0.00821090794688314),.UNSPECIFIED.);
#1397=B_SPLINE_CURVE_WITH_KNOTS('',3,(#49570,#49571,#49572,#49573,#49574),
 .UNSPECIFIED.,.F.,.F.,(4,1,4),(0.00585546030497552,0.00702655236597062,
0.00704598836790498),.UNSPECIFIED.);
#1398=B_SPLINE_CURVE_WITH_KNOTS('',3,(#49576,#49577,#49578,#49579,#49580),
 .UNSPECIFIED.,.F.,.F.,(4,1,4),(0.0035261755011782,0.00468436824398041,
0.00585546030497552),.UNSPECIFIED.);
#1399=B_SPLINE_CURVE_WITH_KNOTS('',3,(#49582,#49583,#49584,#49585,#49586),
 .UNSPECIFIED.,.F.,.F.,(4,1,4),(0.00236041305988064,0.00351327618298531,
0.0035261755011782),.UNSPECIFIED.);
#1400=B_SPLINE_CURVE_WITH_KNOTS('',3,(#49588,#49589,#49590,#49591,#49592),
 .UNSPECIFIED.,.F.,.F.,(4,1,4),(0.0011710920609951,0.00234218412199021,
0.00236041305988064),.UNSPECIFIED.);
#1401=B_SPLINE_CURVE_WITH_KNOTS('',3,(#49593,#49594,#49595,#49596),
 .UNSPECIFIED.,.F.,.F.,(4,4),(2.2209506323727E-5,0.0011710920609951),
 .UNSPECIFIED.);
#1402=B_SPLINE_CURVE_WITH_KNOTS('',3,(#49600,#49601,#49602,#49603),
 .UNSPECIFIED.,.F.,.F.,(4,4),(0.,0.000682262674512534),.UNSPECIFIED.);
#1403=B_SPLINE_CURVE_WITH_KNOTS('',3,(#49668,#49669,#49670,#49671,#49672,
#49673),.UNSPECIFIED.,.F.,.F.,(4,2,4),(-0.101895978906481,-0.0984710269726971,
-0.0896897186466305),.UNSPECIFIED.);
#1404=B_SPLINE_CURVE_WITH_KNOTS('',3,(#49680,#49681,#49682,#49683,#49684,
#49685,#49686,#49687,#49688,#49689),.UNSPECIFIED.,.F.,.F.,(4,2,2,2,4),(0.00701311257563557,
0.010982820742087,0.0253526872842843,0.0698643291505208,0.0772205186033042),
 .UNSPECIFIED.);
#1405=B_SPLINE_CURVE_WITH_KNOTS('',3,(#49702,#49703,#49704,#49705,#49706,
#49707,#49708,#49709,#49710,#49711,#49712,#49713,#49714),.UNSPECIFIED.,
 .F.,.F.,(4,3,3,3,4),(0.0824582419012307,0.166224116038678,0.249986773069777,
0.333749430179514,0.417515304238324),.UNSPECIFIED.);
#1406=B_SPLINE_CURVE_WITH_KNOTS('',3,(#49720,#49721,#49722,#49723,#49724,
#49725,#49726,#49727,#49728,#49729,#49730,#49731,#49732),.UNSPECIFIED.,
 .F.,.F.,(4,3,3,3,4),(0.582140268332509,0.666078166051184,0.750012831472539,
0.833947496910044,0.91788539461257),.UNSPECIFIED.);
#1407=B_SPLINE_CURVE_WITH_KNOTS('',3,(#49741,#49742,#49743,#49744),
 .UNSPECIFIED.,.F.,.F.,(4,4),(0.0106661079505722,0.0106910680097673),
 .UNSPECIFIED.);
#1408=B_SPLINE_CURVE_WITH_KNOTS('',3,(#49745,#49746,#49747,#49748),
 .UNSPECIFIED.,.F.,.F.,(4,4),(0.0106661079505723,0.0106910680097674),
 .UNSPECIFIED.);
#1409=B_SPLINE_CURVE_WITH_KNOTS('',3,(#49749,#49750,#49751,#49752),
 .UNSPECIFIED.,.F.,.F.,(4,4),(0.0106661079505718,0.0106910680097674),
 .UNSPECIFIED.);
#1410=B_SPLINE_CURVE_WITH_KNOTS('',3,(#49753,#49754,#49755,#49756),
 .UNSPECIFIED.,.F.,.F.,(4,4),(0.0106661079505719,0.0106910680097674),
 .UNSPECIFIED.);
#1411=B_SPLINE_CURVE_WITH_KNOTS('',3,(#49757,#49758,#49759,#49760),
 .UNSPECIFIED.,.F.,.F.,(4,4),(0.0106661079505718,0.0106910680097673),
 .UNSPECIFIED.);
#1412=B_SPLINE_CURVE_WITH_KNOTS('',3,(#49824,#49825,#49826,#49827,#49828,
#49829,#49830),.UNSPECIFIED.,.F.,.F.,(4,3,4),(2.16840434497101E-19,0.00581319522920539,
0.0116263904584108),.UNSPECIFIED.);
#1413=B_SPLINE_CURVE_WITH_KNOTS('',3,(#49832,#49833,#49834,#49835),
 .UNSPECIFIED.,.F.,.F.,(4,4),(2.79715755706988E-17,0.00267897349074099),
 .UNSPECIFIED.);
#1414=B_SPLINE_CURVE_WITH_KNOTS('',3,(#49851,#49852,#49853,#49854),
 .UNSPECIFIED.,.F.,.F.,(4,4),(3.43963882861591E-14,0.0026798705859963),
 .UNSPECIFIED.);
#1415=B_SPLINE_CURVE_WITH_KNOTS('',3,(#49856,#49857,#49858,#49859,#49860,
#49861,#49862),.UNSPECIFIED.,.F.,.F.,(4,3,4),(0.0153783179950603,0.0211672261179413,
0.0269561342408223),.UNSPECIFIED.);
#1416=B_SPLINE_CURVE_WITH_KNOTS('',3,(#49863,#49864,#49865,#49866,#49867,
#49868,#49869,#49870,#49871,#49872,#49873,#49874,#49875),.UNSPECIFIED.,
 .F.,.F.,(4,3,3,3,4),(1.62471150819444E-9,0.371962494639839,0.5,0.868119627457051,
0.999999997610495),.UNSPECIFIED.);
#1417=B_SPLINE_CURVE_WITH_KNOTS('',3,(#49934,#49935,#49936,#49937,#49938,
#49939,#49940,#49941,#49942,#49943,#49944,#49945,#49946,#49947,#49948,#49949),
 .UNSPECIFIED.,.F.,.F.,(4,3,3,3,3,4),(1.63653485417008E-17,0.000871734875690096,
0.00174346975138018,0.00261520462707026,0.0030510720649153,0.00348693950276033),
 .UNSPECIFIED.);
#1418=B_SPLINE_CURVE_WITH_KNOTS('',3,(#49951,#49952,#49953,#49954,#49955,
#49956,#49957,#49958,#49959,#49960,#49961,#49962,#49963,#49964,#49965,#49966),
 .UNSPECIFIED.,.F.,.F.,(4,3,3,3,3,4),(0.,0.25,0.375,0.5,0.75,1.),
 .UNSPECIFIED.);
#1419=B_SPLINE_CURVE_WITH_KNOTS('',3,(#49970,#49971,#49972,#49973,#49974,
#49975,#49976,#49977,#49978,#49979,#49980,#49981,#49982),.UNSPECIFIED.,
 .F.,.F.,(4,3,3,3,4),(3.26962013452912E-17,0.000593256852872857,0.00118651370574568,
0.00177977055861851,0.00237302741149133),.UNSPECIFIED.);
#1420=B_SPLINE_CURVE_WITH_KNOTS('',3,(#49993,#49994,#49995,#49996,#49997,
#49998,#49999,#50000,#50001,#50002,#50003,#50004,#50005),.UNSPECIFIED.,
 .F.,.F.,(4,3,3,3,4),(1.56949960400744E-16,0.000586676321783765,0.00117335264356737,
0.00176002896535098,0.00234670528713459),.UNSPECIFIED.);
#1421=B_SPLINE_CURVE_WITH_KNOTS('',3,(#50009,#50010,#50011,#50012),
 .UNSPECIFIED.,.F.,.F.,(4,4),(0.,1.),.UNSPECIFIED.);
#1422=B_SPLINE_CURVE_WITH_KNOTS('',3,(#50014,#50015,#50016,#50017),
 .UNSPECIFIED.,.F.,.F.,(4,4),(0.,1.),.UNSPECIFIED.);
#1423=B_SPLINE_CURVE_WITH_KNOTS('',3,(#50019,#50020,#50021,#50022,#50023,
#50024,#50025,#50026,#50027,#50028,#50029,#50030,#50031,#50032,#50033,#50034),
 .UNSPECIFIED.,.F.,.F.,(4,3,3,3,3,4),(1.23884035470014E-17,0.000436227682635904,
0.000872455365271796,0.00174491073054358,0.00261736609581536,0.00348982146108715),
 .UNSPECIFIED.);
#1424=B_SPLINE_CURVE_WITH_KNOTS('',3,(#50071,#50072,#50073,#50074,#50075,
#50076,#50077,#50078,#50079,#50080),.UNSPECIFIED.,.F.,.F.,(4,3,3,4),(0.,
0.250198742533901,0.484142189377901,0.72625720196945),.UNSPECIFIED.);
#1425=B_SPLINE_CURVE_WITH_KNOTS('',3,(#50082,#50083,#50084,#50085,#50086,
#50087,#50088,#50089,#50090,#50091,#50092,#50093,#50094,#50095,#50096,#50097,
#50098,#50099,#50100,#50101,#50102,#50103,#50104,#50105,#50106,#50107,#50108,
#50109,#50110,#50111,#50112,#50113,#50114,#50115,#50116,#50117,#50118,#50119,
#50120,#50121,#50122,#50123,#50124,#50125,#50126,#50127,#50128,#50129,#50130,
#50131,#50132,#50133,#50134,#50135,#50136),.UNSPECIFIED.,.F.,.F.,(4,3,3,
3,3,3,3,3,3,3,3,3,3,3,3,3,3,3,4),(2.6220077343514E-7,0.0203152518413343,
0.134046967430369,0.239869415550571,0.25,0.339303542480863,0.375,0.5,0.523390970218302,
0.625,0.6875,0.69519800169401,0.71875,0.75,0.78125,0.8125,0.875,0.884458267348107,
1.),.UNSPECIFIED.);
#1426=B_SPLINE_CURVE_WITH_KNOTS('',3,(#50138,#50139,#50140,#50141,#50142,
#50143,#50144,#50145,#50146,#50147,#50148,#50149,#50150,#50151,#50152,#50153,
#50154,#50155,#50156,#50157,#50158,#50159,#50160,#50161,#50162,#50163,#50164,
#50165,#50166,#50167,#50168,#50169,#50170,#50171,#50172,#50173,#50174,#50175,
#50176,#50177,#50178,#50179,#50180,#50181,#50182,#50183,#50184,#50185,#50186,
#50187,#50188,#50189,#50190,#50191,#50192,#50193,#50194,#50195,#50196,#50197,
#50198,#50199,#50200,#50201,#50202,#50203,#50204),.UNSPECIFIED.,.F.,.F.,
(4,3,3,3,3,3,3,3,3,3,3,3,3,3,3,3,3,3,3,3,3,3,4),(0.,0.0625,0.125,0.182156208275604,
0.1875,0.25,0.31138954419103,0.3125,0.375,0.41421262630946,0.4375,0.5,0.5625,
0.586017101931546,0.625,0.6875,0.688684714649581,0.75,0.8125,0.81792114283053,
0.875,0.9375,1.),.UNSPECIFIED.);
#1427=B_SPLINE_CURVE_WITH_KNOTS('',3,(#50206,#50207,#50208,#50209,#50210,
#50211,#50212,#50213,#50214,#50215,#50216,#50217,#50218,#50219,#50220,#50221,
#50222,#50223,#50224,#50225,#50226,#50227,#50228,#50229,#50230,#50231,#50232,
#50233,#50234,#50235,#50236,#50237,#50238,#50239,#50240,#50241,#50242,#50243,
#50244,#50245,#50246,#50247,#50248,#50249,#50250,#50251,#50252,#50253,#50254,
#50255,#50256,#50257),.UNSPECIFIED.,.F.,.F.,(4,3,3,3,3,3,3,3,3,3,3,3,3,
3,3,3,3,4),(0.,0.113955744298881,0.125,0.1875,0.21875,0.25,0.28125,0.30198702723121,
0.3125,0.375,0.471780754133228,0.5,0.625,0.654220290439613,0.75,0.856955738520236,
0.969024551611296,0.999999731075503),.UNSPECIFIED.);
#1428=B_SPLINE_CURVE_WITH_KNOTS('',3,(#50258,#50259,#50260,#50261,#50262,
#50263,#50264,#50265,#50266,#50267,#50268,#50269,#50270,#50271,#50272,#50273,
#50274,#50275,#50276,#50277,#50278,#50279,#50280,#50281,#50282,#50283,#50284,
#50285,#50286,#50287,#50288,#50289,#50290,#50291,#50292,#50293,#50294,#50295,
#50296,#50297,#50298,#50299,#50300,#50301,#50302,#50303,#50304,#50305,#50306,
#50307,#50308,#50309,#50310,#50311,#50312,#50313,#50314,#50315,#50316,#50317,
#50318,#50319,#50320,#50321,#50322,#50323,#50324,#50325,#50326,#50327),
 .UNSPECIFIED.,.F.,.F.,(4,3,3,3,3,3,3,3,3,3,3,3,3,3,3,3,3,3,3,3,3,3,3,4),
(0.,0.0625,0.09375,0.109375,0.1171875,0.125,0.140625,0.15625,0.1875,0.25,
0.3125,0.375,0.4375,0.5,0.5625,0.625,0.65625,0.6875,0.703125,0.71875,0.75,
0.8125,0.875,1.),.UNSPECIFIED.);
#1429=B_SPLINE_CURVE_WITH_KNOTS('',3,(#50358,#50359,#50360,#50361,#50362,
#50363,#50364,#50365,#50366,#50367,#50368,#50369,#50370,#50371,#50372,#50373,
#50374,#50375,#50376,#50377,#50378,#50379,#50380,#50381,#50382,#50383,#50384,
#50385,#50386,#50387,#50388,#50389,#50390,#50391,#50392,#50393,#50394,#50395,
#50396,#50397,#50398,#50399,#50400,#50401,#50402,#50403,#50404,#50405,#50406,
#50407,#50408,#50409,#50410,#50411,#50412,#50413,#50414,#50415,#50416,#50417,
#50418),.UNSPECIFIED.,.F.,.F.,(4,3,3,3,3,3,3,3,3,3,3,3,3,3,3,3,3,3,3,3,
4),(0.,0.125,0.18211780806116,0.21875,0.232943528841739,0.25,0.28125,0.3125,
0.32477251801541,0.375,0.4375,0.451086136346817,0.5,0.5625,0.589820371942222,
0.625,0.740436596594459,0.75,0.823581534574207,0.912738301505326,0.999999265653549),
 .UNSPECIFIED.);
#1430=B_SPLINE_CURVE_WITH_KNOTS('',3,(#50419,#50420,#50421,#50422,#50423,
#50424,#50425,#50426,#50427,#50428,#50429,#50430,#50431,#50432,#50433,#50434,
#50435,#50436,#50437,#50438,#50439,#50440,#50441,#50442,#50443,#50444,#50445,
#50446,#50447,#50448,#50449,#50450,#50451,#50452,#50453,#50454,#50455,#50456,
#50457,#50458,#50459,#50460,#50461,#50462,#50463,#50464,#50465,#50466,#50467,
#50468,#50469,#50470),.UNSPECIFIED.,.F.,.F.,(4,3,3,3,3,3,3,3,3,3,3,3,3,
3,3,3,3,4),(1.08343486081908E-7,0.125,0.1875,0.25,0.375,0.4375,0.46875,
0.5,0.53125,0.5625,0.625,0.6875,0.75,0.8125,0.875,0.90625,0.9375,1.),
 .UNSPECIFIED.);
#1431=B_SPLINE_CURVE_WITH_KNOTS('',3,(#50472,#50473,#50474,#50475,#50476,
#50477,#50478,#50479,#50480,#50481,#50482,#50483,#50484,#50485,#50486,#50487,
#50488,#50489,#50490,#50491,#50492,#50493,#50494,#50495,#50496,#50497,#50498,
#50499,#50500,#50501,#50502,#50503,#50504,#50505,#50506,#50507,#50508),
 .UNSPECIFIED.,.F.,.F.,(4,3,3,3,3,3,3,3,3,3,3,3,4),(0.,0.0625,0.125,0.1875,
0.25,0.375,0.5,0.625,0.75,0.78125,0.8125,0.875,0.999999860772477),
 .UNSPECIFIED.);
#1432=B_SPLINE_CURVE_WITH_KNOTS('',3,(#50510,#50511,#50512,#50513,#50514,
#50515,#50516,#50517,#50518,#50519,#50520,#50521,#50522,#50523,#50524,#50525,
#50526,#50527,#50528,#50529,#50530,#50531,#50532,#50533,#50534,#50535,#50536,
#50537,#50538,#50539,#50540,#50541,#50542,#50543,#50544,#50545,#50546,#50547,
#50548,#50549,#50550,#50551,#50552,#50553,#50554,#50555,#50556,#50557,#50558,
#50559,#50560,#50561,#50562,#50563,#50564,#50565,#50566,#50567,#50568,#50569,
#50570),.UNSPECIFIED.,.F.,.F.,(4,3,3,3,3,3,3,3,3,3,3,3,3,3,3,3,3,3,3,3,
4),(7.54076708606675E-7,0.0890838043400427,0.177519647918873,0.25,0.260152278755688,
0.375,0.410146430846909,0.4375,0.5,0.548806008922445,0.5625,0.625,0.675295564779425,
0.6875,0.71875,0.75,0.768236511403328,0.78125,0.829706236970379,0.875,1.),
 .UNSPECIFIED.);
#1433=B_SPLINE_CURVE_WITH_KNOTS('',3,(#50571,#50572,#50573,#50574,#50575,
#50576,#50577,#50578,#50579,#50580,#50581,#50582,#50583,#50584,#50585,#50586,
#50587,#50588,#50589,#50590,#50591,#50592,#50593,#50594,#50595,#50596,#50597,
#50598,#50599,#50600,#50601,#50602,#50603,#50604,#50605,#50606,#50607,#50608,
#50609,#50610,#50611,#50612,#50613,#50614,#50615,#50616,#50617,#50618,#50619),
 .UNSPECIFIED.,.F.,.F.,(4,3,3,3,3,3,3,3,3,3,3,3,3,3,3,3,4),(0.,0.125,0.1875,
0.25,0.299171599130771,0.3125,0.375,0.405133032227414,0.5,0.597278855307766,
0.625,0.6875,0.702732497560042,0.75,0.8125,0.875,1.),.UNSPECIFIED.);
#1434=B_SPLINE_CURVE_WITH_KNOTS('',3,(#50662,#50663,#50664,#50665),
 .UNSPECIFIED.,.F.,.F.,(4,4),(4.48352082164622E-10,0.999999999778094),
 .UNSPECIFIED.);
#1435=B_SPLINE_CURVE_WITH_KNOTS('',3,(#50669,#50670,#50671,#50672,#50673,
#50674,#50675,#50676,#50677,#50678,#50679,#50680,#50681,#50682,#50683,#50684,
#50685,#50686,#50687,#50688,#50689,#50690,#50691,#50692,#50693,#50694,#50695,
#50696,#50697,#50698,#50699,#50700,#50701,#50702,#50703,#50704,#50705,#50706,
#50707,#50708,#50709,#50710,#50711,#50712,#50713,#50714,#50715,#50716,#50717,
#50718,#50719,#50720,#50721,#50722,#50723,#50724,#50725,#50726,#50727,#50728,
#50729,#50730,#50731,#50732,#50733,#50734,#50735,#50736,#50737,#50738,#50739,
#50740,#50741,#50742,#50743,#50744,#50745,#50746,#50747,#50748,#50749,#50750,
#50751,#50752,#50753,#50754,#50755,#50756,#50757,#50758,#50759,#50760,#50761,
#50762,#50763,#50764,#50765,#50766,#50767,#50768,#50769,#50770,#50771,#50772,
#50773,#50774,#50775,#50776,#50777,#50778,#50779,#50780,#50781,#50782,#50783,
#50784,#50785,#50786,#50787,#50788,#50789,#50790,#50791,#50792,#50793,#50794,
#50795),.UNSPECIFIED.,.F.,.F.,(4,3,3,3,3,3,3,3,3,3,3,3,3,3,3,3,3,3,3,3,
3,3,3,3,3,3,3,3,3,3,3,3,3,3,3,3,3,3,3,3,3,3,4),(0.,0.0458053754614711,0.0750691510926553,
0.10248161995056,0.135574456705558,0.183221501845885,0.215541126384413,
0.235200596896411,0.25121949529829,0.270280464799092,0.297803561834966,
0.3125,0.34375,0.375,0.389701511535224,0.40625,0.445507570744879,0.477590011279423,
0.506318202949039,0.54013120645178,0.5625,0.585957017411357,0.625,0.6875,
0.703125,0.71875,0.75,0.780133441203814,0.78125,0.796875,0.813355261544154,
0.831836748639714,0.84375,0.873025477612267,0.875,0.890625,0.912254662027643,
0.926757684009806,0.940434508371303,0.953125,0.964809427833706,0.96875,
0.999999999954988),.UNSPECIFIED.);
#1436=B_SPLINE_CURVE_WITH_KNOTS('',3,(#50797,#50798,#50799,#50800,#50801,
#50802,#50803,#50804,#50805,#50806,#50807,#50808),.UNSPECIFIED.,.F.,.F.,
(4,1,1,1,1,1,1,1,1,4),(0.,0.125,0.25,0.375,0.5,0.5625,0.625,0.75,0.875,
1.),.UNSPECIFIED.);
#1437=B_SPLINE_CURVE_WITH_KNOTS('',3,(#50809,#50810,#50811,#50812,#50813,
#50814,#50815,#50816,#50817,#50818,#50819,#50820,#50821,#50822,#50823,#50824,
#50825,#50826,#50827,#50828,#50829,#50830,#50831,#50832,#50833,#50834,#50835,
#50836,#50837,#50838,#50839,#50840,#50841,#50842,#50843,#50844,#50845,#50846,
#50847,#50848,#50849,#50850,#50851,#50852,#50853,#50854),.UNSPECIFIED.,
 .F.,.F.,(4,3,3,3,3,3,3,3,3,3,3,3,3,3,3,4),(0.,0.0625,0.125,0.15625,0.1875,
0.25,0.375,0.4375,0.5,0.5625,0.625,0.6875,0.75,0.875,0.977913764805899,
1.),.UNSPECIFIED.);
#1438=B_SPLINE_CURVE_WITH_KNOTS('',3,(#50855,#50856,#50857,#50858),
 .UNSPECIFIED.,.F.,.F.,(4,4),(0.,0.997240928837636),.UNSPECIFIED.);
#1439=B_SPLINE_CURVE_WITH_KNOTS('',3,(#50935,#50936,#50937,#50938,#50939,
#50940,#50941,#50942,#50943,#50944,#50945,#50946,#50947,#50948,#50949,#50950,
#50951,#50952,#50953,#50954,#50955,#50956,#50957,#50958,#50959),
 .UNSPECIFIED.,.F.,.F.,(4,3,3,3,3,3,3,3,4),(2.03487242492536E-9,0.0258251891945382,
0.164170751422891,0.302802438327866,0.441718638276399,0.580627042706572,
0.719815414030138,0.859281996108356,1.),.UNSPECIFIED.);
#1440=B_SPLINE_CURVE_WITH_KNOTS('',3,(#50961,#50962,#50963,#50964,#50965,
#50966,#50967,#50968,#50969),.UNSPECIFIED.,.F.,.F.,(4,1,1,1,1,1,4),(7.70326878569046E-5,
0.00437432926208278,0.008671626066204,0.0108202744682646,0.0129689228703252,
0.0151175712723858,0.0172662196744464),.UNSPECIFIED.);
#1441=B_SPLINE_CURVE_WITH_KNOTS('',3,(#50970,#50971,#50972,#50973,#50974,
#50975,#50976,#50977,#50978,#50979,#50980,#50981,#50982,#50983,#50984,#50985,
#50986,#50987,#50988,#50989,#50990,#50991,#50992,#50993,#50994,#50995,#50996,
#50997,#50998,#50999,#51000,#51001,#51002,#51003,#51004,#51005,#51006,#51007,
#51008,#51009,#51010,#51011,#51012,#51013,#51014,#51015,#51016,#51017,#51018,
#51019,#51020,#51021,#51022,#51023,#51024,#51025,#51026,#51027,#51028,#51029,
#51030,#51031,#51032,#51033,#51034,#51035,#51036),.UNSPECIFIED.,.F.,.F.,
(4,3,3,3,3,3,3,3,3,3,3,3,3,3,3,3,3,3,3,3,3,3,4),(1.42349606405191E-7,0.125,
0.1875,0.25,0.3125,0.375,0.4375,0.46875,0.484375,0.5,0.515625,0.53125,0.5625,
0.625,0.6875,0.75,0.8125,0.832640388956925,0.84375,0.875,0.90625,0.9375,
1.),.UNSPECIFIED.);
#1442=B_SPLINE_CURVE_WITH_KNOTS('',3,(#51038,#51039,#51040,#51041,#51042,
#51043,#51044,#51045,#51046,#51047,#51048,#51049,#51050,#51051,#51052,#51053,
#51054,#51055,#51056,#51057,#51058,#51059,#51060,#51061,#51062),
 .UNSPECIFIED.,.F.,.F.,(4,3,3,3,3,3,3,3,4),(0.,0.0171992441380122,0.25,
0.5,0.625,0.75,0.8125,0.875,1.),.UNSPECIFIED.);
#1443=B_SPLINE_CURVE_WITH_KNOTS('',3,(#51064,#51065,#51066,#51067,#51068,
#51069,#51070,#51071,#51072,#51073,#51074,#51075,#51076),.UNSPECIFIED.,
 .F.,.F.,(4,3,3,3,4),(0.,0.500000000000001,0.548723791104437,0.75,1.),
 .UNSPECIFIED.);
#1444=B_SPLINE_CURVE_WITH_KNOTS('',3,(#51077,#51078,#51079,#51080,#51081,
#51082,#51083,#51084),.UNSPECIFIED.,.F.,.F.,(4,1,1,1,1,4),(-5.99999999944752E-8,
0.00312786895657466,0.00469183343486199,0.00625579791314932,0.00938372686972398,
0.0125116558262986),.UNSPECIFIED.);
#1445=B_SPLINE_CURVE_WITH_KNOTS('',3,(#51127,#51128,#51129,#51130,#51131,
#51132,#51133,#51134,#51135,#51136,#51137,#51138,#51139,#51140,#51141,#51142,
#51143,#51144,#51145,#51146,#51147,#51148,#51149,#51150,#51151,#51152,#51153,
#51154,#51155,#51156,#51157,#51158,#51159,#51160,#51161,#51162,#51163,#51164,
#51165,#51166,#51167,#51168,#51169,#51170,#51171,#51172,#51173,#51174,#51175,
#51176,#51177,#51178,#51179,#51180,#51181,#51182,#51183,#51184,#51185,#51186,
#51187,#51188,#51189,#51190,#51191,#51192,#51193,#51194,#51195,#51196,#51197,
#51198,#51199,#51200,#51201,#51202,#51203,#51204,#51205,#51206,#51207,#51208,
#51209,#51210,#51211,#51212,#51213,#51214,#51215,#51216,#51217,#51218,#51219,
#51220,#51221,#51222,#51223,#51224,#51225,#51226,#51227,#51228,#51229,#51230,
#51231,#51232,#51233,#51234,#51235,#51236,#51237,#51238,#51239,#51240,#51241,
#51242,#51243,#51244,#51245,#51246,#51247,#51248,#51249,#51250,#51251,#51252,
#51253,#51254,#51255,#51256,#51257,#51258,#51259,#51260,#51261,#51262,#51263,
#51264,#51265,#51266,#51267,#51268,#51269,#51270,#51271,#51272,#51273,#51274),
 .UNSPECIFIED.,.F.,.F.,(4,3,3,3,3,3,3,3,3,3,3,3,3,3,3,3,3,3,3,3,3,3,3,3,
3,3,3,3,3,3,3,3,3,3,3,3,3,3,3,3,3,3,3,3,3,3,3,3,3,4),(0.,0.0625,0.09375,
0.124731584851994,0.125,0.15625,0.185898086488356,0.1875,0.21875,0.246713282675617,
0.25,0.28125,0.308162129481387,0.328945253391501,0.346341543597235,0.359375,
0.370641832386322,0.375,0.3828125,0.390625,0.3984375,0.40625,0.4140625,
0.421875,0.430538691367311,0.4375,0.46875,0.492575847998397,0.5,0.53125,
0.5625,0.59375,0.609375,0.618852153197554,0.625,0.644295096358991,0.671432424588419,
0.706945894626813,0.730283133511903,0.734375,0.74707850512236,0.75,0.765625,
0.78125,0.84375,0.875,0.876135893436369,0.9375,0.939588219697389,1.),
 .UNSPECIFIED.);
#1446=B_SPLINE_CURVE_WITH_KNOTS('',3,(#51275,#51276,#51277,#51278,#51279,
#51280,#51281,#51282,#51283,#51284,#51285,#51286,#51287),.UNSPECIFIED.,
 .F.,.F.,(4,3,3,3,4),(2.79419382013459E-10,0.290816211170589,0.60141503799362,
0.93668173505155,0.999999998265381),.UNSPECIFIED.);
#1447=B_SPLINE_CURVE_WITH_KNOTS('',3,(#51288,#51289,#51290,#51291,#51292,
#51293,#51294,#51295,#51296,#51297,#51298,#51299,#51300,#51301,#51302,#51303,
#51304,#51305,#51306,#51307,#51308,#51309,#51310,#51311,#51312,#51313,#51314,
#51315,#51316,#51317,#51318,#51319,#51320,#51321,#51322,#51323,#51324,#51325,
#51326,#51327,#51328,#51329,#51330,#51331,#51332,#51333,#51334,#51335,#51336,
#51337,#51338,#51339,#51340,#51341,#51342,#51343,#51344,#51345,#51346,#51347,
#51348),.UNSPECIFIED.,.F.,.F.,(4,3,3,3,3,3,3,3,3,3,3,3,3,3,3,3,3,3,3,3,
4),(0.,0.0625,0.078125,0.09375,0.125,0.15625,0.160643478189123,0.1875,0.25,
0.3125,0.375,0.4375,0.5,0.53125,0.546875,0.5625,0.59375,0.625,0.6875,0.75,
0.999999873926191),.UNSPECIFIED.);
#1448=B_SPLINE_CURVE_WITH_KNOTS('',3,(#51353,#51354,#51355,#51356),
 .UNSPECIFIED.,.F.,.F.,(4,4),(0.,2.22095063237474E-5),.UNSPECIFIED.);
#1449=B_SPLINE_CURVE_WITH_KNOTS('',3,(#51358,#51359,#51360,#51361),
 .UNSPECIFIED.,.F.,.F.,(4,4),(0.,2.22095063236846E-5),.UNSPECIFIED.);
#1450=B_SPLINE_CURVE_WITH_KNOTS('',3,(#51363,#51364,#51365,#51366),
 .UNSPECIFIED.,.F.,.F.,(4,4),(0.,2.2209506323702E-5),.UNSPECIFIED.);
#1451=B_SPLINE_CURVE_WITH_KNOTS('',3,(#51368,#51369,#51370,#51371),
 .UNSPECIFIED.,.F.,.F.,(4,4),(0.,2.22095063237639E-5),.UNSPECIFIED.);
#1452=B_SPLINE_CURVE_WITH_KNOTS('',3,(#51373,#51374,#51375,#51376),
 .UNSPECIFIED.,.F.,.F.,(4,4),(0.,2.2209506323727E-5),.UNSPECIFIED.);
#1453=B_SPLINE_CURVE_WITH_KNOTS('',3,(#51397,#51398,#51399,#51400,#51401,
#51402,#51403),.UNSPECIFIED.,.F.,.F.,(4,3,4),(0.,0.125,0.25),
 .UNSPECIFIED.);
#1454=B_SPLINE_CURVE_WITH_KNOTS('',3,(#51405,#51406,#51407,#51408,#51409,
#51410,#51411,#51412,#51413,#51414,#51415,#51416,#51417,#51418,#51419,#51420,
#51421,#51422,#51423,#51424,#51425,#51426,#51427,#51428,#51429,#51430,#51431,
#51432,#51433,#51434,#51435,#51436,#51437,#51438,#51439,#51440,#51441,#51442,
#51443,#51444,#51445,#51446,#51447,#51448,#51449,#51450),.UNSPECIFIED.,
 .F.,.F.,(4,3,3,3,3,3,3,3,3,3,3,3,3,3,3,4),(0.25,0.3125,0.375,0.4375,0.46875,
0.4765625,0.484375,0.5,0.515625,0.53125,0.5625,0.625,0.6875,0.75,0.875,
1.),.UNSPECIFIED.);
#1455=B_SPLINE_CURVE_WITH_KNOTS('',3,(#51452,#51453,#51454,#51455,#51456,
#51457,#51458,#51459,#51460,#51461,#51462,#51463,#51464),.UNSPECIFIED.,
 .F.,.F.,(4,3,3,3,4),(3.36788025480501E-14,0.351091870377537,0.5,0.845889958604177,
0.999999999999961),.UNSPECIFIED.);
#1456=B_SPLINE_CURVE_WITH_KNOTS('',3,(#51466,#51467,#51468,#51469,#51470,
#51471,#51472,#51473,#51474,#51475,#51476,#51477,#51478,#51479,#51480,#51481,
#51482,#51483,#51484,#51485,#51486,#51487,#51488,#51489,#51490,#51491,#51492,
#51493,#51494,#51495,#51496,#51497,#51498,#51499,#51500,#51501,#51502,#51503,
#51504,#51505,#51506,#51507,#51508,#51509,#51510,#51511,#51512,#51513,#51514),
 .UNSPECIFIED.,.F.,.F.,(4,3,3,3,3,3,3,3,3,3,3,3,3,3,3,3,4),(1.91266793240995E-6,
0.125,0.25,0.3125,0.375,0.4375,0.46875,0.484375,0.5,0.515625,0.53125,0.53515625,
0.53857421875,0.5625,0.625,0.6875,0.75),.UNSPECIFIED.);
#1457=B_SPLINE_CURVE_WITH_KNOTS('',3,(#51516,#51517,#51518,#51519,#51520,
#51521,#51522),.UNSPECIFIED.,.F.,.F.,(4,3,4),(0.75,0.875,1.),
 .UNSPECIFIED.);
#1458=B_SPLINE_CURVE_WITH_KNOTS('',3,(#51524,#51525,#51526,#51527),
 .UNSPECIFIED.,.F.,.F.,(4,4),(7.33287537516016E-16,0.00234848012465154),
 .UNSPECIFIED.);
#1459=B_SPLINE_CURVE_WITH_KNOTS('',3,(#51538,#51539,#51540,#51541),
 .UNSPECIFIED.,.F.,.F.,(4,4),(1.73200015566965E-14,0.00232242609217698),
 .UNSPECIFIED.);
#1460=B_SPLINE_CURVE_WITH_KNOTS('',3,(#51725,#51726,#51727,#51728,#51729,
#51730,#51731,#51732,#51733,#51734,#51735,#51736,#51737,#51738,#51739,#51740,
#51741,#51742,#51743,#51744,#51745,#51746,#51747,#51748,#51749,#51750,#51751,
#51752,#51753,#51754,#51755,#51756,#51757,#51758,#51759,#51760,#51761,#51762,
#51763,#51764,#51765,#51766,#51767,#51768,#51769,#51770,#51771,#51772,#51773,
#51774,#51775,#51776,#51777,#51778,#51779,#51780,#51781,#51782,#51783,#51784,
#51785,#51786,#51787,#51788,#51789,#51790,#51791,#51792,#51793,#51794),
 .UNSPECIFIED.,.F.,.F.,(4,3,3,3,3,3,3,3,3,3,3,3,3,3,3,3,3,3,3,3,3,3,3,4),
(3.70547010534069E-18,0.000685488878875431,0.00136362733180547,0.00203809428842422,
0.00233379670455984,0.00271195014349479,0.00304962754454054,0.00338935778381529,
0.0037325111035576,0.00408059769401021,0.00425701959752223,0.00443534472717101,
0.00461584026680862,0.0047069932936327,0.00479880275422561,0.00489131137324147,
0.0049845646172225,0.00502420741213766,0.00507856216536076,0.0051258809722966,
0.00517358713695751,0.00519763445194167,0.00521516460782795,0.00522531763086377),
 .UNSPECIFIED.);
#1461=B_SPLINE_CURVE_WITH_KNOTS('',3,(#51796,#51797,#51798,#51799,#51800,
#51801,#51802,#51803,#51804,#51805,#51806,#51807,#51808,#51809,#51810,#51811,
#51812,#51813,#51814,#51815,#51816,#51817,#51818,#51819,#51820,#51821,#51822,
#51823,#51824,#51825,#51826,#51827,#51828,#51829,#51830,#51831,#51832,#51833,
#51834,#51835,#51836,#51837,#51838,#51839,#51840,#51841,#51842,#51843,#51844,
#51845,#51846,#51847,#51848,#51849,#51850,#51851,#51852,#51853,#51854,#51855,
#51856,#51857,#51858,#51859,#51860,#51861,#51862,#51863,#51864,#51865,#51866,
#51867,#51868,#51869,#51870,#51871,#51872,#51873,#51874,#51875,#51876,#51877),
 .UNSPECIFIED.,.F.,.F.,(4,3,3,3,3,3,3,3,3,3,3,3,3,3,3,3,3,3,3,3,3,3,3,3,
3,3,3,4),(0.00522531763086377,0.00522824582386111,0.00524825807115921,0.00527773686304108,
0.005310921500641,0.00534817438862756,0.00538918146335247,0.00543238248536955,
0.00547514739040225,0.0055150805388988,0.00557528016196572,0.00564345584262177,
0.00570170125821141,0.00578803619489881,0.00581440066319727,0.00592499322569639,
0.00614208305587578,0.00635423289316619,0.00656198496558043,0.00676580497685607,
0.00696609711170371,0.00735747320605897,0.00773849369111559,0.00811107456944985,
0.00883702717746603,0.00954554528659402,0.010244744341838,0.0115760723897976),
 .UNSPECIFIED.);
#1462=B_SPLINE_CURVE_WITH_KNOTS('',3,(#51878,#51879,#51880,#51881,#51882,
#51883,#51884,#51885,#51886,#51887,#51888,#51889,#51890,#51891,#51892,#51893,
#51894,#51895,#51896,#51897,#51898,#51899,#51900,#51901,#51902,#51903,#51904,
#51905,#51906,#51907,#51908,#51909,#51910,#51911,#51912,#51913,#51914,#51915,
#51916,#51917,#51918,#51919,#51920,#51921,#51922,#51923),.UNSPECIFIED.,
 .F.,.F.,(4,3,3,3,3,3,3,3,3,3,3,3,3,3,3,4),(0.000332625453320718,0.00115607112755972,
0.00186065645282291,0.00239123963891823,0.00362640815027674,0.0045803311999874,
0.00527329949875475,0.00568502233587425,0.00692019084723276,0.00693751245226992,
0.00856708219571078,0.00911007271031551,0.0102139735441888,0.0106256963813083,
0.0112717507118465,0.0135077562411448),.UNSPECIFIED.);
#1463=B_SPLINE_CURVE_WITH_KNOTS('',3,(#51959,#51960,#51961,#51962,#51963,
#51964,#51965,#51966,#51967,#51968,#51969,#51970,#51971,#51972,#51973,#51974,
#51975,#51976,#51977,#51978,#51979,#51980,#51981,#51982,#51983,#51984,#51985,
#51986,#51987,#51988,#51989,#51990,#51991,#51992,#51993,#51994,#51995,#51996,
#51997,#51998,#51999,#52000,#52001),.UNSPECIFIED.,.F.,.F.,(4,3,3,3,3,3,
3,3,3,3,3,3,3,3,4),(0.,0.0803788659656621,0.125,0.199206661927729,0.25,
0.345037361920189,0.375,0.5,0.625,0.654605288102519,0.75,0.800518552305932,
0.875,0.91969786384336,1.),.UNSPECIFIED.);
#1464=B_SPLINE_CURVE_WITH_KNOTS('',3,(#52156,#52157,#52158,#52159,#52160,
#52161,#52162),.UNSPECIFIED.,.F.,.F.,(4,1,1,1,4),(0.,0.00328982736702057,
0.00657965473404115,0.00986948210106172,0.0131593094680823),
 .UNSPECIFIED.);
#1465=B_SPLINE_CURVE_WITH_KNOTS('',3,(#52164,#52165,#52166,#52167,#52168,
#52169,#52170,#52171,#52172,#52173,#52174,#52175,#52176,#52177,#52178,#52179,
#52180,#52181,#52182,#52183,#52184,#52185,#52186,#52187,#52188,#52189,#52190,
#52191,#52192,#52193,#52194,#52195,#52196,#52197,#52198,#52199,#52200,#52201,
#52202,#52203,#52204,#52205,#52206,#52207,#52208,#52209,#52210,#52211,#52212,
#52213,#52214,#52215,#52216,#52217,#52218,#52219,#52220,#52221,#52222,#52223,
#52224,#52225,#52226,#52227,#52228,#52229,#52230,#52231,#52232,#52233,#52234,
#52235,#52236,#52237,#52238,#52239,#52240,#52241,#52242,#52243,#52244,#52245,
#52246,#52247,#52248,#52249,#52250,#52251,#52252,#52253,#52254,#52255,#52256,
#52257,#52258,#52259,#52260,#52261,#52262,#52263),.UNSPECIFIED.,.F.,.F.,
(4,3,3,3,3,3,3,3,3,3,3,3,3,3,3,3,3,3,3,3,3,3,3,3,3,3,3,3,3,3,3,3,3,4),(1.79045146764256E-15,
0.00133239898080196,0.00203135800119964,0.0027393221849017,0.00346457247643882,
0.00383680540508471,0.00421752044955265,0.00460867485617364,0.00480890442754651,
0.00501270574910554,0.00522049417185399,0.00543274922784831,0.00554072296176422,
0.00565003054244384,0.00576075791804394,0.00581233006619133,0.00587405491108055,
0.00593349990772224,0.00599474288809984,0.00605737935932001,0.00612089251884205,
0.00618468694311985,0.00621649466230807,0.00624814061748105,0.00631066365578348,
0.00632608721374795,0.00634141346716181,0.00635663602067303,0.00637174896766624,
0.00640162488731466,0.00643100383429519,0.00648815925212972,0.00654306111029986,
0.00659565065852666),.UNSPECIFIED.);
#1466=B_SPLINE_CURVE_WITH_KNOTS('',3,(#52264,#52265,#52266,#52267,#52268,
#52269,#52270,#52271,#52272,#52273,#52274,#52275,#52276,#52277,#52278,#52279,
#52280,#52281,#52282,#52283,#52284,#52285,#52286,#52287,#52288,#52289,#52290,
#52291,#52292,#52293,#52294,#52295,#52296,#52297,#52298,#52299,#52300,#52301,
#52302,#52303,#52304,#52305,#52306,#52307,#52308,#52309),.UNSPECIFIED.,
 .F.,.F.,(4,3,3,3,3,3,3,3,3,3,3,3,3,3,3,4),(0.00659565065852666,0.00669380080030737,
0.00678763860389039,0.00688067717343409,0.0069731418250513,0.00715645851125297,
0.00733779444607574,0.007517337530045,0.00787172263135117,0.00822084899494823,
0.00856579604438765,0.0089075288715255,0.00958482516796702,0.0102592404404008,
0.0109370028829842,0.0116246601323809),.UNSPECIFIED.);
#1467=B_SPLINE_CURVE_WITH_KNOTS('',3,(#52458,#52459,#52460,#52461,#52462,
#52463,#52464,#52465),.UNSPECIFIED.,.F.,.F.,(4,1,1,1,1,4),(1.77756260508886E-17,
0.00247652675053282,0.00371479012579921,0.00495305350106561,0.00742958025159841,
0.00990610420568183),.UNSPECIFIED.);
#1468=B_SPLINE_CURVE_WITH_KNOTS('',3,(#52467,#52468,#52469,#52470,#52471,
#52472,#52473),.UNSPECIFIED.,.F.,.F.,(4,3,4),(0.890529645287399,0.941951608103805,
1.),.UNSPECIFIED.);
#1469=B_SPLINE_CURVE_WITH_KNOTS('',3,(#52475,#52476,#52477,#52478,#52479,
#52480,#52481,#52482,#52483,#52484,#52485,#52486,#52487,#52488,#52489,#52490,
#52491,#52492,#52493,#52494,#52495,#52496,#52497,#52498,#52499,#52500,#52501,
#52502,#52503,#52504,#52505,#52506,#52507,#52508,#52509,#52510,#52511,#52512,
#52513,#52514,#52515,#52516,#52517,#52518,#52519,#52520,#52521,#52522,#52523,
#52524,#52525,#52526,#52527,#52528,#52529,#52530,#52531,#52532,#52533,#52534,
#52535,#52536,#52537,#52538,#52539,#52540,#52541,#52542,#52543,#52544,#52545,
#52546,#52547,#52548,#52549,#52550,#52551,#52552,#52553,#52554,#52555,#52556,
#52557,#52558,#52559,#52560,#52561,#52562,#52563,#52564,#52565,#52566,#52567,
#52568,#52569,#52570,#52571,#52572,#52573,#52574,#52575,#52576,#52577,#52578,
#52579,#52580,#52581,#52582,#52583,#52584,#52585,#52586,#52587,#52588,#52589,
#52590,#52591,#52592,#52593,#52594,#52595,#52596,#52597,#52598,#52599,#52600,
#52601),.UNSPECIFIED.,.F.,.F.,(4,3,3,3,3,3,3,3,3,3,3,3,3,3,3,3,3,3,3,3,
3,3,3,3,3,3,3,3,3,3,3,3,3,3,3,3,3,3,3,3,3,3,4),(0.4375,0.447953139951671,
0.46875,0.484375,0.5,0.50261698921794,0.515625,0.522734388082496,0.53125,
0.533337365500028,0.543622114252509,0.553625463971614,0.5625,0.568643278230123,
0.574064030279117,0.579758768591498,0.585692930148249,0.588732265688585,
0.590265995396032,0.591807342322294,0.593354897555682,0.594907192948267,
0.598019914889625,0.601133101571348,0.604234327992868,0.610353982579369,
0.616296060704126,0.622000466234711,0.625,0.63268403637845,0.642706690214556,
0.65223168774306,0.670184521519534,0.6875,0.71875,0.746273631098841,0.75,
0.779126048854605,0.78125,0.8125,0.875,0.877403592710768,0.890529645287399),
 .UNSPECIFIED.);
#1470=B_SPLINE_CURVE_WITH_KNOTS('',3,(#52603,#52604,#52605,#52606,#52607,
#52608,#52609,#52610,#52611,#52612,#52613,#52614,#52615,#52616,#52617,#52618,
#52619,#52620,#52621,#52622,#52623,#52624,#52625,#52626,#52627,#52628,#52629,
#52630,#52631,#52632,#52633,#52634,#52635,#52636,#52637,#52638,#52639,#52640,
#52641,#52642,#52643,#52644,#52645,#52646,#52647,#52648),.UNSPECIFIED.,
 .F.,.F.,(4,3,3,3,3,3,3,3,3,3,3,3,3,3,3,4),(0.,0.0680280639044606,0.104883098894702,
0.125,0.144558395882076,0.188305153814917,0.238207334935121,0.25,0.266693333173773,
0.298717535411549,0.3125,0.335981288472857,0.375,0.381870329444042,0.410570188685067,
0.4375),.UNSPECIFIED.);
#1471=B_SPLINE_CURVE_WITH_KNOTS('',3,(#52678,#52679,#52680,#52681,#52682,
#52683,#52684,#52685,#52686,#52687,#52688,#52689,#52690),.UNSPECIFIED.,
 .F.,.F.,(4,3,3,3,4),(0.,0.385769213597709,0.5,0.8882470488323,0.99999999999998),
 .UNSPECIFIED.);
#1472=B_SPLINE_CURVE_WITH_KNOTS('',3,(#52858,#52859,#52860,#52861,#52862,
#52863,#52864,#52865,#52866,#52867,#52868,#52869,#52870,#52871,#52872,#52873,
#52874,#52875,#52876,#52877,#52878,#52879),.UNSPECIFIED.,.F.,.F.,(4,3,3,
3,3,3,3,4),(0.75,0.762630349837623,0.812707493406033,0.856396526178607,
0.875,0.895847435088822,0.932392098898145,1.),.UNSPECIFIED.);
#1473=B_SPLINE_CURVE_WITH_KNOTS('',3,(#52881,#52882,#52883,#52884,#52885,
#52886,#52887,#52888,#52889,#52890,#52891,#52892,#52893,#52894,#52895,#52896,
#52897,#52898,#52899,#52900,#52901,#52902,#52903,#52904,#52905,#52906,#52907,
#52908,#52909,#52910,#52911,#52912,#52913,#52914,#52915,#52916,#52917,#52918,
#52919,#52920,#52921,#52922,#52923,#52924,#52925,#52926,#52927,#52928,#52929,
#52930,#52931,#52932,#52933,#52934,#52935,#52936,#52937,#52938,#52939,#52940,
#52941,#52942,#52943,#52944,#52945,#52946,#52947,#52948,#52949,#52950,#52951,
#52952,#52953,#52954,#52955,#52956,#52957,#52958,#52959,#52960,#52961,#52962,
#52963,#52964,#52965,#52966,#52967,#52968,#52969,#52970,#52971,#52972,#52973,
#52974,#52975,#52976,#52977,#52978,#52979,#52980,#52981,#52982,#52983,#52984,
#52985,#52986,#52987,#52988,#52989,#52990,#52991,#52992,#52993,#52994,#52995,
#52996,#52997,#52998,#52999,#53000,#53001,#53002,#53003,#53004,#53005,#53006,
#53007,#53008,#53009,#53010,#53011,#53012,#53013,#53014,#53015,#53016,#53017,
#53018,#53019,#53020,#53021,#53022,#53023,#53024,#53025,#53026,#53027,#53028,
#53029,#53030,#53031,#53032,#53033,#53034,#53035,#53036,#53037,#53038,#53039,
#53040,#53041,#53042,#53043,#53044,#53045,#53046,#53047,#53048,#53049,#53050,
#53051,#53052,#53053,#53054,#53055,#53056,#53057,#53058,#53059,#53060,#53061,
#53062,#53063,#53064,#53065,#53066,#53067,#53068,#53069,#53070),
 .UNSPECIFIED.,.F.,.F.,(4,3,3,3,3,3,3,3,3,3,3,3,3,3,3,3,3,3,3,3,3,3,3,3,
3,3,3,3,3,3,3,3,3,3,3,3,3,3,3,3,3,3,3,3,3,3,3,3,3,3,3,3,3,3,3,3,3,3,3,3,
3,3,3,4),(0.183933550895872,0.1875,0.21875,0.25,0.25098239560007,0.279533235815916,
0.28125,0.295006732441368,0.31232060369789,0.331303612740551,0.34139109420047,
0.34375,0.351986115795895,0.359375,0.364637802978179,0.375,0.376321507864968,
0.38451085849127,0.388462648085802,0.390625,0.392740169656706,0.397601835508714,
0.400288993494641,0.403160543694781,0.406217079719029,0.40958258006508,
0.411447390674892,0.413444325260174,0.415574852471787,0.417830243347339,
0.418954779483583,0.419628043089068,0.42005515725583,0.421336499756114,
0.42371844902768,0.42676266038335,0.428586931024468,0.430291954434473,0.433433718802995,
0.436311041923835,0.438987607354032,0.443872262911617,0.452821357758043,
0.46160958182739,0.46875,0.478223111052318,0.484375,0.4921875,0.493727913835873,
0.5,0.5078125,0.515625,0.53125,0.542156621633365,0.5625,0.584268222136265,
0.59375,0.615486063512961,0.625,0.66344091850867,0.6875,0.701499573604137,
0.733921780432045,0.75),.UNSPECIFIED.);
#1474=B_SPLINE_CURVE_WITH_KNOTS('',3,(#53072,#53073,#53074,#53075,#53076,
#53077,#53078,#53079,#53080,#53081,#53082,#53083,#53084),.UNSPECIFIED.,
 .F.,.F.,(4,3,3,3,4),(0.,0.0559678243043705,0.11909959188631,0.125,0.183933550895872),
 .UNSPECIFIED.);
#1475=B_SPLINE_CURVE_WITH_KNOTS('',3,(#53085,#53086,#53087,#53088,#53089,
#53090,#53091,#53092,#53093,#53094,#53095,#53096,#53097,#53098,#53099,#53100,
#53101,#53102,#53103,#53104,#53105,#53106,#53107,#53108,#53109,#53110,#53111,
#53112,#53113,#53114,#53115,#53116,#53117,#53118,#53119,#53120,#53121,#53122,
#53123,#53124,#53125,#53126,#53127,#53128,#53129,#53130,#53131,#53132,#53133),
 .UNSPECIFIED.,.F.,.F.,(4,3,3,3,3,3,3,3,3,3,3,3,3,3,3,3,4),(0.000238545193572011,
0.000851590334526773,0.00177115804595892,0.00202346165952711,0.00223094190167499,
0.00269072575739106,0.00319418747363505,0.00391681603930059,0.00425872230842761,
0.00514290632121012,0.00616921820595708,0.00636899660311964,0.00652225788835833,
0.00712664416160244,0.00759508688502917,0.00809898762340667,0.0100472674488482),
 .UNSPECIFIED.);
#1476=B_SPLINE_CURVE_WITH_KNOTS('',3,(#53177,#53178,#53179,#53180,#53181,
#53182,#53183),.UNSPECIFIED.,.F.,.F.,(4,3,4),(1.64794717479639E-14,0.000692615597163757,
0.0022638573967611),.UNSPECIFIED.);
#1477=B_SPLINE_CURVE_WITH_KNOTS('',3,(#53185,#53186,#53187,#53188,#53189,
#53190,#53191,#53192,#53193,#53194),.UNSPECIFIED.,.F.,.F.,(4,1,1,1,1,1,
1,4),(0.,0.000164336190648263,0.000328672381296526,0.000657344762593053,
0.000986017143889579,0.00131468952518611,0.00197203428777916,0.00262937905037221),
 .UNSPECIFIED.);
#1478=B_SPLINE_CURVE_WITH_KNOTS('',3,(#53195,#53196,#53197,#53198,#53199,
#53200,#53201,#53202,#53203,#53204,#53205,#53206,#53207,#53208,#53209,#53210,
#53211,#53212,#53213,#53214,#53215,#53216,#53217,#53218,#53219,#53220,#53221,
#53222),.UNSPECIFIED.,.F.,.F.,(4,3,3,3,3,3,3,3,3,4),(1.58990032769613E-17,
0.000791485231628063,0.000826267123390952,0.00158297046325611,0.00197871307907013,
0.00199274490496515,0.00237445569488416,0.00277019831069818,0.00296806961860519,
0.0031659409265122),.UNSPECIFIED.);
#1479=B_SPLINE_CURVE_WITH_KNOTS('',3,(#53223,#53224,#53225,#53226,#53227,
#53228,#53229),.UNSPECIFIED.,.F.,.F.,(4,3,4),(0.,0.864714126347195,0.999999253323372),
 .UNSPECIFIED.);
#1480=B_SPLINE_CURVE_WITH_KNOTS('',3,(#53280,#53281,#53282,#53283,#53284,
#53285,#53286,#53287,#53288,#53289,#53290,#53291,#53292,#53293,#53294,#53295,
#53296,#53297,#53298),.UNSPECIFIED.,.F.,.F.,(4,3,3,3,3,3,4),(3.84625751079355E-15,
0.000265106688219907,0.000530213376435968,0.000795320064652029,0.00106042675286809,
0.00159064012930021,0.00212085350573233),.UNSPECIFIED.);
#1481=B_SPLINE_CURVE_WITH_KNOTS('',3,(#53300,#53301,#53302,#53303,#53304,
#53305,#53306,#53307,#53308,#53309,#53310,#53311,#53312,#53313,#53314,#53315,
#53316,#53317,#53318,#53319,#53320,#53321,#53322,#53323,#53324,#53325,#53326,
#53327,#53328,#53329,#53330,#53331,#53332,#53333),.UNSPECIFIED.,.F.,.F.,
(4,3,3,3,3,3,3,3,3,3,3,4),(3.93312924486614E-18,0.000498106772859835,0.000538560220293626,
0.000996213545719667,0.00106388037241615,0.00124526693214958,0.0014943203185795,
0.00156579269657072,0.00174337370500941,0.00180010855767657,0.00186790039822437,
0.00199242709143933),.UNSPECIFIED.);
#1482=B_SPLINE_CURVE_WITH_KNOTS('',3,(#53334,#53335,#53336,#53337),
 .UNSPECIFIED.,.F.,.F.,(4,4),(-0.000356991008063635,0.00227547242484036),
 .UNSPECIFIED.);
#1483=B_SPLINE_CURVE_WITH_KNOTS('',3,(#53338,#53339,#53340,#53341),
 .UNSPECIFIED.,.F.,.F.,(4,4),(6.75947242081653E-8,1.),.UNSPECIFIED.);
#1484=B_SPLINE_CURVE_WITH_KNOTS('',3,(#53388,#53389,#53390,#53391),
 .UNSPECIFIED.,.F.,.F.,(4,4),(5.26912590866588E-9,0.00263380354365925),
 .UNSPECIFIED.);
#1485=B_SPLINE_CURVE_WITH_KNOTS('',3,(#53393,#53394,#53395,#53396,#53397,
#53398,#53399,#53400,#53401,#53402,#53403,#53404,#53405,#53406,#53407,#53408,
#53409,#53410,#53411,#53412,#53413,#53414,#53415,#53416,#53417,#53418,#53419,
#53420,#53421,#53422,#53423,#53424,#53425,#53426),.UNSPECIFIED.,.F.,.F.,
(4,3,3,3,3,3,3,3,3,3,3,4),(0.,0.000124653703275801,0.000184227434801142,
0.000249307406551601,0.00041766537279728,0.000498614813103202,0.000747922219654804,
0.000922322810580849,0.000997229626206405,0.00145222768964327,0.00149584443930961,
0.00199445925241281),.UNSPECIFIED.);
#1486=B_SPLINE_CURVE_WITH_KNOTS('',3,(#53427,#53428,#53429,#53430,#53431,
#53432,#53433,#53434,#53435,#53436,#53437,#53438,#53439,#53440,#53441,#53442,
#53443,#53444,#53445),.UNSPECIFIED.,.F.,.F.,(4,3,3,3,3,3,4),(3.90312782094781E-18,
0.000530467727866949,0.00106093545573389,0.00132616931966737,0.00159140318360084,
0.00185663704753431,0.00212187091146779),.UNSPECIFIED.);
#1487=B_SPLINE_CURVE_WITH_KNOTS('',3,(#53446,#53447,#53448,#53449),
 .UNSPECIFIED.,.F.,.F.,(4,4),(0.,1.),.UNSPECIFIED.);
#1488=B_SPLINE_CURVE_WITH_KNOTS('',3,(#53452,#53453,#53454,#53455,#53456,
#53457,#53458),.UNSPECIFIED.,.F.,.F.,(4,3,4),(7.59701845949959E-7,0.86537068925697,
1.),.UNSPECIFIED.);
#1489=B_SPLINE_CURVE_WITH_KNOTS('',3,(#53505,#53506,#53507,#53508,#53509,
#53510,#53511,#53512,#53513,#53514,#53515,#53516,#53517,#53518,#53519,#53520,
#53521,#53522,#53523,#53524,#53525,#53526,#53527,#53528,#53529,#53530,#53531,
#53532),.UNSPECIFIED.,.F.,.F.,(4,3,3,3,3,3,3,3,3,4),(5.70737205233477E-16,
0.000202064457052415,0.000404128914104259,0.000808257828207947,0.00119619719877999,
0.00121238674231163,0.00161651565641532,0.00237726972942536,0.0024247734846227,
0.00323303131283008),.UNSPECIFIED.);
#1490=B_SPLINE_CURVE_WITH_KNOTS('',3,(#53534,#53535,#53536,#53537,#53538,
#53539,#53540,#53541,#53542,#53543,#53544,#53545,#53546,#53547,#53548,#53549,
#53550,#53551,#53552,#53553,#53554,#53555,#53556,#53557,#53558,#53559,#53560,
#53561,#53562,#53563,#53564,#53565,#53566,#53567),.UNSPECIFIED.,.F.,.F.,
(4,3,3,3,3,3,3,3,3,3,3,4),(7.94950163848063E-18,0.000640690988150711,0.000699211931287781,
0.00128138197630141,0.00137633837260762,0.00160172747037677,0.00192207296445212,
0.00201766788276466,0.00224241845852747,0.00231776125826869,0.00240259120556514,
0.00256276376725831),.UNSPECIFIED.);
#1491=B_SPLINE_CURVE_WITH_KNOTS('',3,(#53568,#53569,#53570,#53571,#53572,
#53573,#53574),.UNSPECIFIED.,.F.,.F.,(4,3,4),(-0.000461466528563571,0.00111744893139882,
0.00182907629052203),.UNSPECIFIED.);
#1492=B_SPLINE_CURVE_WITH_KNOTS('',3,(#53584,#53585,#53586,#53587,#53588,
#53589,#53590,#53591,#53592,#53593,#53594,#53595),.UNSPECIFIED.,.F.,.F.,
(4,2,2,2,2,4),(-0.0429082490477899,-0.0358623622035485,-0.0270225822664231,
-0.0151674140885932,0.,0.000281753242151189),.UNSPECIFIED.);
#1493=B_SPLINE_CURVE_WITH_KNOTS('',3,(#53604,#53605,#53606,#53607,#53608,
#53609,#53610,#53611,#53612,#53613,#53614,#53615,#53616,#53617),
 .UNSPECIFIED.,.F.,.F.,(4,2,2,2,2,2,4),(-0.0423657771798303,-0.0371697057665082,
-0.0311389710525321,-0.022717188634609,-0.0120263902095206,-3.97598620693884E-15,
0.00034806785588522),.UNSPECIFIED.);
#1494=B_SPLINE_CURVE_WITH_KNOTS('',3,(#53619,#53620,#53621,#53622,#53623,
#53624,#53625,#53626,#53627,#53628,#53629,#53630,#53631,#53632),
 .UNSPECIFIED.,.F.,.F.,(4,2,2,2,2,2,4),(-0.0423574776745687,-0.0371604407800644,
-0.0311227690155774,-0.022675758099277,-0.0120468921834928,-2.5882074261574E-15,
0.000356146845347506),.UNSPECIFIED.);
#1495=B_SPLINE_CURVE_WITH_KNOTS('',3,(#53641,#53642,#53643,#53644,#53645,
#53646,#53647,#53648,#53649,#53650,#53651,#53652),.UNSPECIFIED.,.F.,.F.,
(4,2,2,2,2,4),(0.0382003500357908,0.043948148696183,0.0511593452998606,
0.060830394704669,0.0732034634623376,0.0734333083269417),.UNSPECIFIED.);
#1496=B_SPLINE_CURVE_WITH_KNOTS('',3,(#53673,#53674,#53675,#53676,#53677,
#53678,#53679),.UNSPECIFIED.,.F.,.F.,(4,3,4),(0.,0.726667315922346,1.),
 .UNSPECIFIED.);
#1497=B_SPLINE_CURVE_WITH_KNOTS('',3,(#53686,#53687,#53688,#53689,#53690,
#53691,#53692),.UNSPECIFIED.,.F.,.F.,(4,3,4),(1.07390946806767E-6,0.86016968037695,
0.999942871118562),.UNSPECIFIED.);
#1498=B_SPLINE_CURVE_WITH_KNOTS('',3,(#53693,#53694,#53695,#53696,#53697,
#53698,#53699,#53700,#53701,#53702,#53703,#53704,#53705,#53706,#53707,#53708,
#53709,#53710,#53711,#53712,#53713,#53714,#53715,#53716,#53717,#53718,#53719,
#53720,#53721,#53722,#53723),.UNSPECIFIED.,.F.,.F.,(4,3,3,3,3,3,3,3,3,3,
4),(1.34228257431211E-16,3.87540787402395E-5,7.75081574803447E-5,0.000155016314960555,
0.000310032629920976,0.000465048944881397,0.000620065259841818,0.00093009788976266,
0.0012401305196835,0.00186019577952519,0.00248026103936687),
 .UNSPECIFIED.);
#1499=B_SPLINE_CURVE_WITH_KNOTS('',3,(#53778,#53779,#53780,#53781,#53782,
#53783,#53784),.UNSPECIFIED.,.F.,.F.,(4,3,4),(0.,0.816373731602943,1.),
 .UNSPECIFIED.);
#1500=B_SPLINE_CURVE_WITH_KNOTS('',3,(#53793,#53794,#53795,#53796,#53797,
#53798,#53799,#53800,#53801,#53802,#53803,#53804,#53805,#53806,#53807,#53808,
#53809,#53810,#53811,#53812,#53813,#53814,#53815,#53816,#53817,#53818,#53819,
#53820,#53821,#53822,#53823),.UNSPECIFIED.,.F.,.F.,(4,3,3,3,3,3,3,3,3,3,
4),(4.26082128994329E-16,0.000617840564227267,0.00123568112845411,0.00154460141056753,
0.00185352169268095,0.00200798183373766,0.00216244197479437,0.00231690211585108,
0.00239413218637943,0.00243274722164361,0.00247136225690779),
 .UNSPECIFIED.);
#1501=B_SPLINE_CURVE_WITH_KNOTS('',3,(#53824,#53825,#53826,#53827,#53828,
#53829,#53830),.UNSPECIFIED.,.F.,.F.,(4,3,4),(3.15157433218311E-5,0.776531405694898,
0.999998921742255),.UNSPECIFIED.);
#1502=B_SPLINE_CURVE_WITH_KNOTS('',3,(#53872,#53873,#53874,#53875,#53876,
#53877,#53878),.UNSPECIFIED.,.F.,.F.,(4,3,4),(0.,0.5,1.),.UNSPECIFIED.);
#1503=B_SPLINE_CURVE_WITH_KNOTS('',3,(#53882,#53883,#53884,#53885,#53886,
#53887,#53888,#53889,#53890,#53891,#53892,#53893,#53894,#53895,#53896,#53897,
#53898,#53899,#53900,#53901,#53902,#53903,#53904,#53905,#53906,#53907,#53908,
#53909,#53910,#53911,#53912,#53913,#53914,#53915,#53916,#53917,#53918,#53919,
#53920,#53921),.UNSPECIFIED.,.F.,.F.,(4,3,3,3,3,3,3,3,3,3,3,3,3,4),(3.87981183129397E-18,
0.000476315485915268,0.00053559406864673,0.000952630971830532,0.0010598222626488,
0.00119078871478816,0.0014289464577458,0.00154802532922461,0.00155886726192386,
0.00166710420070343,0.00177886290992897,0.00184572250792165,0.00188774403954471,
0.00190526194366106),.UNSPECIFIED.);
#1504=B_SPLINE_CURVE_WITH_KNOTS('',3,(#53922,#53923,#53924,#53925,#53926,
#53927,#53928),.UNSPECIFIED.,.F.,.F.,(4,3,4),(9.15977827778901E-6,0.5,0.999998963616504),
 .UNSPECIFIED.);
#1505=B_SPLINE_CURVE_WITH_KNOTS('',3,(#53982,#53983,#53984,#53985,#53986,
#53987,#53988),.UNSPECIFIED.,.F.,.F.,(4,3,4),(0.,0.661687537605397,0.999999849194684),
 .UNSPECIFIED.);
#1506=B_SPLINE_CURVE_WITH_KNOTS('',3,(#53993,#53994,#53995,#53996,#53997,
#53998,#53999),.UNSPECIFIED.,.F.,.F.,(4,3,4),(1.05656453661477E-6,0.769344479228148,
0.999985988157446),.UNSPECIFIED.);
#1507=B_SPLINE_CURVE_WITH_KNOTS('',3,(#54000,#54001,#54002,#54003,#54004,
#54005,#54006,#54007,#54008,#54009,#54010,#54011,#54012,#54013,#54014,#54015,
#54016,#54017,#54018,#54019,#54020,#54021,#54022,#54023,#54024,#54025,#54026,
#54027,#54028,#54029,#54030),.UNSPECIFIED.,.F.,.F.,(4,3,3,3,3,3,3,3,3,3,
4),(7.59605884606955E-17,3.00957540793479E-5,6.01915081586198E-5,0.000120383016317164,
0.000240766032634251,0.000361149048951339,0.000481532065268427,0.000722298097902602,
0.000963064130536778,0.00144459619580513,0.00192612826107348),
 .UNSPECIFIED.);
#1508=B_SPLINE_CURVE_WITH_KNOTS('',3,(#54034,#54035,#54036,#54037,#54038,
#54039,#54040,#54041,#54042,#54043,#54044,#54045,#54046,#54047,#54048,#54049),
 .UNSPECIFIED.,.F.,.F.,(4,2,2,2,2,2,2,4),(-0.0333293903198794,-0.0329576040327539,
-0.0259519923232747,-0.0185023367726281,-0.0101196043509111,-0.00508448543974312,
-4.19109191795997E-15,0.00022476035086433),.UNSPECIFIED.);
#1509=B_SPLINE_CURVE_WITH_KNOTS('',3,(#54050,#54051,#54052,#54053,#54054,
#54055,#54056,#54057,#54058,#54059,#54060,#54061),.UNSPECIFIED.,.F.,.F.,
(4,2,2,2,2,4),(0.0333293903199977,0.0401691226088174,0.0479843704625406,
0.0568871869476023,0.0666660435803344,0.066890541210896),.UNSPECIFIED.);
#1510=B_SPLINE_CURVE_WITH_KNOTS('',3,(#54079,#54080,#54081,#54082,#54083,
#54084,#54085,#54086,#54087,#54088,#54089,#54090,#54091,#54092,#54093,#54094,
#54095,#54096,#54097,#54098,#54099,#54100,#54101,#54102,#54103,#54104,#54105,
#54106,#54107,#54108,#54109),.UNSPECIFIED.,.F.,.F.,(4,3,3,3,3,3,3,3,3,3,
4),(0.,1.25074494335884E-5,5.94103848095448E-5,0.000200119190937414,0.000212626640371002,
0.000224352374214991,0.00031229537804491,0.000356266879959869,0.000378252630917348,
0.000389245506396088,0.000400238381874828),.UNSPECIFIED.);
#1511=B_SPLINE_CURVE_WITH_KNOTS('',3,(#54111,#54112,#54113,#54114,#54115,
#54116,#54117,#54118,#54119,#54120),.UNSPECIFIED.,.F.,.F.,(4,2,2,2,4),(0.0495097784252302,
0.0511592393817984,0.0608272218939915,0.0732022980075359,0.0734320722136546),
 .UNSPECIFIED.);
#1512=(
BOUNDED_CURVE()
B_SPLINE_CURVE(2,(#24900,#24901,#24902),.UNSPECIFIED.,.F.,.F.)
B_SPLINE_CURVE_WITH_KNOTS((3,3),(-0.99956690722118,-2.51118997643904E-6),
 .UNSPECIFIED.)
CURVE()
GEOMETRIC_REPRESENTATION_ITEM()
RATIONAL_B_SPLINE_CURVE((0.999750853586006,0.71236441613048,0.999998554758888))
REPRESENTATION_ITEM('')
);
#1513=(
BOUNDED_CURVE()
B_SPLINE_CURVE(2,(#25047,#25048,#25049),.UNSPECIFIED.,.F.,.F.)
B_SPLINE_CURVE_WITH_KNOTS((3,3),(-0.999613386882244,0.),.UNSPECIFIED.)
CURVE()
GEOMETRIC_REPRESENTATION_ITEM()
RATIONAL_B_SPLINE_CURVE((0.999776843008427,0.711394956192752,1.))
REPRESENTATION_ITEM('')
);
#1514=(
BOUNDED_CURVE()
B_SPLINE_CURVE(2,(#47235,#47236,#47237),.UNSPECIFIED.,.F.,.F.)
B_SPLINE_CURVE_WITH_KNOTS((3,3),(-0.999702996074256,0.),.UNSPECIFIED.)
CURVE()
GEOMETRIC_REPRESENTATION_ITEM()
RATIONAL_B_SPLINE_CURVE((0.999826070801379,0.707193771622355,1.))
REPRESENTATION_ITEM('')
);
#1515=(
BOUNDED_CURVE()
B_SPLINE_CURVE(2,(#47251,#47252,#47253),.UNSPECIFIED.,.F.,.F.)
B_SPLINE_CURVE_WITH_KNOTS((3,3),(-0.994986770849844,0.),.UNSPECIFIED.)
CURVE()
GEOMETRIC_REPRESENTATION_ITEM()
RATIONAL_B_SPLINE_CURVE((0.997078040613149,0.708575122008982,1.))
REPRESENTATION_ITEM('')
);
#1516=(
BOUNDED_CURVE()
B_SPLINE_CURVE(2,(#47319,#47320,#47321),.UNSPECIFIED.,.F.,.F.)
B_SPLINE_CURVE_WITH_KNOTS((3,3),(0.00740039126125963,1.),.UNSPECIFIED.)
CURVE()
GEOMETRIC_REPRESENTATION_ITEM()
RATIONAL_B_SPLINE_CURVE((0.995114090594777,0.669888440169379,1.))
REPRESENTATION_ITEM('')
);
#1517=(
BOUNDED_CURVE()
B_SPLINE_CURVE(2,(#47419,#47420,#47421),.UNSPECIFIED.,.F.,.F.)
B_SPLINE_CURVE_WITH_KNOTS((3,3),(-0.00697045907981074,0.999910955807272),
 .UNSPECIFIED.)
CURVE()
GEOMETRIC_REPRESENTATION_ITEM()
RATIONAL_B_SPLINE_CURVE((1.00469261537463,0.6634228407113,0.999940474400924))
REPRESENTATION_ITEM('')
);
#1518=(
BOUNDED_CURVE()
B_SPLINE_CURVE(2,(#47494,#47495,#47496),.UNSPECIFIED.,.F.,.F.)
B_SPLINE_CURVE_WITH_KNOTS((3,3),(-1.02488087602095,0.),.UNSPECIFIED.)
CURVE()
GEOMETRIC_REPRESENTATION_ITEM()
RATIONAL_B_SPLINE_CURVE((1.01354104029,0.727882565738598,1.))
REPRESENTATION_ITEM('')
);
#1519=(
BOUNDED_CURVE()
B_SPLINE_CURVE(2,(#47625,#47626,#47627),.UNSPECIFIED.,.F.,.F.)
B_SPLINE_CURVE_WITH_KNOTS((3,3),(-1.01384567949804,0.),.UNSPECIFIED.)
CURVE()
GEOMETRIC_REPRESENTATION_ITEM()
RATIONAL_B_SPLINE_CURVE((1.00769298321285,0.722188311019934,1.))
REPRESENTATION_ITEM('')
);
#1520=(
BOUNDED_CURVE()
B_SPLINE_CURVE(2,(#49167,#49168,#49169),.UNSPECIFIED.,.F.,.F.)
B_SPLINE_CURVE_WITH_KNOTS((3,3),(-0.999979498354126,-3.91220184957483E-5),
 .UNSPECIFIED.)
CURVE()
GEOMETRIC_REPRESENTATION_ITEM()
RATIONAL_B_SPLINE_CURVE((0.999987153020195,0.686696441488091,0.999975485362207))
REPRESENTATION_ITEM('')
);
#1521=(
BOUNDED_CURVE()
B_SPLINE_CURVE(2,(#49183,#49184,#49185),.UNSPECIFIED.,.F.,.F.)
B_SPLINE_CURVE_WITH_KNOTS((3,3),(-1.00003164257888,4.00451552356698E-5),
 .UNSPECIFIED.)
CURVE()
GEOMETRIC_REPRESENTATION_ITEM()
RATIONAL_B_SPLINE_CURVE((1.00001982986642,0.686645949278685,1.00002509582908))
REPRESENTATION_ITEM('')
);
#1522=(
BOUNDED_CURVE()
B_SPLINE_CURVE(2,(#49260,#49261,#49262),.UNSPECIFIED.,.F.,.F.)
B_SPLINE_CURVE_WITH_KNOTS((3,3),(-0.999979498354114,-3.91220185005021E-5),
 .UNSPECIFIED.)
CURVE()
GEOMETRIC_REPRESENTATION_ITEM()
RATIONAL_B_SPLINE_CURVE((0.999987153020188,0.686696441488096,0.999975485362204))
REPRESENTATION_ITEM('')
);
#1523=(
BOUNDED_CURVE()
B_SPLINE_CURVE(2,(#49276,#49277,#49278),.UNSPECIFIED.,.F.,.F.)
B_SPLINE_CURVE_WITH_KNOTS((3,3),(-1.00003164257888,4.00451552399089E-5),
 .UNSPECIFIED.)
CURVE()
GEOMETRIC_REPRESENTATION_ITEM()
RATIONAL_B_SPLINE_CURVE((1.00001982986642,0.686645949278685,1.00002509582908))
REPRESENTATION_ITEM('')
);
#1524=(
BOUNDED_CURVE()
B_SPLINE_CURVE(2,(#49353,#49354,#49355),.UNSPECIFIED.,.F.,.F.)
B_SPLINE_CURVE_WITH_KNOTS((3,3),(-0.999979498354106,-3.9122018497479E-5),
 .UNSPECIFIED.)
CURVE()
GEOMETRIC_REPRESENTATION_ITEM()
RATIONAL_B_SPLINE_CURVE((0.999987153020183,0.686696441488098,0.999975485362207))
REPRESENTATION_ITEM('')
);
#1525=(
BOUNDED_CURVE()
B_SPLINE_CURVE(2,(#49369,#49370,#49371),.UNSPECIFIED.,.F.,.F.)
B_SPLINE_CURVE_WITH_KNOTS((3,3),(-1.00003164257888,4.00451552363315E-5),
 .UNSPECIFIED.)
CURVE()
GEOMETRIC_REPRESENTATION_ITEM()
RATIONAL_B_SPLINE_CURVE((1.00001982986642,0.686645949278687,1.00002509582908))
REPRESENTATION_ITEM('')
);
#1526=(
BOUNDED_CURVE()
B_SPLINE_CURVE(2,(#49446,#49447,#49448),.UNSPECIFIED.,.F.,.F.)
B_SPLINE_CURVE_WITH_KNOTS((3,3),(-0.999979498354116,-3.91220185320975E-5),
 .UNSPECIFIED.)
CURVE()
GEOMETRIC_REPRESENTATION_ITEM()
RATIONAL_B_SPLINE_CURVE((0.999987153020189,0.686696441488106,0.999975485362184))
REPRESENTATION_ITEM('')
);
#1527=(
BOUNDED_CURVE()
B_SPLINE_CURVE(2,(#49462,#49463,#49464),.UNSPECIFIED.,.F.,.F.)
B_SPLINE_CURVE_WITH_KNOTS((3,3),(-1.00003164257888,4.0045155211594E-5),
 .UNSPECIFIED.)
CURVE()
GEOMETRIC_REPRESENTATION_ITEM()
RATIONAL_B_SPLINE_CURVE((1.00001982986642,0.686645949278692,1.00002509582907))
REPRESENTATION_ITEM('')
);
#1528=(
BOUNDED_CURVE()
B_SPLINE_CURVE(2,(#49539,#49540,#49541),.UNSPECIFIED.,.F.,.F.)
B_SPLINE_CURVE_WITH_KNOTS((3,3),(-0.999979498354118,-3.91220184959991E-5),
 .UNSPECIFIED.)
CURVE()
GEOMETRIC_REPRESENTATION_ITEM()
RATIONAL_B_SPLINE_CURVE((0.99998715302019,0.686696441488094,0.999975485362207))
REPRESENTATION_ITEM('')
);
#1529=(
BOUNDED_CURVE()
B_SPLINE_CURVE(2,(#49555,#49556,#49557),.UNSPECIFIED.,.F.,.F.)
B_SPLINE_CURVE_WITH_KNOTS((3,3),(-1.00003164257889,4.00451552394756E-5),
 .UNSPECIFIED.)
CURVE()
GEOMETRIC_REPRESENTATION_ITEM()
RATIONAL_B_SPLINE_CURVE((1.00001982986643,0.686645949278681,1.00002509582908))
REPRESENTATION_ITEM('')
);
#1530=(
BOUNDED_SURFACE()
B_SPLINE_SURFACE(3,2,((#24841,#24842,#24843),(#24844,#24845,#24846),(#24847,
#24848,#24849),(#24850,#24851,#24852),(#24853,#24854,#24855),(#24856,#24857,
#24858),(#24859,#24860,#24861),(#24862,#24863,#24864),(#24865,#24866,#24867),
(#24868,#24869,#24870),(#24871,#24872,#24873),(#24874,#24875,#24876),(#24877,
#24878,#24879),(#24880,#24881,#24882),(#24883,#24884,#24885),(#24886,#24887,
#24888),(#24889,#24890,#24891),(#24892,#24893,#24894),(#24895,#24896,#24897)),
 .UNSPECIFIED.,.T.,.F.,.F.)
B_SPLINE_SURFACE_WITH_KNOTS((4,1,1,1,1,1,1,1,1,1,1,1,1,1,1,1,4),(3,3),(-0.056131150341711,
-0.0526229534453541,-0.0491147565489971,-0.0456065596526402,-0.0420983627562833,
-0.0385901658599263,-0.0350819689635694,-0.0315737720672124,-0.0280655751708555,
-0.0245573782744986,-0.0210491813781416,-0.0175409844817847,-0.0140327875854278,
-0.0105245906890708,-0.0070163937927139,-0.003508196896357,0.),(0.,1.),
 .UNSPECIFIED.)
GEOMETRIC_REPRESENTATION_ITEM()
RATIONAL_B_SPLINE_SURFACE(((1.,0.712239066951905,1.),(1.,0.711110760308393,
1.),(1.,0.708331161318748,1.),(1.,0.701023190412799,1.),(1.,0.701644224301599,
1.),(1.,0.70884038203116,1.),(1.,0.712835506198471,1.),(1.,0.715218629500482,
1.),(1.,0.715102433806893,1.),(1.,0.712501311419114,1.),(1.,0.708334487423287,
1.),(1.,0.701010241546403,1.),(1.,0.701662301810715,1.),(1.,0.708859933389416,
1.),(1.,0.712846256318991,1.),(1.,0.715219419684522,1.),(1.,0.715101001179818,
1.),(1.,0.713367373595416,1.),(1.,0.712239066951905,1.)))
REPRESENTATION_ITEM('')
SURFACE()
);
#1531=(
BOUNDED_SURFACE()
B_SPLINE_SURFACE(3,2,((#25782,#25783,#25784),(#25785,#25786,#25787),(#25788,
#25789,#25790),(#25791,#25792,#25793),(#25794,#25795,#25796),(#25797,#25798,
#25799),(#25800,#25801,#25802),(#25803,#25804,#25805),(#25806,#25807,#25808),
(#25809,#25810,#25811),(#25812,#25813,#25814),(#25815,#25816,#25817),(#25818,
#25819,#25820),(#25821,#25822,#25823),(#25824,#25825,#25826),(#25827,#25828,
#25829),(#25830,#25831,#25832),(#25833,#25834,#25835),(#25836,#25837,#25838)),
 .UNSPECIFIED.,.T.,.F.,.F.)
B_SPLINE_SURFACE_WITH_KNOTS((4,1,1,1,1,1,1,1,1,1,1,1,1,1,1,1,4),(3,3),(0.056131150341711,
0.0596393472380679,0.0631475441344249,0.0666557410307818,0.0701639379271387,
0.0736721348234957,0.0771803317198526,0.0806885286162096,0.0841967255125665,
0.0877049224089234,0.0912131193052804,0.0947213162016373,0.0982295130979942,
0.101737709994351,0.105245906890708,0.108754103787065,0.112262300683422),
(0.,1.),.UNSPECIFIED.)
GEOMETRIC_REPRESENTATION_ITEM()
RATIONAL_B_SPLINE_SURFACE(((1.,0.712239066951905,1.),(1.,0.711110760308393,
1.),(1.,0.708331161318748,1.),(1.,0.701023190412799,1.),(1.,0.701644224301599,
1.),(1.,0.70884038203116,1.),(1.,0.712835506198471,1.),(1.,0.715218629500482,
1.),(1.,0.715102433806893,1.),(1.,0.712501311419114,1.),(1.,0.708334487423287,
1.),(1.,0.701010241546403,1.),(1.,0.701662301810715,1.),(1.,0.708859933389416,
1.),(1.,0.712846256318991,1.),(1.,0.715219419684522,1.),(1.,0.715101001179818,
1.),(1.,0.713367373595416,1.),(1.,0.712239066951905,1.)))
REPRESENTATION_ITEM('')
SURFACE()
);
#1532=(
BOUNDED_SURFACE()
B_SPLINE_SURFACE(2,2,((#35087,#35088,#35089),(#35090,#35091,#35092),(#35093,
#35094,#35095)),.UNSPECIFIED.,.F.,.F.,.F.)
B_SPLINE_SURFACE_WITH_KNOTS((3,3),(3,3),(-2.00840310324026,-1.7944713619242),
(-0.411288011040583,0.054890026555908),.UNSPECIFIED.)
GEOMETRIC_REPRESENTATION_ITEM()
RATIONAL_B_SPLINE_SURFACE(((1.,0.972957523892801,1.),(0.994284603862378,
0.967396686218674,0.994284603862378),(1.,0.972957523892801,1.)))
REPRESENTATION_ITEM('')
SURFACE()
);
#1533=(
BOUNDED_SURFACE()
B_SPLINE_SURFACE(3,2,((#36527,#36528,#36529),(#36530,#36531,#36532),(#36533,
#36534,#36535),(#36536,#36537,#36538),(#36539,#36540,#36541),(#36542,#36543,
#36544),(#36545,#36546,#36547),(#36548,#36549,#36550),(#36551,#36552,#36553),
(#36554,#36555,#36556),(#36557,#36558,#36559),(#36560,#36561,#36562),(#36563,
#36564,#36565)),.UNSPECIFIED.,.F.,.F.,.F.)
B_SPLINE_SURFACE_WITH_KNOTS((4,1,1,1,1,1,1,1,1,1,4),(3,3),(-9.12136692509678E-5,
0.00220796830307519,0.0044159366061504,0.005519920757688,0.00662390490922561,
0.00883187321230082,0.011039841515376,0.0121438256669136,0.0132478098184512,
0.0154557781215264,0.0177549600938526),(0.,1.00009121366925),
 .UNSPECIFIED.)
GEOMETRIC_REPRESENTATION_ITEM()
RATIONAL_B_SPLINE_SURFACE(((1.,0.856598302581804,1.00002616039),(1.,0.85648245509437,
1.00002618152375),(1.,0.837039368671017,1.00002972847425),(1.,0.783240704790969,
1.00003954282132),(1.,0.741022900299178,1.00004724450303),(1.,0.710759323434978,
1.00005276540681),(1.,0.713774372303659,1.00005221537947),(1.,0.710758784450604,
1.00005276550514),(1.,0.741025562278053,1.00004724401741),(1.,0.783315033613179,
1.00003952926171),(1.,0.836980639913045,1.00002973918798),(1.,0.85648437213857,
1.00002618117402),(1.,0.856596624849924,1.00002616069606)))
REPRESENTATION_ITEM('')
SURFACE()
);
#1534=(
BOUNDED_SURFACE()
B_SPLINE_SURFACE(3,2,((#36578,#36579,#36580),(#36581,#36582,#36583),(#36584,
#36585,#36586),(#36587,#36588,#36589),(#36590,#36591,#36592),(#36593,#36594,
#36595),(#36596,#36597,#36598)),.UNSPECIFIED.,.F.,.F.,.F.)
B_SPLINE_SURFACE_WITH_KNOTS((4,1,1,1,4),(3,3),(0.0220837783457775,0.0258964944248447,
0.0286667756071232,0.0314370567894017,0.0352497216550509),(-0.00765169206451642,
1.00921035252307),.UNSPECIFIED.)
GEOMETRIC_REPRESENTATION_ITEM()
RATIONAL_B_SPLINE_SURFACE(((1.01141897281319,0.246902245950543,1.01376629482688),
(1.01094701638963,0.278028453921076,1.01319732147188),(1.00923044814925,
0.391238609305028,1.01112788975729),(1.00696653098374,0.54054721705706,
1.00839859425289),(1.00514075800961,0.660959582399751,1.00619750931644),
(1.00458410278544,0.697671798635305,1.00552642619379),(1.0046514192879,
0.693232178045747,1.00560758050029)))
REPRESENTATION_ITEM('')
SURFACE()
);
#1535=(
BOUNDED_SURFACE()
B_SPLINE_SURFACE(3,2,((#36612,#36613,#36614),(#36615,#36616,#36617),(#36618,
#36619,#36620),(#36621,#36622,#36623),(#36624,#36625,#36626),(#36627,#36628,
#36629),(#36630,#36631,#36632)),.UNSPECIFIED.,.F.,.F.,.F.)
B_SPLINE_SURFACE_WITH_KNOTS((4,1,1,1,4),(3,3),(0.0225273553584918,0.0261980037033457,
0.0288843286844024,0.0315706536654592,0.0353315086389343),(0.,1.00171344488683),
 .UNSPECIFIED.)
GEOMETRIC_REPRESENTATION_ITEM()
RATIONAL_B_SPLINE_SURFACE(((1.,0.698070739631419,1.00103467829473),(1.,
0.701445296152567,1.00102311406149),(1.,0.667087022821676,1.00114085607701),
(1.,0.554485456741017,1.00152672923231),(1.,0.412396180757329,1.00201365351913),
(1.,0.303473902619339,1.0023869181602),(1.,0.264839160729741,1.00251931516209)))
REPRESENTATION_ITEM('')
SURFACE()
);
#1536=(
BOUNDED_SURFACE()
B_SPLINE_SURFACE(3,2,((#36657,#36658,#36659),(#36660,#36661,#36662),(#36663,
#36664,#36665),(#36666,#36667,#36668),(#36669,#36670,#36671),(#36672,#36673,
#36674),(#36675,#36676,#36677)),.UNSPECIFIED.,.F.,.F.,.F.)
B_SPLINE_SURFACE_WITH_KNOTS((4,1,1,1,4),(3,3),(0.0225273401345282,0.026197989064192,
0.028884314475386,0.03157063988658,0.0353314954622503),(0.,1.00171342949153),
 .UNSPECIFIED.)
GEOMETRIC_REPRESENTATION_ITEM()
RATIONAL_B_SPLINE_SURFACE(((1.,0.698070764188803,1.00103466891399),(1.,
0.701445290615732,1.00102310488779),(1.,0.667086987296867,1.00114084594816),
(1.,0.554485918057329,1.00152671393378),(1.,0.412395167858293,1.00201363889751),
(1.,0.303472815512153,1.00238690043911),(1.,0.264838377974932,1.00251929520844)))
REPRESENTATION_ITEM('')
SURFACE()
);
#1537=(
BOUNDED_SURFACE()
B_SPLINE_SURFACE(3,2,((#36679,#36680,#36681),(#36682,#36683,#36684),(#36685,
#36686,#36687),(#36688,#36689,#36690),(#36691,#36692,#36693),(#36694,#36695,
#36696),(#36697,#36698,#36699)),.UNSPECIFIED.,.F.,.F.,.F.)
B_SPLINE_SURFACE_WITH_KNOTS((4,1,1,1,4),(3,3),(0.0223953062325209,0.0261531475701134,
0.0288373199541088,0.0315214923381043,0.0352152692137),(-0.00583702121317319,
1.00094993511605),.UNSPECIFIED.)
GEOMETRIC_REPRESENTATION_ITEM()
RATIONAL_B_SPLINE_SURFACE(((1.008611578014,0.261626297741005,1.00139466579746),
(1.00816947060695,0.299533459750967,1.00132306543822),(1.00688616459349,
0.409566651199769,1.00111523093893),(1.0052192786986,0.552488739050661,
1.00084527475412),(1.003898428583,0.665741035947371,1.00063135989707),(1.00349620161079,
0.700228770730926,1.00056621827029),(1.00354053058602,0.696427916868363,
1.00057339745458)))
REPRESENTATION_ITEM('')
SURFACE()
);
#1538=(
BOUNDED_SURFACE()
B_SPLINE_SURFACE(3,2,((#36707,#36708,#36709),(#36710,#36711,#36712),(#36713,
#36714,#36715),(#36716,#36717,#36718),(#36719,#36720,#36721),(#36722,#36723,
#36724),(#36725,#36726,#36727),(#36728,#36729,#36730),(#36731,#36732,#36733),
(#36734,#36735,#36736),(#36737,#36738,#36739),(#36740,#36741,#36742),(#36743,
#36744,#36745)),.UNSPECIFIED.,.F.,.F.,.F.)
B_SPLINE_SURFACE_WITH_KNOTS((4,1,1,1,1,1,1,1,1,1,4),(3,3),(-9.11921919217132E-5,
0.00220796838434516,0.00441593676869044,0.00551992096086308,0.00662390515303572,
0.008831873537381,0.0110398419217263,0.0121438261138989,0.0132478103060716,
0.0154557786904168,0.0177549392666837),(0.,1.00009119219192),
 .UNSPECIFIED.)
GEOMETRIC_REPRESENTATION_ITEM()
RATIONAL_B_SPLINE_SURFACE(((1.,0.856596899436669,1.00002615448614),(1.,
0.85648081496737,1.00002617565813),(1.,0.837038206403486,1.00002972168632),
(1.,0.783241039910642,1.00003953344938),(1.,0.741023293792506,1.00004723330699),
(1.,0.710759112115924,1.00005275302112),(1.,0.71377437769044,1.00005220308377),
(1.,0.710759010469376,1.00005275303966),(1.,0.741025173682679,1.00004723296413),
(1.,0.783314706872162,1.00003952001367),(1.,0.836981393995776,1.00002973204801),
(1.,0.856485647362579,1.00002617477678),(1.,0.85659802774457,1.00002615428035)))
REPRESENTATION_ITEM('')
SURFACE()
);
#1539=(
BOUNDED_SURFACE()
B_SPLINE_SURFACE(3,2,((#36746,#36747,#36748),(#36749,#36750,#36751),(#36752,
#36753,#36754),(#36755,#36756,#36757),(#36758,#36759,#36760),(#36761,#36762,
#36763),(#36764,#36765,#36766),(#36767,#36768,#36769),(#36770,#36771,#36772),
(#36773,#36774,#36775),(#36776,#36777,#36778)),.UNSPECIFIED.,.F.,.F.,.F.)
B_SPLINE_SURFACE_WITH_KNOTS((4,1,1,1,1,1,1,1,4),(3,3),(0.,0.00377228174191368,
0.00754456348382736,0.011316845225741,0.0150891269676547,0.0188614087095684,
0.0226336904514821,0.0264059721933958,0.0301782539353095),(0.,1.),
 .UNSPECIFIED.)
GEOMETRIC_REPRESENTATION_ITEM()
RATIONAL_B_SPLINE_SURFACE(((1.,0.720825457499061,1.),(1.,0.746053483029738,
1.),(1.,0.792459011243824,1.),(1.,0.852569440734204,1.),(1.,0.897509773183224,
1.),(1.,0.916020285468781,1.),(1.,0.897590557115624,1.),(1.,0.852747215867504,
1.),(1.,0.792807767335747,1.),(1.,0.746067376211881,1.),(1.,0.72082545750045,
1.)))
REPRESENTATION_ITEM('')
SURFACE()
);
#1540=(
BOUNDED_SURFACE()
B_SPLINE_SURFACE(3,2,((#36809,#36810,#36811),(#36812,#36813,#36814),(#36815,
#36816,#36817),(#36818,#36819,#36820),(#36821,#36822,#36823),(#36824,#36825,
#36826),(#36827,#36828,#36829),(#36830,#36831,#36832),(#36833,#36834,#36835),
(#36836,#36837,#36838),(#36839,#36840,#36841)),.UNSPECIFIED.,.F.,.F.,.F.)
B_SPLINE_SURFACE_WITH_KNOTS((4,1,1,1,1,1,1,1,4),(3,3),(-1.73472347597681E-18,
0.00377227680972667,0.00754455361945335,0.01131683042918,0.0150891072389067,
0.0188613840486334,0.02263366085836,0.0264059376680867,0.0301782144778134),
(0.,1.),.UNSPECIFIED.)
GEOMETRIC_REPRESENTATION_ITEM()
RATIONAL_B_SPLINE_SURFACE(((1.,0.720825215852201,1.),(1.,0.746052603520604,
1.),(1.,0.792461511277909,1.),(1.,0.852568820521414,1.),(1.,0.897509277356171,
1.),(1.,0.91602054372931,1.),(1.,0.897590043072446,1.),(1.,0.852746545403375,
1.),(1.,0.7928103156905,1.),(1.,0.746066497116235,1.),(1.,0.72082521585216,
1.)))
REPRESENTATION_ITEM('')
SURFACE()
);
#1541=(
BOUNDED_SURFACE()
B_SPLINE_SURFACE(3,2,((#36849,#36850,#36851),(#36852,#36853,#36854),(#36855,
#36856,#36857),(#36858,#36859,#36860),(#36861,#36862,#36863),(#36864,#36865,
#36866),(#36867,#36868,#36869),(#36870,#36871,#36872),(#36873,#36874,#36875),
(#36876,#36877,#36878),(#36879,#36880,#36881),(#36882,#36883,#36884),(#36885,
#36886,#36887)),.UNSPECIFIED.,.F.,.F.,.F.)
B_SPLINE_SURFACE_WITH_KNOTS((4,1,1,1,1,1,1,1,1,1,4),(3,3),(-0.00176595467568201,
0.0022074433446026,0.00441488668920515,0.00551860836150642,0.0066223300338077,
0.00882977337841024,0.0110372167230128,0.0121409383953141,0.0132446600676153,
0.0154521034122179,0.0194255014325015),(0.,1.00864869369591),
 .UNSPECIFIED.)
GEOMETRIC_REPRESENTATION_ITEM()
RATIONAL_B_SPLINE_SURFACE(((1.,0.544825883657364,1.00787332302111),(1.,
0.493235442718456,1.00876570286374),(1.,0.525872619257827,1.00820116497777),
(1.,0.621115631978769,1.00655370969037),(1.,0.669445109196877,1.00571773600048),
(1.,0.70093114970011,1.00517310976046),(1.,0.697705140131851,1.0052289112977),
(1.,0.700929440745956,1.00517313932091),(1.,0.669452202490575,1.00571761330503),
(1.,0.621028362011165,1.00655521923281),(1.,0.526002484867079,1.00819891864201),
(1.,0.493141690839259,1.00876732452632),(1.,0.544954936890859,1.00787109073733)))
REPRESENTATION_ITEM('')
SURFACE()
);
#1542=(
BOUNDED_SURFACE()
B_SPLINE_SURFACE(3,2,((#36891,#36892,#36893),(#36894,#36895,#36896),(#36897,
#36898,#36899),(#36900,#36901,#36902),(#36903,#36904,#36905),(#36906,#36907,
#36908),(#36909,#36910,#36911)),.UNSPECIFIED.,.F.,.F.,.F.)
B_SPLINE_SURFACE_WITH_KNOTS((4,1,1,1,4),(3,3),(0.0261906037883101,0.0302303928825723,
0.033115956521331,0.0360015201600897,0.0400413092543519),(-0.0507184440799791,
1.00026154811442),.UNSPECIFIED.)
GEOMETRIC_REPRESENTATION_ITEM()
RATIONAL_B_SPLINE_SURFACE(((1.03014167181211,0.702771482890882,1.00014797223261),
(1.03110563607959,0.693265783553587,1.00015270454957),(1.02714115683959,
0.732359709496436,1.00013324203111),(1.01704078885099,0.831959937984839,
1.00008365705749),(1.00803324096205,0.920783813399147,1.00003943698305),
(1.00421260453237,0.958459298272233,1.00002068062122),(1.00382474942852,
0.962283956641881,1.00001877655346)))
REPRESENTATION_ITEM('')
SURFACE()
);
#1543=(
BOUNDED_SURFACE()
B_SPLINE_SURFACE(3,2,((#36929,#36930,#36931),(#36932,#36933,#36934),(#36935,
#36936,#36937),(#36938,#36939,#36940),(#36941,#36942,#36943),(#36944,#36945,
#36946),(#36947,#36948,#36949)),.UNSPECIFIED.,.F.,.F.,.F.)
B_SPLINE_SURFACE_WITH_KNOTS((4,1,1,1,4),(3,3),(-0.00115047521367835,0.00287618803419606,
0.00575237606839212,0.00862856410258818,0.0126552273504408),(-0.000568079850883721,
1.04798315002903),.UNSPECIFIED.)
GEOMETRIC_REPRESENTATION_ITEM()
RATIONAL_B_SPLINE_SURFACE(((1.0003214960984,0.703447277837381,1.02844217030743),
(1.00033176605283,0.69397412105832,1.02935073434453),(1.00028951139962,
0.732950433664678,1.02561254265631),(1.00018183730347,0.832270601096544,
1.01608681280814),(1.00008575580974,0.920897581817965,1.00758665923973),
(1.00004504507645,0.958449760014905,1.00398505531614),(1.00004061088175,
0.962539926325762,1.00359277024133)))
REPRESENTATION_ITEM('')
SURFACE()
);
#1544=(
BOUNDED_SURFACE()
B_SPLINE_SURFACE(3,2,((#36960,#36961,#36962),(#36963,#36964,#36965),(#36966,
#36967,#36968),(#36969,#36970,#36971),(#36972,#36973,#36974),(#36975,#36976,
#36977),(#36978,#36979,#36980)),.UNSPECIFIED.,.F.,.F.,.F.)
B_SPLINE_SURFACE_WITH_KNOTS((4,1,1,1,4),(3,3),(-0.00115111019723794,0.00287777549291802,
0.0057555509858653,0.00863332647881258,0.0126622121689389),(-0.000643035815390294,
1.07541381943444),.UNSPECIFIED.)
GEOMETRIC_REPRESENTATION_ITEM()
RATIONAL_B_SPLINE_SURFACE(((1.00004576857842,0.961726564359363,1.00576872230422),
(1.00005117817168,0.957202855590032,1.00645055342909),(1.00009690251692,
0.918966409424796,1.01221370053452),(1.00020563830265,0.828037386912416,
1.02591887937431),(1.0003277752714,0.725901782649337,1.04131315816077),
(1.00037553613851,0.685962319009775,1.0473329907381),(1.00036398122763,
0.695624977392983,1.04587659697569)))
REPRESENTATION_ITEM('')
SURFACE()
);
#1545=(
BOUNDED_SURFACE()
B_SPLINE_SURFACE(3,2,((#36995,#36996,#36997),(#36998,#36999,#37000),(#37001,
#37002,#37003),(#37004,#37005,#37006),(#37007,#37008,#37009),(#37010,#37011,
#37012),(#37013,#37014,#37015)),.UNSPECIFIED.,.F.,.F.,.F.)
B_SPLINE_SURFACE_WITH_KNOTS((4,1,1,1,4),(3,3),(0.0261827954531206,0.0302498424885473,
0.0331548760852807,0.036059909682014,0.0400490479324759),(-0.000287608915424847,
1.05864682838005),.UNSPECIFIED.)
GEOMETRIC_REPRESENTATION_ITEM()
RATIONAL_B_SPLINE_SURFACE(((1.00016268700008,0.700581569757827,1.03510922546522),
(1.00016800320713,0.690797319202815,1.03625650774329),(1.00014630959746,
0.730723475269262,1.03157484397877),(1.00009133985094,0.831892930759882,
1.01971190948892),(1.00004296133221,0.920931514840218,1.00927141749565),
(1.00002264108182,0.95833006218513,1.00488613623644),(1.00002066329306,
0.961970097374021,1.00445931275719)))
REPRESENTATION_ITEM('')
SURFACE()
);
#1546=(
BOUNDED_SURFACE()
B_SPLINE_SURFACE(3,2,((#37022,#37023,#37024),(#37025,#37026,#37027),(#37028,
#37029,#37030),(#37031,#37032,#37033),(#37034,#37035,#37036),(#37037,#37038,
#37039),(#37040,#37041,#37042),(#37043,#37044,#37045),(#37046,#37047,#37048),
(#37049,#37050,#37051),(#37052,#37053,#37054),(#37055,#37056,#37057),(#37058,
#37059,#37060)),.UNSPECIFIED.,.F.,.F.,.F.)
B_SPLINE_SURFACE_WITH_KNOTS((4,1,1,1,1,1,1,1,1,1,4),(3,3),(-0.00176595473644677,
0.0022074434205581,0.00441488684111636,0.00551860855139549,0.00662233026167463,
0.00882977368223289,0.0110372171027912,0.0121409388130703,0.0132446605233494,
0.0154521039439077,0.0194255021009125),(0.,1.01020005259311),
 .UNSPECIFIED.)
GEOMETRIC_REPRESENTATION_ITEM()
RATIONAL_B_SPLINE_SURFACE(((1.,0.544126551146727,1.00929986630821),(1.,
0.492459105087841,1.01035388764251),(1.,0.5251450880049,1.00968709015289),
(1.,0.620532420331288,1.00774117854),(1.,0.668936288031776,1.00675373454749),
(1.,0.700471393560587,1.00611041507764),(1.,0.697240194317183,1.00617633188209),
(1.,0.700469222078685,1.0061104593761),(1.,0.668944216768396,1.00675357280043),
(1.,0.620445949537654,1.00774294255329),(1.,0.525271753063256,1.00968450617238),
(1.,0.492359013196966,1.01035592952762),(1.,0.544254308534535,1.00929726004406)))
REPRESENTATION_ITEM('')
SURFACE()
);
#1547=(
BOUNDED_SURFACE()
B_SPLINE_SURFACE(3,2,((#37072,#37073,#37074),(#37075,#37076,#37077),(#37078,
#37079,#37080),(#37081,#37082,#37083),(#37084,#37085,#37086),(#37087,#37088,
#37089),(#37090,#37091,#37092),(#37093,#37094,#37095),(#37096,#37097,#37098),
(#37099,#37100,#37101),(#37102,#37103,#37104),(#37105,#37106,#37107)),
 .UNSPECIFIED.,.F.,.F.,.F.)
B_SPLINE_SURFACE_WITH_KNOTS((4,1,1,1,1,1,1,1,1,4),(3,3),(-0.0030542815954037,
0.00381785199425464,0.00763570398850928,0.0114535559827639,0.0152714079770186,
0.0171803339741459,0.0190892599712732,0.0229071119655278,0.0267249639597825,
0.0335970975494408),(-0.0368451854302645,1.01725950520625),
 .UNSPECIFIED.)
GEOMETRIC_REPRESENTATION_ITEM()
RATIONAL_B_SPLINE_SURFACE(((1.01871196188825,0.741534782597279,1.00859972889014),
(1.02219172652787,0.693469372382115,1.01019897501307),(1.02778619975629,
0.616193844146687,1.01277010856576),(1.03620063164043,0.499966696013097,
1.01663725159439),(1.0425598341734,0.412128089083168,1.01955984293289),
(1.04521778205111,0.375414297116216,1.02078139475567),(1.0442088809608,
0.389350080077,1.02031771938558),(1.0414873683936,0.426941880527789,1.01906695421255),
(1.03623393472764,0.4995066860085,1.01665255717928),(1.02781586355586,0.615784103016817,
1.01278374159022),(1.02216498736205,0.693838716032383,1.01018668610514),
(1.01874578590278,0.741067577110249,1.00861527388518)))
REPRESENTATION_ITEM('')
SURFACE()
);
#1548=(
BOUNDED_SURFACE()
B_SPLINE_SURFACE(3,2,((#37109,#37110,#37111),(#37112,#37113,#37114),(#37115,
#37116,#37117),(#37118,#37119,#37120),(#37121,#37122,#37123),(#37124,#37125,
#37126),(#37127,#37128,#37129),(#37130,#37131,#37132),(#37133,#37134,#37135),
(#37136,#37137,#37138),(#37139,#37140,#37141),(#37142,#37143,#37144)),
 .UNSPECIFIED.,.F.,.F.,.F.)
B_SPLINE_SURFACE_WITH_KNOTS((4,1,1,1,1,1,1,1,1,4),(3,3),(-0.00305427764783682,
0.00381784705979506,0.00763569411959017,0.0114535411793853,0.0152713882391804,
0.0171803117690779,0.0190892352989755,0.0229070823587706,0.0267249294185657,
0.0335970541261962),(-0.0368459337971598,1.01726409934155),
 .UNSPECIFIED.)
GEOMETRIC_REPRESENTATION_ITEM()
RATIONAL_B_SPLINE_SURFACE(((1.01871302304651,0.741524163778113,1.00860236370568),
(1.02219179877096,0.693473164098863,1.01020155449158),(1.0277870960048,
0.616187461632156,1.01277370874625),(1.03620133847609,0.49996474585093,
1.01664173016993),(1.04256065696545,0.4121259097498,1.01956510446546),(1.04521871380193,
0.375411186435116,1.02078701134822),(1.04420986197529,0.389346071187173,
1.02032324286376),(1.04148811400065,0.426940535853924,1.019072057209),(1.03623465494052,
0.499504558259523,1.01665704572551),(1.02781675696288,0.615777766153,1.01278734386809),
(1.02216506046242,0.693842490136804,1.0101892629097),(1.0187468466081,0.741056971847484,
1.00861791237346)))
REPRESENTATION_ITEM('')
SURFACE()
);
#1549=(
BOUNDED_SURFACE()
B_SPLINE_SURFACE(3,2,((#40991,#40992,#40993),(#40994,#40995,#40996),(#40997,
#40998,#40999),(#41000,#41001,#41002),(#41003,#41004,#41005)),
 .UNSPECIFIED.,.F.,.F.,.F.)
B_SPLINE_SURFACE_WITH_KNOTS((4,1,4),(3,3),(0.00211353105058633,0.00519232055190078,
0.00827110090347046),(-0.00516083805459814,1.00866525867518),
 .UNSPECIFIED.)
GEOMETRIC_REPRESENTATION_ITEM()
RATIONAL_B_SPLINE_SURFACE(((1.00303922812236,0.702984379259216,1.00512077981927),
(1.00303934171677,0.702973277982015,1.0051209712139),(1.00303825215374,
0.703079758057304,1.00511913541476),(1.00303914737112,0.702992270862198,
1.00512064376191),(1.00303903424133,0.703003326733027,1.00512045315011)))
REPRESENTATION_ITEM('')
SURFACE()
);
#1550=(
BOUNDED_SURFACE()
B_SPLINE_SURFACE(3,2,((#41051,#41052,#41053),(#41054,#41055,#41056),(#41057,
#41058,#41059),(#41060,#41061,#41062),(#41063,#41064,#41065)),
 .UNSPECIFIED.,.F.,.F.,.F.)
B_SPLINE_SURFACE_WITH_KNOTS((4,1,4),(3,3),(0.00221234569844904,0.00528825921434574,
0.00836416458159152),(-0.00575439008396576,1.00913990416131),
 .UNSPECIFIED.)
GEOMETRIC_REPRESENTATION_ITEM()
RATIONAL_B_SPLINE_SURFACE(((1.00339056153718,0.702685410650244,1.00540347836286),
(1.00339068855421,0.70267427266794,1.00540368078766),(1.00338968434316,
0.702762330823273,1.00540208039415),(1.00339089447563,0.70265621564664,
1.005404008961),(1.0033907691906,0.702667201751574,1.00540380929647)))
REPRESENTATION_ITEM('')
SURFACE()
);
#1551=(
BOUNDED_SURFACE()
B_SPLINE_SURFACE(3,2,((#41081,#41082,#41083),(#41084,#41085,#41086),(#41087,
#41088,#41089),(#41090,#41091,#41092),(#41093,#41094,#41095)),
 .UNSPECIFIED.,.F.,.F.,.F.)
B_SPLINE_SURFACE_WITH_KNOTS((4,1,4),(3,3),(0.00222416842683505,0.00530805677349043,
0.0083919356037823),(-0.00409731518056885,1.0410723457723),
 .UNSPECIFIED.)
GEOMETRIC_REPRESENTATION_ITEM()
RATIONAL_B_SPLINE_SURFACE(((1.0024101526089,0.693757123833212,1.02504954154737),
(1.00241039130659,0.693726794025117,1.02505202241418),(1.00240948251975,
0.693842267831515,1.02504257708129),(1.00241057855278,0.693703001832813,
1.02505396852805),(1.00241027824273,0.693741160335315,1.02505084730281)))
REPRESENTATION_ITEM('')
SURFACE()
);
#1552=(
BOUNDED_SURFACE()
B_SPLINE_SURFACE(3,2,((#41125,#41126,#41127),(#41128,#41129,#41130),(#41131,
#41132,#41133),(#41134,#41135,#41136),(#41137,#41138,#41139)),
 .UNSPECIFIED.,.F.,.F.,.F.)
B_SPLINE_SURFACE_WITH_KNOTS((4,1,4),(3,3),(0.00210886666210934,0.00518760413944781,
0.00826633150911516),(-0.00505999595092042,1.00745187552521),
 .UNSPECIFIED.)
GEOMETRIC_REPRESENTATION_ITEM()
RATIONAL_B_SPLINE_SURFACE(((1.00297954446705,0.703373335363558,1.00439842930772),
(1.00297965807745,0.70336202495157,1.00439859702038),(1.0029785791549,0.70346943640386,
1.00439700430558),(1.00297947505286,0.703380245849253,1.00439832683789),
(1.00297936120932,0.703391579470171,1.00439815878108)))
REPRESENTATION_ITEM('')
SURFACE()
);
#1553=(
BOUNDED_SURFACE()
B_SPLINE_SURFACE(3,2,((#41185,#41186,#41187),(#41188,#41189,#41190),(#41191,
#41192,#41193),(#41194,#41195,#41196),(#41197,#41198,#41199)),
 .UNSPECIFIED.,.F.,.F.,.F.)
B_SPLINE_SURFACE_WITH_KNOTS((4,1,4),(3,3),(0.00220767749077139,0.00528378315884176,
0.00835988069763376),(-0.00560693921170706,1.00691897286156),
 .UNSPECIFIED.)
GEOMETRIC_REPRESENTATION_ITEM()
RATIONAL_B_SPLINE_SURFACE(((1.00330320591931,0.703386463026645,1.00408148016421),
(1.00330333288896,0.70337506170423,1.0040816370494),(1.00330233511646,0.703464657338961,
1.00408040418994),(1.00330352567297,0.70335775053797,1.00408187525559),
(1.00330340109961,0.703368936684566,1.00408172133128)))
REPRESENTATION_ITEM('')
SURFACE()
);
#1554=(
BOUNDED_SURFACE()
B_SPLINE_SURFACE(3,2,((#41215,#41216,#41217),(#41218,#41219,#41220),(#41221,
#41222,#41223),(#41224,#41225,#41226),(#41227,#41228,#41229)),
 .UNSPECIFIED.,.F.,.F.,.F.)
B_SPLINE_SURFACE_WITH_KNOTS((4,1,4),(3,3),(0.00222837931943227,0.00530337439357363,
0.008387101212674),(-0.00371892845766894,1.04348929973661),
 .UNSPECIFIED.)
GEOMETRIC_REPRESENTATION_ITEM()
RATIONAL_B_SPLINE_SURFACE(((1.00218675766921,0.693162880560133,1.02658527365176),
(1.00218697373197,0.693132563495335,1.02658790041173),(1.00218613883333,
0.693249713144516,1.02657775022036),(1.00218713984747,0.693109254830448,
1.02658991994325),(1.00218686662003,0.693147593015035,1.02658659820979)))
REPRESENTATION_ITEM('')
SURFACE()
);
#1555=(
BOUNDED_SURFACE()
B_SPLINE_SURFACE(3,2,((#41259,#41260,#41261),(#41262,#41263,#41264),(#41265,
#41266,#41267),(#41268,#41269,#41270),(#41271,#41272,#41273)),
 .UNSPECIFIED.,.F.,.F.,.F.)
B_SPLINE_SURFACE_WITH_KNOTS((4,1,4),(3,3),(0.00213710998071491,0.00521859354582936,
0.00830006498572616),(-0.0047763098346721,1.04045393253535),
 .UNSPECIFIED.)
GEOMETRIC_REPRESENTATION_ITEM()
RATIONAL_B_SPLINE_SURFACE(((1.00281160073715,0.69370896974105,1.02465899497813),
(1.00281195203053,0.693670700434191,1.02466207597807),(1.00281066656601,
0.693810736765885,1.02465080187972),(1.00281175009521,0.693692698926688,
1.02466030491506),(1.00281146517294,0.693723737877578,1.02465780601937)))
REPRESENTATION_ITEM('')
SURFACE()
);
#1556=(
BOUNDED_SURFACE()
B_SPLINE_SURFACE(3,2,((#41274,#41275,#41276),(#41277,#41278,#41279),(#41280,
#41281,#41282),(#41283,#41284,#41285),(#41286,#41287,#41288)),
 .UNSPECIFIED.,.F.,.F.,.F.)
B_SPLINE_SURFACE_WITH_KNOTS((4,1,4),(3,3),(0.00218918062982001,0.00518293797295347,
0.00817668510764242),(-8.59234239166145E-5,1.00619494117646),
 .UNSPECIFIED.)
GEOMETRIC_REPRESENTATION_ITEM()
RATIONAL_B_SPLINE_SURFACE(((1.00005034519059,0.705219481653293,1.00365198021966),
(1.00005034650813,0.705211767201325,1.00365207579255),(1.00005032906604,
0.705313893907877,1.00365081056405),(1.00005034362165,0.705228668089402,
1.00365186641064),(1.00005034221189,0.705236922522977,1.00365176414802)))
REPRESENTATION_ITEM('')
SURFACE()
);
#1557=(
BOUNDED_SURFACE()
B_SPLINE_SURFACE(3,2,((#41333,#41334,#41335),(#41336,#41337,#41338),(#41339,
#41340,#41341),(#41342,#41343,#41344),(#41345,#41346,#41347)),
 .UNSPECIFIED.,.F.,.F.,.F.)
B_SPLINE_SURFACE_WITH_KNOTS((4,1,4),(3,3),(0.0022120171615497,0.00527933863147846,
0.00824260155135531),(-0.00590011768353364,1.00557329179908),
 .UNSPECIFIED.)
GEOMETRIC_REPRESENTATION_ITEM()
RATIONAL_B_SPLINE_SURFACE(((1.00347694896963,0.703697377703806,1.00328328282864),
(1.00347708155473,0.703686078915469,1.00328340802874),(1.0034760363704,
0.703775148631286,1.00328242106121),(1.00347723423213,0.703673067877452,
1.00328355220201),(1.00347715795409,0.703679568226981,1.00328348017266)))
REPRESENTATION_ITEM('')
SURFACE()
);
#1558=(
BOUNDED_SURFACE()
B_SPLINE_SURFACE(3,2,((#41363,#41364,#41365),(#41366,#41367,#41368),(#41369,
#41370,#41371),(#41372,#41373,#41374),(#41375,#41376,#41377)),
 .UNSPECIFIED.,.F.,.F.,.F.)
B_SPLINE_SURFACE_WITH_KNOTS((4,1,4),(3,3),(0.00222404092240201,0.00529888594152649,
0.00838256483619836),(0.,1.04068548646261),.UNSPECIFIED.)
GEOMETRIC_REPRESENTATION_ITEM()
RATIONAL_B_SPLINE_SURFACE(((1.,0.695167490611038,1.02480451786822),(1.,
0.69513692670821,1.02480700488273),(1.,0.695255211522984,1.02479737993227),
(1.,0.695114648184839,1.02480881770785),(0.999999999999999,0.695152833845352,
1.0248057105035)))
REPRESENTATION_ITEM('')
SURFACE()
);
#1559=(
BOUNDED_SURFACE()
B_SPLINE_SURFACE(3,2,((#41407,#41408,#41409),(#41410,#41411,#41412),(#41413,
#41414,#41415),(#41416,#41417,#41418),(#41419,#41420,#41421)),
 .UNSPECIFIED.,.F.,.F.,.F.)
B_SPLINE_SURFACE_WITH_KNOTS((4,1,4),(3,3),(0.00213247470912648,0.00521406655521492,
0.00829564634926749),(-0.00540439094631414,1.03776288419203),
 .UNSPECIFIED.)
GEOMETRIC_REPRESENTATION_ITEM()
RATIONAL_B_SPLINE_SURFACE(((1.00318331520391,0.694306668775563,1.0229591285056),
(1.00318371379977,0.694268391668199,1.02296200331162),(1.00318224820494,
0.694409132543476,1.02295143295397),(1.00318349318509,0.69428957726687,
1.02296041216509),(1.00318316652491,0.694320946399417,1.02295805618322)))
REPRESENTATION_ITEM('')
SURFACE()
);
#1560=(
BOUNDED_SURFACE()
B_SPLINE_SURFACE(3,2,((#41422,#41423,#41424),(#41425,#41426,#41427),(#41428,
#41429,#41430),(#41431,#41432,#41433),(#41434,#41435,#41436)),
 .UNSPECIFIED.,.F.,.F.,.F.)
B_SPLINE_SURFACE_WITH_KNOTS((4,1,4),(3,3),(0.00233261591753651,0.00517832061855419,
0.00802401515924038),(-7.72572681589754E-5,1.00514489144249),
 .UNSPECIFIED.)
GEOMETRIC_REPRESENTATION_ITEM()
RATIONAL_B_SPLINE_SURFACE(((1.00004526716879,0.705528796585439,1.00302980947609),
(1.00004526749927,0.705526646764979,1.00302983159556),(1.00004525314264,
0.70562003930361,1.00302887068123),(1.00004526513196,0.705542046570605,
1.0030296731472),(1.00004526460806,0.705545454637005,1.00302963808166)))
REPRESENTATION_ITEM('')
SURFACE()
);
#1561=(
BOUNDED_SURFACE()
B_SPLINE_SURFACE(3,2,((#41481,#41482,#41483),(#41484,#41485,#41486),(#41487,
#41488,#41489),(#41490,#41491,#41492),(#41493,#41494,#41495)),
 .UNSPECIFIED.,.F.,.F.,.F.)
B_SPLINE_SURFACE_WITH_KNOTS((4,1,4),(3,3),(0.00243689541702302,0.00527505369168907,
0.00811320384373953),(0.,1.00460943847749),.UNSPECIFIED.)
GEOMETRIC_REPRESENTATION_ITEM()
RATIONAL_B_SPLINE_SURFACE(((1.,0.705724883744445,1.00271288608767),(1.,
0.705721625583332,1.00271291612426),(1.,0.705799460846715,1.00271219857054),
(1.,0.705706915990024,1.00271305173019),(1.,0.705708813997457,1.00271303423269)))
REPRESENTATION_ITEM('')
SURFACE()
);
#1562=(
BOUNDED_SURFACE()
B_SPLINE_SURFACE(3,2,((#41511,#41512,#41513),(#41514,#41515,#41516),(#41517,
#41518,#41519),(#41520,#41521,#41522),(#41523,#41524,#41525)),
 .UNSPECIFIED.,.F.,.F.,.F.)
B_SPLINE_SURFACE_WITH_KNOTS((4,1,4),(3,3),(0.00221982944241213,0.00529456505217135,
0.008378248795424),(0.,1.0382896554605),.UNSPECIFIED.)
GEOMETRIC_REPRESENTATION_ITEM()
RATIONAL_B_SPLINE_SURFACE(((1.,0.69586844611684,1.02329018482571),(1.,0.695837517046898,
1.02329255335257),(1.,0.695957500887875,1.02328336507271),(1.,0.6958162707029,
1.02329418038295),(1.,0.6958544674275,1.0232912553041)))
REPRESENTATION_ITEM('')
SURFACE()
);
#1563=(
BOUNDED_SURFACE()
B_SPLINE_SURFACE(3,2,((#41555,#41556,#41557),(#41558,#41559,#41560),(#41561,
#41562,#41563),(#41564,#41565,#41566),(#41567,#41568,#41569)),
 .UNSPECIFIED.,.F.,.F.,.F.)
B_SPLINE_SURFACE_WITH_KNOTS((4,1,4),(3,3),(0.00212792315612553,0.00520972108197668,
0.00829150685946455),(-0.00526004879476004,1.03627119860815),
 .UNSPECIFIED.)
GEOMETRIC_REPRESENTATION_ITEM()
RATIONAL_B_SPLINE_SURFACE(((1.00309785139817,0.694793504025019,1.02202052760681),
(1.00309824020449,0.694755198050842,1.02202329136765),(1.00309680397593,
0.694896698151953,1.02201308219149),(1.00309803532104,0.694775383576623,
1.02202183498998),(1.00309771298394,0.694807140870483,1.02201954371382)))
REPRESENTATION_ITEM('')
SURFACE()
);
#1564=(
BOUNDED_SURFACE()
B_SPLINE_SURFACE(3,2,((#41570,#41571,#41572),(#41573,#41574,#41575),(#41576,
#41577,#41578),(#41579,#41580,#41581),(#41582,#41583,#41584)),
 .UNSPECIFIED.,.F.,.F.,.F.)
B_SPLINE_SURFACE_WITH_KNOTS((4,1,4),(3,3),(0.00213818526553338,0.0052157458800678,
0.00829330762307971),(-0.00554775121829963,1.01491778474661),
 .UNSPECIFIED.)
GEOMETRIC_REPRESENTATION_ITEM()
RATIONAL_B_SPLINE_SURFACE(((1.00326831063643,0.701019795764348,1.00887031106351),
(1.00326841298166,0.701010433374775,1.0088705888321),(1.00326732556116,
0.701109908987846,1.00886763753426),(1.003268229636,0.701027205563585,1.00887009122547),
(1.00326811057159,0.701038097399366,1.00886976808042)))
REPRESENTATION_ITEM('')
SURFACE()
);
#1565=(
BOUNDED_SURFACE()
B_SPLINE_SURFACE(3,2,((#41629,#41630,#41631),(#41632,#41633,#41634),(#41635,
#41636,#41637),(#41638,#41639,#41640),(#41641,#41642,#41643)),
 .UNSPECIFIED.,.F.,.F.,.F.)
B_SPLINE_SURFACE_WITH_KNOTS((4,1,4),(3,3),(0.002137775280116,0.00521728249168771,
0.00829679082832463),(-0.015531588982551,1.00678065132455),
 .UNSPECIFIED.)
GEOMETRIC_REPRESENTATION_ITEM()
RATIONAL_B_SPLINE_SURFACE(((1.00924086261519,0.70046593417571,1.00399953462119),
(1.00924114133672,0.700456899673426,1.00399965525456),(1.00923811504382,
0.700554994175509,1.00399834544575),(1.0092406084373,0.700474173118263,
1.00399942461054),(1.00924030377847,0.700484048354195,1.00399929275125)))
REPRESENTATION_ITEM('')
SURFACE()
);
#1566=(
BOUNDED_SURFACE()
B_SPLINE_SURFACE(3,2,((#41659,#41660,#41661),(#41662,#41663,#41664),(#41665,
#41666,#41667),(#41668,#41669,#41670),(#41671,#41672,#41673)),
 .UNSPECIFIED.,.F.,.F.,.F.)
B_SPLINE_SURFACE_WITH_KNOTS((4,1,4),(3,3),(0.00216604370290396,0.00524889691178157,
0.00833175256952228),(-0.044566622087351,1.00513202347875),
 .UNSPECIFIED.)
GEOMETRIC_REPRESENTATION_ITEM()
RATIONAL_B_SPLINE_SURFACE(((1.02727300006651,0.69238259352349,1.00302203016815),
(1.02727633149881,0.692345017658627,1.00302239931305),(1.02726460789245,
0.69247725046666,1.00302110025933),(1.02727436205614,0.692367231380822,
1.00302218108567),(1.02727180366488,0.692396087967221,1.00302189759887)))
REPRESENTATION_ITEM('')
SURFACE()
);
#1567=(
BOUNDED_SURFACE()
B_SPLINE_SURFACE(3,2,((#41703,#41704,#41705),(#41706,#41707,#41708),(#41709,
#41710,#41711),(#41712,#41713,#41714),(#41715,#41716,#41717)),
 .UNSPECIFIED.,.F.,.F.,.F.)
B_SPLINE_SURFACE_WITH_KNOTS((4,1,4),(3,3),(0.00216543696354447,0.00524970208791062,
0.00833396653031472),(-0.00587539799910988,1.04292218799995),
 .UNSPECIFIED.)
GEOMETRIC_REPRESENTATION_ITEM()
RATIONAL_B_SPLINE_SURFACE(((1.00346232181416,0.692633563902817,1.02622525467492),
(1.00346274197103,0.692596264619502,1.02622843714083),(1.00346127232254,
0.692726732162592,1.02621730533155),(1.00346250014727,0.692617732441765,
1.02622660545382),(1.00346217135636,0.692646920741768,1.02622411503681)))
REPRESENTATION_ITEM('')
SURFACE()
);
#1568=(
BOUNDED_SURFACE()
B_SPLINE_SURFACE(3,2,((#41718,#41719,#41720),(#41721,#41722,#41723),(#41724,
#41725,#41726),(#41727,#41728,#41729),(#41730,#41731,#41732)),
 .UNSPECIFIED.,.F.,.F.,.F.)
B_SPLINE_SURFACE_WITH_KNOTS((4,1,4),(3,3),(0.00247947538704121,0.0051691692688655,
0.00785885309266148),(0.,1.00371535323371),.UNSPECIFIED.)
GEOMETRIC_REPRESENTATION_ITEM()
RATIONAL_B_SPLINE_SURFACE(((1.,0.705970164087497,1.00218484940333),(1.,
0.705972859468082,1.00218482937474),(1.,0.70605787745789,1.00218419763102),
(1.,0.705986056430116,1.00218473131199),(1.,0.705985239891227,1.00218473737945)))
REPRESENTATION_ITEM('')
SURFACE()
);
#1569=(
BOUNDED_SURFACE()
B_SPLINE_SURFACE(3,2,((#41778,#41779,#41780),(#41781,#41782,#41783),(#41784,
#41785,#41786),(#41787,#41788,#41789),(#41790,#41791,#41792)),
 .UNSPECIFIED.,.F.,.F.,.F.)
B_SPLINE_SURFACE_WITH_KNOTS((4,1,4),(3,3),(0.00267719565163109,0.00526763354664624,
0.00785807144166138),(0.,1.00296412736609),.UNSPECIFIED.)
GEOMETRIC_REPRESENTATION_ITEM()
RATIONAL_B_SPLINE_SURFACE(((1.,0.706205282353514,1.00174168992518),(1.,
0.706208521892236,1.00174167072037),(1.,0.706274936988307,1.00174127699476),
(1.,0.706196203322784,1.00174174374799),(1.,0.706190892079292,1.00174177523439)))
REPRESENTATION_ITEM('')
SURFACE()
);
#1570=(
BOUNDED_SURFACE()
B_SPLINE_SURFACE(3,2,((#41808,#41809,#41810),(#41811,#41812,#41813),(#41814,
#41815,#41816),(#41817,#41818,#41819),(#41820,#41821,#41822)),
 .UNSPECIFIED.,.F.,.F.,.F.)
B_SPLINE_SURFACE_WITH_KNOTS((4,1,4),(3,3),(0.00221168766977545,0.00528551896642512,
0.00836848652357398),(-0.00323543465076996,1.0329973662126),
 .UNSPECIFIED.)
GEOMETRIC_REPRESENTATION_ITEM()
RATIONAL_B_SPLINE_SURFACE(((1.00190156217512,0.696406930093278,1.01996887164199),
(1.00190175990839,0.696375361075404,1.01997094809804),(1.00190098872769,
0.696498483590981,1.01996284969938),(1.00190188263966,0.696355766470008,
1.01997223693562),(1.00190164269477,0.696394074764875,1.0199697172028)))
REPRESENTATION_ITEM('')
SURFACE()
);
#1571=(
BOUNDED_SURFACE()
B_SPLINE_SURFACE(3,2,((#41854,#41855,#41856),(#41857,#41858,#41859),(#41860,
#41861,#41862),(#41863,#41864,#41865),(#41866,#41867,#41868)),
 .UNSPECIFIED.,.F.,.F.,.F.)
B_SPLINE_SURFACE_WITH_KNOTS((4,1,4),(3,3),(0.00211918404214125,0.00520185796130005,
0.00828451973195975),(-0.00495630116524082,1.03080453538952),
 .UNSPECIFIED.)
GEOMETRIC_REPRESENTATION_ITEM()
RATIONAL_B_SPLINE_SURFACE(((1.00291808547175,0.6965056233853,1.01860304884576),
(1.0029184535517,0.696467341369736,1.01860539538744),(1.00291708203809,
0.696609985124191,1.01859665186883),(1.00291827395877,0.696486019864228,
1.01860425046691),(1.00291796306127,0.696518354641951,1.01860226846824)))
REPRESENTATION_ITEM('')
SURFACE()
);
#1572=(
BOUNDED_SURFACE()
B_SPLINE_SURFACE(3,2,((#41869,#41870,#41871),(#41872,#41873,#41874),(#41875,
#41876,#41877),(#41878,#41879,#41880),(#41881,#41882,#41883),(#41884,#41885,
#41886)),.UNSPECIFIED.,.F.,.F.,.F.)
B_SPLINE_SURFACE_WITH_KNOTS((4,1,1,4),(3,3),(0.00206501500476494,0.00583597574226651,
0.00742288849389084,0.00960693139660508),(-0.0135007365230585,1.00552142297207),
 .UNSPECIFIED.)
GEOMETRIC_REPRESENTATION_ITEM()
RATIONAL_B_SPLINE_SURFACE(((1.00801609181928,0.701462893341436,1.00325254638159),
(1.00801649298684,0.701447952968216,1.00325270915619),(1.00801421110542,
0.701532935312785,1.00325178327793),(1.0080170203036,0.701428314518215,
1.00325292311609),(1.00802044103978,0.701300918686746,1.0032543110871),
(1.00801836836181,0.701378109829282,1.00325347009359)))
REPRESENTATION_ITEM('')
SURFACE()
);
#1573=(
BOUNDED_SURFACE()
B_SPLINE_SURFACE(3,2,((#41920,#41921,#41922),(#41923,#41924,#41925),(#41926,
#41927,#41928),(#41929,#41930,#41931),(#41932,#41933,#41934),(#41935,#41936,
#41937)),.UNSPECIFIED.,.F.,.F.,.F.)
B_SPLINE_SURFACE_WITH_KNOTS((4,1,1,4),(3,3),(0.00206609914260828,0.00583090828463318,
0.00741523232466728,0.00959571243431081),(-0.00622355113870663,1.01477263265198),
 .UNSPECIFIED.)
GEOMETRIC_REPRESENTATION_ITEM()
RATIONAL_B_SPLINE_SURFACE(((1.00366871744853,0.700874212332019,1.00878229800042),
(1.00366887894059,0.700861045213046,1.00878268458549),(1.00366786004834,
0.700944119734037,1.00878024552731),(1.00366914086107,0.700839689747176,
1.00878331157946),(1.00367078368537,0.700705743451035,1.00878724422698),
(1.00366979976439,0.700785966619564,1.00878488888418)))
REPRESENTATION_ITEM('')
SURFACE()
);
#1574=(
BOUNDED_SURFACE()
B_SPLINE_SURFACE(3,2,((#41966,#41967,#41968),(#41969,#41970,#41971),(#41972,
#41973,#41974),(#41975,#41976,#41977),(#41978,#41979,#41980),(#41981,#41982,
#41983)),.UNSPECIFIED.,.F.,.F.,.F.)
B_SPLINE_SURFACE_WITH_KNOTS((4,1,1,4),(3,3),(0.00207738560236064,0.00585322491241914,
0.00744219183711539,0.0096290583604494),(-0.00990380407034745,1.06114958053671),
 .UNSPECIFIED.)
GEOMETRIC_REPRESENTATION_ITEM()
RATIONAL_B_SPLINE_SURFACE(((1.00585937207028,0.685919476704603,1.03801361024168),
(1.00586010065921,0.685880422077222,1.03801833707851),(1.00585811055901,
0.685987097622889,1.03800542598624),(1.00586022036471,0.685874005491064,
1.03801911368701),(1.00586244311324,0.685754859273445,1.03803353412235),
(1.00586161631504,0.685799178222131,1.03802817013727)))
REPRESENTATION_ITEM('')
SURFACE()
);
#1575=(
BOUNDED_SURFACE()
B_SPLINE_SURFACE(3,2,((#42017,#42018,#42019),(#42020,#42021,#42022),(#42023,
#42024,#42025),(#42026,#42027,#42028),(#42029,#42030,#42031),(#42032,#42033,
#42034)),.UNSPECIFIED.,.F.,.F.,.F.)
B_SPLINE_SURFACE_WITH_KNOTS((4,1,1,4),(3,3),(0.00207838220750666,0.00584814811204442,
0.00743455922903145,0.00961791173284076),(-0.0645177248056397,1.00996895944737),
 .UNSPECIFIED.)
GEOMETRIC_REPRESENTATION_ITEM()
RATIONAL_B_SPLINE_SURFACE(((1.0402346106114,0.684892659950512,1.0058982845107),
(1.04023973342761,0.684852539343795,1.00589903550163),(1.04022614361739,
0.684958971315759,1.0058970432724),(1.040240467454,0.684846790633866,1.0058991431079),
(1.04025671917778,0.684719511225116,1.00590152556641),(1.04025057634624,
0.684767620335115,1.00590062504401)))
REPRESENTATION_ITEM('')
SURFACE()
);
#1576=(
BOUNDED_SURFACE()
B_SPLINE_SURFACE(3,2,((#42035,#42036,#42037),(#42038,#42039,#42040),(#42041,
#42042,#42043),(#42044,#42045,#42046),(#42047,#42048,#42049)),
 .UNSPECIFIED.,.F.,.F.,.F.)
B_SPLINE_SURFACE_WITH_KNOTS((4,1,4),(3,3),(0.00242285948437873,0.0051736196439449,
0.00792436969222164),(0.,1.00437695596552),.UNSPECIFIED.)
GEOMETRIC_REPRESENTATION_ITEM()
RATIONAL_B_SPLINE_SURFACE(((1.,0.705776383171405,1.00257560762975),(1.,
0.705777293944189,1.00257559965693),(1.,0.705865449509473,1.00257482795087),
(1.,0.705791558721078,1.00257547478433),(0.999999999999999,0.705792282982492,
1.0025754684442)))
REPRESENTATION_ITEM('')
SURFACE()
);
#1577=(
BOUNDED_SURFACE()
B_SPLINE_SURFACE(3,2,((#42095,#42096,#42097),(#42098,#42099,#42100),(#42101,
#42102,#42103),(#42104,#42105,#42106),(#42107,#42108,#42109)),
 .UNSPECIFIED.,.F.,.F.,.F.)
B_SPLINE_SURFACE_WITH_KNOTS((4,1,4),(3,3),(0.00243078313184364,0.00527111731602525,
0.00811144338637717),(0.,1.00382472942682),.UNSPECIFIED.)
GEOMETRIC_REPRESENTATION_ITEM()
RATIONAL_B_SPLINE_SURFACE(((1.,0.705953974699161,1.00224929297161),(1.,
0.705950577782826,1.00224931895619),(1.,0.706029820377507,1.00224871279322),
(1.,0.705936375867464,1.00224942759315),(1.,0.705938430322632,1.00224941187768)))
REPRESENTATION_ITEM('')
SURFACE()
);
#1578=(
BOUNDED_SURFACE()
B_SPLINE_SURFACE(3,2,((#42125,#42126,#42127),(#42128,#42129,#42130),(#42131,
#42132,#42133),(#42134,#42135,#42136),(#42137,#42138,#42139)),
 .UNSPECIFIED.,.F.,.F.,.F.)
B_SPLINE_SURFACE_WITH_KNOTS((4,1,4),(3,3),(0.00221566111994076,0.00529019030192516,
0.00837375924116679),(-0.00339130215178826,1.03561277968481),
 .UNSPECIFIED.)
GEOMETRIC_REPRESENTATION_ITEM()
RATIONAL_B_SPLINE_SURFACE(((1.00199347489228,0.695587723001425,1.02160614203281),
(1.00199368000553,0.695556401317895,1.02160836513876),(1.00199288246575,
0.695678189106253,1.02159972105817),(1.00199381434552,0.695535887017177,
1.02160982117364),(1.00199356332364,0.695574219148555,1.02160710049009)))
REPRESENTATION_ITEM('')
SURFACE()
);
#1579=(
BOUNDED_SURFACE()
B_SPLINE_SURFACE(3,2,((#42169,#42170,#42171),(#42172,#42173,#42174),(#42175,
#42176,#42177),(#42178,#42179,#42180),(#42181,#42182,#42183)),
 .UNSPECIFIED.,.F.,.F.,.F.)
B_SPLINE_SURFACE_WITH_KNOTS((4,1,4),(3,3),(0.00212349273369012,0.00520565186730131,
0.00828779885095397),(-0.00480844917136824,1.03341610948654),
 .UNSPECIFIED.)
GEOMETRIC_REPRESENTATION_ITEM()
RATIONAL_B_SPLINE_SURFACE(((1.00283061667055,0.69577951134894,1.02023130347533),
(1.00283097276619,0.695741239975037,1.02023384860233),(1.00282965163483,
0.695883228549338,1.02022440606297),(1.00283079197036,0.6957606710036,1.02023255639799),
(1.00283049396244,0.695792699401415,1.02023042644205)))
REPRESENTATION_ITEM('')
SURFACE()
);
#1580=(
BOUNDED_SURFACE()
B_SPLINE_SURFACE(3,2,((#42184,#42185,#42186),(#42187,#42188,#42189),(#42190,
#42191,#42192),(#42193,#42194,#42195),(#42196,#42197,#42198)),
 .UNSPECIFIED.,.F.,.F.,.F.)
B_SPLINE_SURFACE_WITH_KNOTS((4,1,4),(3,3),(0.00211837924580892,0.00519732079082784,
0.00827625862043334),(-0.00532010498308729,1.01360000328723),
 .UNSPECIFIED.)
GEOMETRIC_REPRESENTATION_ITEM()
RATIONAL_B_SPLINE_SURFACE(((1.00313352122389,0.701475567287313,1.00807632313618),
(1.00313363791523,0.70146445033165,1.00807662389591),(1.00313251661584,
0.701571274329799,1.00807373386403),(1.00313341826975,0.701485375526323,
1.00807605778267),(1.00313330429228,0.701496233936907,1.00807576401766)))
REPRESENTATION_ITEM('')
SURFACE()
);
#1581=(
BOUNDED_SURFACE()
B_SPLINE_SURFACE(3,2,((#42243,#42244,#42245),(#42246,#42247,#42248),(#42249,
#42250,#42251),(#42252,#42253,#42254),(#42255,#42256,#42257)),
 .UNSPECIFIED.,.F.,.F.,.F.)
B_SPLINE_SURFACE_WITH_KNOTS((4,1,4),(3,3),(0.00211872601142628,0.00519507594284825,
0.00827142282117545),(-0.0125752621045938,1.00753736038806),
 .UNSPECIFIED.)
GEOMETRIC_REPRESENTATION_ITEM()
RATIONAL_B_SPLINE_SURFACE(((1.00746022322175,0.701113508392646,1.00444926121364),
(1.00746049609062,0.701102576170414,1.00444942395205),(1.00745784401348,
0.701208829027323,1.00444784225891),(1.00745999974221,0.701122461880137,
1.00444912793092),(1.00745972953064,0.701133287640395,1.00444896677732)))
REPRESENTATION_ITEM('')
SURFACE()
);
#1582=(
BOUNDED_SURFACE()
B_SPLINE_SURFACE(3,2,((#42273,#42274,#42275),(#42276,#42277,#42278),(#42279,
#42280,#42281),(#42282,#42283,#42284),(#42285,#42286,#42287)),
 .UNSPECIFIED.,.F.,.F.,.F.)
B_SPLINE_SURFACE_WITH_KNOTS((4,1,4),(3,3),(0.00214652638394637,0.00523052097319175,
0.00831451160094196),(-0.0445550628231248,1.00430563736809),
 .UNSPECIFIED.)
GEOMETRIC_REPRESENTATION_ITEM()
RATIONAL_B_SPLINE_SURFACE(((1.02726594007204,0.692646097681134,1.00253335135591),
(1.02726933899953,0.69260778344634,1.00253366715935),(1.02725699574049,
0.692746922196893,1.00253252031417),(1.02726708176979,0.692633227952121,
1.0025334574341),(1.02726443043493,0.692663114987534,1.0025332110915)))
REPRESENTATION_ITEM('')
SURFACE()
);
#1583=(
BOUNDED_SURFACE()
B_SPLINE_SURFACE(3,2,((#42317,#42318,#42319),(#42320,#42321,#42322),(#42323,
#42324,#42325),(#42326,#42327,#42328),(#42329,#42330,#42331)),
 .UNSPECIFIED.,.F.,.F.,.F.)
B_SPLINE_SURFACE_WITH_KNOTS((4,1,4),(3,3),(0.00214672101519236,0.00522830221175709,
0.00830987665062646),(-0.00501736956493107,1.04391786530058),
 .UNSPECIFIED.)
GEOMETRIC_REPRESENTATION_ITEM()
RATIONAL_B_SPLINE_SURFACE(((1.00295420698496,0.692608136042445,1.02685955507165),
(1.00295457482959,0.692569860983192,1.02686289950325),(1.00295324247231,
0.692708495747623,1.02685078575358),(1.00295434419837,0.692593858679657,
1.02686080261154),(1.0029540534599,0.692624110668846,1.02685815922678)))
REPRESENTATION_ITEM('')
SURFACE()
);
#1584=(
BOUNDED_SURFACE()
B_SPLINE_SURFACE(3,2,((#42332,#42333,#42334),(#42335,#42336,#42337),(#42338,
#42339,#42340),(#42341,#42342,#42343),(#42344,#42345,#42346)),
 .UNSPECIFIED.,.F.,.F.,.F.)
B_SPLINE_SURFACE_WITH_KNOTS((4,1,4),(3,3),(0.00212309359701631,0.00520196736840092,
0.00828083965993362),(-0.00538667073334126,1.01435395411296),
 .UNSPECIFIED.)
GEOMETRIC_REPRESENTATION_ITEM()
RATIONAL_B_SPLINE_SURFACE(((1.00317292968628,0.701233103961014,1.00853037209161),
(1.00317304291575,0.701222442137482,1.00853067650727),(1.00317192956387,
0.70132727669669,1.00852768327806),(1.00317283024653,0.701242467328061,
1.00853010474939),(1.00317271575512,0.701253247978216,1.008529796941)))
REPRESENTATION_ITEM('')
SURFACE()
);
#1585=(
BOUNDED_SURFACE()
B_SPLINE_SURFACE(3,2,((#42391,#42392,#42393),(#42394,#42395,#42396),(#42397,
#42398,#42399),(#42400,#42401,#42402),(#42403,#42404,#42405)),
 .UNSPECIFIED.,.F.,.F.,.F.)
B_SPLINE_SURFACE_WITH_KNOTS((4,1,4),(3,3),(0.00212328649712472,0.00520006178542504,
0.0082768361456668),(-0.0121981081337134,1.00757620462087),
 .UNSPECIFIED.)
GEOMETRIC_REPRESENTATION_ITEM()
RATIONAL_B_SPLINE_SURFACE(((1.00723375242928,0.701215254384846,1.00447234439468),
(1.00723400107668,0.701204984189714,1.00447249812358),(1.00723150164427,
0.701308221379959,1.0044709528229),(1.00723356035961,0.701223187679178,
1.00447222564556),(1.00723330348688,0.701233797615521,1.00447206683127)))
REPRESENTATION_ITEM('')
SURFACE()
);
#1586=(
BOUNDED_SURFACE()
B_SPLINE_SURFACE(3,2,((#42421,#42422,#42423),(#42424,#42425,#42426),(#42427,
#42428,#42429),(#42430,#42431,#42432),(#42433,#42434,#42435)),
 .UNSPECIFIED.,.F.,.F.,.F.)
B_SPLINE_SURFACE_WITH_KNOTS((4,1,4),(3,3),(0.00215121360431741,0.00523488372589789,
0.00831855159752948),(-0.0446503843220741,1.00450356492348),
 .UNSPECIFIED.)
GEOMETRIC_REPRESENTATION_ITEM()
RATIONAL_B_SPLINE_SURFACE(((1.02732668542833,0.692555691390288,1.00265032234403),
(1.02733007044875,0.692517607544939,1.00265065064566),(1.02731787184475,
0.692654850364981,1.00264946754452),(1.0273278731463,0.692542328733031,
1.00265043753676),(1.0273252504547,0.692571835846397,1.00265018317082)))
REPRESENTATION_ITEM('')
SURFACE()
);
#1587=(
BOUNDED_SURFACE()
B_SPLINE_SURFACE(3,2,((#42465,#42466,#42467),(#42468,#42469,#42470),(#42471,
#42472,#42473),(#42474,#42475,#42476),(#42477,#42478,#42479)),
 .UNSPECIFIED.,.F.,.F.,.F.)
B_SPLINE_SURFACE_WITH_KNOTS((4,1,4),(3,3),(0.0021508461774662,0.0052332832138809,
0.00831571518714347),(-0.00531073766834972,1.04411327492098),
 .UNSPECIFIED.)
GEOMETRIC_REPRESENTATION_ITEM()
RATIONAL_B_SPLINE_SURFACE(((1.00312783777046,0.692458369995794,1.02698397756318),
(1.00312822235194,0.692420556392284,1.02698729536256),(1.00312684516247,
0.692555967217898,1.02697541429566),(1.00312799463627,0.692442946316364,
1.02698533085061),(1.0031276897709,0.692472921909204,1.02698270076529)))
REPRESENTATION_ITEM('')
SURFACE()
);
#1588=(
BOUNDED_SURFACE()
B_SPLINE_SURFACE(3,2,((#42480,#42481,#42482),(#42483,#42484,#42485),(#42486,
#42487,#42488),(#42489,#42490,#42491),(#42492,#42493,#42494)),
 .UNSPECIFIED.,.F.,.F.,.F.)
B_SPLINE_SURFACE_WITH_KNOTS((4,1,4),(3,3),(0.0021280017507586,0.00520643335911326,
0.00828486609849074),(-0.00545222989642442,1.01483574006136),
 .UNSPECIFIED.)
GEOMETRIC_REPRESENTATION_ITEM()
RATIONAL_B_SPLINE_SURFACE(((1.00321174730507,0.701071451701929,1.00882085607408),
(1.00321185722931,0.701061220668788,1.00882115797388),(1.00321075044288,
0.701164233150451,1.0088181182566),(1.00321165357415,0.701080175566389,
1.00882059864817),(1.00321153695881,0.701091029363851,1.00882027837168)))
REPRESENTATION_ITEM('')
SURFACE()
);
#1589=(
BOUNDED_SURFACE()
B_SPLINE_SURFACE(3,2,((#42539,#42540,#42541),(#42542,#42543,#42544),(#42545,
#42546,#42547),(#42548,#42549,#42550),(#42551,#42552,#42553)),
 .UNSPECIFIED.,.F.,.F.,.F.)
B_SPLINE_SURFACE_WITH_KNOTS((4,1,4),(3,3),(0.00212778800052849,0.0052053406359233,
0.00828289438645528),(-0.0123411007820522,1.00604991564916),
 .UNSPECIFIED.)
GEOMETRIC_REPRESENTATION_ITEM()
RATIONAL_B_SPLINE_SURFACE(((1.00731954899057,0.701632309420459,1.00356592662071),
(1.00731978090901,0.701622855700233,1.00356603960637),(1.00731734036416,
0.701722339935083,1.00356485062549),(1.00731937739681,0.701639304118356,
1.00356584302392),(1.00731912529299,0.701649580657985,1.00356572020437)))
REPRESENTATION_ITEM('')
SURFACE()
);
#1590=(
BOUNDED_SURFACE()
B_SPLINE_SURFACE(3,2,((#42569,#42570,#42571),(#42572,#42573,#42574),(#42575,
#42576,#42577),(#42578,#42579,#42580),(#42581,#42582,#42583)),
 .UNSPECIFIED.,.F.,.F.,.F.)
B_SPLINE_SURFACE_WITH_KNOTS((4,1,4),(3,3),(0.0021560260114394,0.00523931072137745,
0.00832259563410914),(-0.0447835452829565,1.00470829840081),
 .UNSPECIFIED.)
GEOMETRIC_REPRESENTATION_ITEM()
RATIONAL_B_SPLINE_SURFACE(((1.02741159374151,0.692451908000683,1.00277136329061),
(1.02741496864924,0.692414042765858,1.00277170450009),(1.02740290435876,
0.692549399708443,1.0027704847778),(1.02741282944973,0.692438043804821,
1.00277148822302),(1.02741023266766,0.692467178753231,1.00277122568351)))
REPRESENTATION_ITEM('')
SURFACE()
);
#1591=(
BOUNDED_SURFACE()
B_SPLINE_SURFACE(3,2,((#42613,#42614,#42615),(#42616,#42617,#42618),(#42619,
#42620,#42621),(#42622,#42623,#42624),(#42625,#42626,#42627)),
 .UNSPECIFIED.,.F.,.F.,.F.)
B_SPLINE_SURFACE_WITH_KNOTS((4,1,4),(3,3),(0.00215602788258475,0.00523917993081111,
0.00832232919221315),(-0.00552106013962827,1.04545478644752),
 .UNSPECIFIED.)
GEOMETRIC_REPRESENTATION_ITEM()
RATIONAL_B_SPLINE_SURFACE(((1.00325239185633,0.691993903191183,1.02784031168291),
(1.00325279353845,0.691955863327452,1.0278437500618),(1.00325135869187,
0.692091745322464,1.02783146784683),(1.00325255025752,0.691978902374865,
1.02784166758919),(1.00325223397536,0.692008854742086,1.02783896022967)))
REPRESENTATION_ITEM('')
SURFACE()
);
#1592=(
BOUNDED_SURFACE()
B_SPLINE_SURFACE(3,2,((#42628,#42629,#42630),(#42631,#42632,#42633),(#42634,
#42635,#42636),(#42637,#42638,#42639),(#42640,#42641,#42642)),
 .UNSPECIFIED.,.F.,.F.,.F.)
B_SPLINE_SURFACE_WITH_KNOTS((4,1,4),(3,3),(0.00213299782738826,0.00521097577115018,
0.00828895484434125),(-0.00550087397147942,1.01477086238353),
 .UNSPECIFIED.)
GEOMETRIC_REPRESENTATION_ITEM()
RATIONAL_B_SPLINE_SURFACE(((1.003240550509,0.701076763936148,1.0087816978033),
(1.00324065665487,0.701066972554508,1.00878198545225),(1.00323955961029,
0.701168168976641,1.00877901252713),(1.00324046420802,0.701084724734234,
1.00878146393281),(1.00324034568342,0.701095657987022,1.00878114273824)))
REPRESENTATION_ITEM('')
SURFACE()
);
#1593=(
BOUNDED_SURFACE()
B_SPLINE_SURFACE(3,2,((#42687,#42688,#42689),(#42690,#42691,#42692),(#42693,
#42694,#42695),(#42696,#42697,#42698),(#42699,#42700,#42701)),
 .UNSPECIFIED.,.F.,.F.,.F.)
B_SPLINE_SURFACE_WITH_KNOTS((4,1,4),(3,3),(0.00213310765920635,0.00521163324568507,
0.00829015996762764),(-0.0156377890551712,1.00702192656802),
 .UNSPECIFIED.)
GEOMETRIC_REPRESENTATION_ITEM()
RATIONAL_B_SPLINE_SURFACE(((1.00930506145392,0.700360232778602,1.00414285996969),
(1.00930536821373,0.700350354559057,1.00414299654729),(1.00930220263952,
0.700452291760049,1.00414158714976),(1.00930480530383,0.700368481273429,
1.00414274592489),(1.00930448227842,0.700378883274418,1.00414260210542)))
REPRESENTATION_ITEM('')
SURFACE()
);
#1594=(
BOUNDED_SURFACE()
B_SPLINE_SURFACE(3,2,((#42717,#42718,#42719),(#42720,#42721,#42722),(#42723,
#42724,#42725),(#42726,#42727,#42728),(#42729,#42730,#42731)),
 .UNSPECIFIED.,.F.,.F.,.F.)
B_SPLINE_SURFACE_WITH_KNOTS((4,1,4),(3,3),(0.00216106225273672,0.00524376924181206,
0.00832647862208329),(-0.0446517915472245,1.00491634737552),
 .UNSPECIFIED.)
GEOMETRIC_REPRESENTATION_ITEM()
RATIONAL_B_SPLINE_SURFACE(((1.02732742650838,0.692425328535973,1.00289441476859),
(1.02733077687705,0.692387619586655,1.00289476962662),(1.02731889160327,
0.6925213902941,1.00289351078463),(1.02732871811155,0.69241079133026,1.00289455157018),
(1.02732615236371,0.692439669243409,1.00289427981614)))
REPRESENTATION_ITEM('')
SURFACE()
);
#1595=(
BOUNDED_SURFACE()
B_SPLINE_SURFACE(3,2,((#42756,#42757,#42758),(#42759,#42760,#42761),(#42762,
#42763,#42764),(#42765,#42766,#42767),(#42768,#42769,#42770)),
 .UNSPECIFIED.,.F.,.F.,.F.)
B_SPLINE_SURFACE_WITH_KNOTS((4,1,4),(3,3),(0.00216083159531938,0.00524514060142026,
0.00832944899172471),(-0.00570770278406545,1.04561266300805),
 .UNSPECIFIED.)
GEOMETRIC_REPRESENTATION_ITEM()
RATIONAL_B_SPLINE_SURFACE(((1.00336295925547,0.691888008928606,1.02794117990572),
(1.00336337356489,0.691850050187208,1.0279446221996),(1.00336190347963,
0.69198473837774,1.02793240798181),(1.00336312152517,0.69187314189091,1.02794252812516),
(1.00336279729876,0.691902847289583,1.02793983428684)))
REPRESENTATION_ITEM('')
SURFACE()
);
#1596=(
BOUNDED_SURFACE()
B_SPLINE_SURFACE(3,2,((#42771,#42772,#42773),(#42774,#42775,#42776),(#42777,
#42778,#42779),(#42780,#42781,#42782),(#42783,#42784,#42785),(#42786,#42787,
#42788)),.UNSPECIFIED.,.F.,.F.,.F.)
B_SPLINE_SURFACE_WITH_KNOTS((4,1,1,4),(3,3),(0.00206897381009835,0.00584008937427813,
0.00742706726542499,0.00961119981566884),(-0.0133262372495361,1.00554811092291),
 .UNSPECIFIED.)
GEOMETRIC_REPRESENTATION_ITEM()
RATIONAL_B_SPLINE_SURFACE(((1.00791112140402,0.701506499763767,1.00326835491122),
(1.00791150703105,0.701491949720231,1.00326851422694),(1.00790926322385,
0.701576610520087,1.00326758723341),(1.00791204091466,0.701471805826733,
1.00326873479252),(1.0079153810578,0.701345779317039,1.00327011471993),
(1.00791335564888,0.70142219975936,1.00326927795421)))
REPRESENTATION_ITEM('')
SURFACE()
);
#1597=(
BOUNDED_SURFACE()
B_SPLINE_SURFACE(3,2,((#42821,#42822,#42823),(#42824,#42825,#42826),(#42827,
#42828,#42829),(#42830,#42831,#42832),(#42833,#42834,#42835),(#42836,#42837,
#42838)),.UNSPECIFIED.,.F.,.F.,.F.)
B_SPLINE_SURFACE_WITH_KNOTS((4,1,1,4),(3,3),(0.00206996661703809,0.0058353060121813,
0.00741985318197331,0.00960064037745484),(-0.00834800729421259,1.01461865695033),
 .UNSPECIFIED.)
GEOMETRIC_REPRESENTATION_ITEM()
RATIONAL_B_SPLINE_SURFACE(((1.00493145052503,0.700279457869589,1.00868943892189),
(1.0049316670474,0.700266298211422,1.00868982044411),(1.00493030045999,
0.700349355786042,1.00868741245526),(1.004932019035,0.700244905334656,1.00869044066218),
(1.00493419864013,0.700112434689801,1.00869428122502),(1.00493289102759,
0.700191907927257,1.00869197715257)))
REPRESENTATION_ITEM('')
SURFACE()
);
#1598=(
BOUNDED_SURFACE()
B_SPLINE_SURFACE(3,2,((#42857,#42858,#42859),(#42860,#42861,#42862),(#42863,
#42864,#42865),(#42866,#42867,#42868),(#42869,#42870,#42871),(#42872,#42873,
#42874)),.UNSPECIFIED.,.F.,.F.,.F.)
B_SPLINE_SURFACE_WITH_KNOTS((4,1,1,4),(3,3),(0.00208137534035049,0.00585739874086686,
0.00744644313070167,0.00963341629415647),(-0.0100342287213997,1.06112763756809),
 .UNSPECIFIED.)
GEOMETRIC_REPRESENTATION_ITEM()
RATIONAL_B_SPLINE_SURFACE(((1.0059372961562,0.685883449975777,1.03799914827316),
(1.00593804189723,0.685843996057386,1.03800392107261),(1.00593602425211,
0.685950740896645,1.03799100798995),(1.00593815920701,0.685837789706304,
1.03800467186417),(1.00594039944253,0.685719268576007,1.03801900954234),
(1.00593956271628,0.685763536127451,1.03801365443052)))
REPRESENTATION_ITEM('')
SURFACE()
);
#1599=(
BOUNDED_SURFACE()
B_SPLINE_SURFACE(3,2,((#42908,#42909,#42910),(#42911,#42912,#42913),(#42914,
#42915,#42916),(#42917,#42918,#42919),(#42920,#42921,#42922),(#42923,#42924,
#42925)),.UNSPECIFIED.,.F.,.F.,.F.)
B_SPLINE_SURFACE_WITH_KNOTS((4,1,1,4),(3,3),(0.00208245624318126,0.00585171550471199,
0.00743791339961705,0.0096209724434026),(-0.0634162322184188,1.00964045485374),
 .UNSPECIFIED.)
GEOMETRIC_REPRESENTATION_ITEM()
RATIONAL_B_SPLINE_SURFACE(((1.0395067583518,0.685330296084069,1.0057020621191),
(1.03951179919293,0.685290145992003,1.00570278967029),(1.03949841639537,
0.685396739423676,1.00570085811361),(1.03951261007788,0.685283687326768,
1.00570290670638),(1.03952817116967,0.685159743871252,1.00570515265912),
(1.0395222844102,0.685206631668106,1.00570430301542)))
REPRESENTATION_ITEM('')
SURFACE()
);
#1600=(
BOUNDED_SURFACE()
B_SPLINE_SURFACE(3,2,((#42926,#42927,#42928),(#42929,#42930,#42931),(#42932,
#42933,#42934),(#42935,#42936,#42937),(#42938,#42939,#42940),(#42941,#42942,
#42943)),.UNSPECIFIED.,.F.,.F.,.F.)
B_SPLINE_SURFACE_WITH_KNOTS((4,1,1,4),(3,3),(0.00207550115510636,0.00583206770309977,
0.00741292302561788,0.00958862921574725),(-0.0139548191437294,1.00546415117684),
 .UNSPECIFIED.)
GEOMETRIC_REPRESENTATION_ITEM()
RATIONAL_B_SPLINE_SURFACE(((1.00828942257687,0.701345444582124,1.00321862782116),
(1.00828980522591,0.701331658352956,1.00321877639663),(1.00828751542455,
0.701414156211213,1.00321788730956),(1.00829030395828,0.701313689828347,
1.00321897004508),(1.0082938627312,0.701185472967017,1.00322035185008),
(1.00829178378737,0.701260373967849,1.00321954463505)))
REPRESENTATION_ITEM('')
SURFACE()
);
#1601=(
BOUNDED_SURFACE()
B_SPLINE_SURFACE(3,2,((#42979,#42980,#42981),(#42982,#42983,#42984),(#42985,
#42986,#42987),(#42988,#42989,#42990),(#42991,#42992,#42993),(#42994,#42995,
#42996)),.UNSPECIFIED.,.F.,.F.,.F.)
B_SPLINE_SURFACE_WITH_KNOTS((4,1,1,4),(3,3),(0.00562012573083522,0.00630029289699113,
0.00664037648006909,0.00698046006314705),(0.,1.00004938595224),
 .UNSPECIFIED.)
GEOMETRIC_REPRESENTATION_ITEM()
RATIONAL_B_SPLINE_SURFACE(((1.,0.704092907135692,1.00002922730711),(1.,
0.704090406431475,1.00002922755411),(1.,0.703664702577133,1.00002926960169),
(1.,0.702970262149341,1.0000293381929),(1.,0.703271663610187,1.0000293084229),
(1.,0.703272425211359,1.00002930834768)))
REPRESENTATION_ITEM('')
SURFACE()
);
#1602=(
BOUNDED_SURFACE()
B_SPLINE_SURFACE(3,2,((#43011,#43012,#43013),(#43014,#43015,#43016),(#43017,
#43018,#43019),(#43020,#43021,#43022),(#43023,#43024,#43025),(#43026,#43027,
#43028)),.UNSPECIFIED.,.F.,.F.,.F.)
B_SPLINE_SURFACE_WITH_KNOTS((4,1,1,4),(3,3),(0.00207453111129043,0.00583682887046017,
0.00742009603050453,0.00959912157199512),(-0.00709208229884144,1.01455199349045),
 .UNSPECIFIED.)
GEOMETRIC_REPRESENTATION_ITEM()
RATIONAL_B_SPLINE_SURFACE(((1.00418431442723,0.700677941873041,1.00864924429771),
(1.00418449834326,0.700664785565795,1.00864962446387),(1.00418333960424,
0.700747675165923,1.00864722927654),(1.00418479483858,0.700643575977048,
1.00865023733856),(1.00418663690651,0.700511804913243,1.00865404501023),
(1.00418553484717,0.700590639970702,1.00865176698343)))
REPRESENTATION_ITEM('')
SURFACE()
);
#1603=(
BOUNDED_SURFACE()
B_SPLINE_SURFACE(3,2,((#43051,#43052,#43053),(#43054,#43055,#43056),(#43057,
#43058,#43059),(#43060,#43061,#43062),(#43063,#43064,#43065),(#43066,#43067,
#43068)),.UNSPECIFIED.,.F.,.F.,.F.)
B_SPLINE_SURFACE_WITH_KNOTS((4,1,1,4),(3,3),(0.00211751772537189,0.00570450909625921,
0.00721400412766881,0.00929149854507189),(-0.00844675675792914,1.05533037709487),
 .UNSPECIFIED.)
GEOMETRIC_REPRESENTATION_ITEM()
RATIONAL_B_SPLINE_SURFACE(((1.00499014862227,0.688130707990867,1.03420759866455),
(1.00499072016438,0.688094988326579,1.0342115166006),(1.00498920859429,
0.688189456914593,1.03420115474828),(1.00499054744122,0.688105783004858,
1.03421033257886),(1.00499226460991,0.687998465122432,1.0342221038149),
(1.0049914820894,0.688047370302582,1.03421673961645)))
REPRESENTATION_ITEM('')
SURFACE()
);
#1604=(
BOUNDED_SURFACE()
B_SPLINE_SURFACE(3,2,((#43083,#43084,#43085),(#43086,#43087,#43088),(#43089,
#43090,#43091),(#43092,#43093,#43094),(#43095,#43096,#43097),(#43098,#43099,
#43100)),.UNSPECIFIED.,.F.,.F.,.F.)
B_SPLINE_SURFACE_WITH_KNOTS((4,1,1,4),(3,3),(0.00606474645459548,0.00687768219289253,
0.00721978592523264,0.00769061870795424),(-0.00208860429383766,1.00954344417007),
 .UNSPECIFIED.)
GEOMETRIC_REPRESENTATION_ITEM()
RATIONAL_B_SPLINE_SURFACE(((1.00124267640761,0.699665335788881,1.00572039361805),
(1.00124236841496,0.699739772599195,1.00571897584013),(1.00124365335567,
0.699429223342106,1.00572489078835),(1.00123971608937,0.700380796529177,
1.00570676642965),(1.00123395160836,0.701773977778471,1.00568023088088),
(1.00123674694762,0.701098389771248,1.00569309862406)))
REPRESENTATION_ITEM('')
SURFACE()
);
#1605=(
BOUNDED_SURFACE()
B_SPLINE_SURFACE(3,2,((#43115,#43116,#43117),(#43118,#43119,#43120),(#43121,
#43122,#43123),(#43124,#43125,#43126),(#43127,#43128,#43129),(#43130,#43131,
#43132)),.UNSPECIFIED.,.F.,.F.,.F.)
B_SPLINE_SURFACE_WITH_KNOTS((4,1,1,4),(3,3),(0.00211111585136037,0.00418032934692781,
0.00568380331161446,0.00925648951110398),(-0.00558429959324884,1.05817709439886),
 .UNSPECIFIED.)
GEOMETRIC_REPRESENTATION_ITEM()
RATIONAL_B_SPLINE_SURFACE(((1.00329060357544,0.688134171423838,1.03607436996445),
(1.00329116786007,0.688080691540763,1.03608055612821),(1.00328994720374,
0.688196378826951,1.03606717426467),(1.00328910968704,0.688275754186287,
1.03605799270062),(1.00329008190375,0.688183612679626,1.03606865095971),
(1.00328970654605,0.688219187077167,1.03606453597223)))
REPRESENTATION_ITEM('')
SURFACE()
);
#1606=(
BOUNDED_SURFACE()
B_SPLINE_SURFACE(3,2,((#43133,#43134,#43135),(#43136,#43137,#43138),(#43139,
#43140,#43141),(#43142,#43143,#43144),(#43145,#43146,#43147),(#43148,#43149,
#43150)),.UNSPECIFIED.,.F.,.F.,.F.)
B_SPLINE_SURFACE_WITH_KNOTS((4,1,1,4),(3,3),(0.00206989346412758,0.00402645380207103,
0.00544807632115799,0.00882626159430671),(-0.00595850905898064,1.01180195773527),
 .UNSPECIFIED.)
GEOMETRIC_REPRESENTATION_ITEM()
RATIONAL_B_SPLINE_SURFACE(((1.0035120861051,0.701789401008881,1.0069967612183),
(1.00351252080015,0.701752491130503,1.00699762721571),(1.00351163037285,
0.701828097151536,1.0069958533107),(1.00351087607069,0.701892144812239,
1.00699435059353),(1.00351171129339,0.70182122620348,1.0069960145202),(1.00351156571752,
0.701833587024572,1.00699572450464)))
REPRESENTATION_ITEM('')
SURFACE()
);
#1607=(
BOUNDED_SURFACE()
B_SPLINE_SURFACE(3,2,((#43172,#43173,#43174),(#43175,#43176,#43177),(#43178,
#43179,#43180),(#43181,#43182,#43183),(#43184,#43185,#43186),(#43187,#43188,
#43189)),.UNSPECIFIED.,.F.,.F.,.F.)
B_SPLINE_SURFACE_WITH_KNOTS((4,1,1,4),(3,3),(0.00579676790523706,0.00657748490359677,
0.0069060300593971,0.00735820154402503),(0.,1.01353017141622),
 .UNSPECIFIED.)
GEOMETRIC_REPRESENTATION_ITEM()
RATIONAL_B_SPLINE_SURFACE(((1.,0.699822260672061,1.00812291253688),(1.,
0.699895928175691,1.00812091906898),(1.,0.699649690014438,1.00812758235804),
(1.,0.69899042483752,1.00814542229975),(1.,0.699390436250587,1.00813459785377),
(1.,0.699218266641026,1.00813925682243)))
REPRESENTATION_ITEM('')
SURFACE()
);
#1608=(
BOUNDED_SURFACE()
B_SPLINE_SURFACE(3,2,((#43233,#43234,#43235),(#43236,#43237,#43238),(#43239,
#43240,#43241),(#43242,#43243,#43244),(#43245,#43246,#43247)),
 .UNSPECIFIED.,.F.,.F.,.F.)
B_SPLINE_SURFACE_WITH_KNOTS((4,1,4),(3,3),(0.00217494176891105,0.00539842225200163,
0.00863013951237006),(-0.00371571512923231,1.05640803844583),
 .UNSPECIFIED.)
GEOMETRIC_REPRESENTATION_ITEM()
RATIONAL_B_SPLINE_SURFACE(((1.00218484151612,0.689354498488246,1.03490916812134),
(1.00218506494712,0.689322730584858,1.03491273807833),(1.00218418879701,
0.689447303506582,1.03489873904391),(1.00218536490516,0.689280081900558,
1.03491753077638),(1.00218509616368,0.689318292146319,1.03491323685329)))
REPRESENTATION_ITEM('')
SURFACE()
);
#1609=(
BOUNDED_SURFACE()
B_SPLINE_SURFACE(3,2,((#43263,#43264,#43265),(#43266,#43267,#43268),(#43269,
#43270,#43271),(#43272,#43273,#43274),(#43275,#43276,#43277)),
 .UNSPECIFIED.,.F.,.F.,.F.)
B_SPLINE_SURFACE_WITH_KNOTS((4,1,4),(3,3),(0.00576650017740751,0.00655247885962792,
0.00733845477348281),(0.,1.05287365404843),.UNSPECIFIED.)
GEOMETRIC_REPRESENTATION_ITEM()
RATIONAL_B_SPLINE_SURFACE(((1.,0.68746170886739,1.03305008296447),(1.,0.687609668253521,
1.03303443665767),(1.,0.686759401653278,1.03312435006181),(1.,0.689240361632676,
1.0328619952225),(1.,0.688759740156979,1.03291281964977)))
REPRESENTATION_ITEM('')
SURFACE()
);
#1610=(
BOUNDED_SURFACE()
B_SPLINE_SURFACE(3,2,((#43292,#43293,#43294),(#43295,#43296,#43297),(#43298,
#43299,#43300),(#43301,#43302,#43303),(#43304,#43305,#43306)),
 .UNSPECIFIED.,.F.,.F.,.F.)
B_SPLINE_SURFACE_WITH_KNOTS((4,1,4),(3,3),(0.00213679191355045,0.00535178046044285,
0.00855851013636219),(-0.00508088630754948,1.05456301268146),
 .UNSPECIFIED.)
GEOMETRIC_REPRESENTATION_ITEM()
RATIONAL_B_SPLINE_SURFACE(((1.00299197946971,0.689418739054714,1.03371234749458),
(1.00299234361822,0.689380938761304,1.03371645056449),(1.00299073389702,
0.689548035241304,1.03369831291323),(1.00299192835185,0.689424045324576,
1.03371177152031),(1.00299162252656,0.689455791399116,1.03370832561152)))
REPRESENTATION_ITEM('')
SURFACE()
);
#1611=(
BOUNDED_SURFACE()
B_SPLINE_SURFACE(3,2,((#43307,#43308,#43309),(#43310,#43311,#43312),(#43313,
#43314,#43315),(#43316,#43317,#43318),(#43319,#43320,#43321)),
 .UNSPECIFIED.,.F.,.F.,.F.)
B_SPLINE_SURFACE_WITH_KNOTS((4,1,4),(3,3),(0.00206760785143967,0.00523238397297043,
0.00839715035804973),(-0.00490441686180068,1.01404629551803),
 .UNSPECIFIED.)
GEOMETRIC_REPRESENTATION_ITEM()
RATIONAL_B_SPLINE_SURFACE(((1.00288754135804,0.701463125129675,1.00834517917058),
(1.00288769200597,0.701447549954039,1.00834561455275),(1.00288651080142,
0.701569672227322,1.00834220079607),(1.00288740164171,0.70147757010922,
1.00834477538146),(1.00288728891469,0.701489224720478,1.00834444959317)))
REPRESENTATION_ITEM('')
SURFACE()
);
#1612=(
BOUNDED_SURFACE()
B_SPLINE_SURFACE(3,2,((#43361,#43362,#43363),(#43364,#43365,#43366),(#43367,
#43368,#43369),(#43370,#43371,#43372),(#43373,#43374,#43375)),
 .UNSPECIFIED.,.F.,.F.,.F.)
B_SPLINE_SURFACE_WITH_KNOTS((4,1,4),(3,3),(0.002170029345752,0.00533298360778802,
0.00849593060227173),(-0.00937893121976585,1.01422351742609),
 .UNSPECIFIED.)
GEOMETRIC_REPRESENTATION_ITEM()
RATIONAL_B_SPLINE_SURFACE(((1.00554607201155,0.700088980780457,1.00845120436019),
(1.00554628250909,0.700077597854026,1.00845152512012),(1.00554458089537,
0.700169614817188,1.00844893217051),(1.00554685665382,0.700046550234841,
1.0084524000122),(1.00554656556966,0.700062290987494,1.00845195645291)))
REPRESENTATION_ITEM('')
SURFACE()
);
#1613=(
BOUNDED_SURFACE()
B_SPLINE_SURFACE(3,2,((#43389,#43390,#43391),(#43392,#43393,#43394),(#43395,
#43396,#43397),(#43398,#43399,#43400),(#43401,#43402,#43403)),
 .UNSPECIFIED.,.F.,.F.,.F.)
B_SPLINE_SURFACE_WITH_KNOTS((4,1,4),(3,3),(0.00219592593545592,0.00532324237200424,
0.00845896001036928),(-0.00320737611465728,1.04761084667385),
 .UNSPECIFIED.)
GEOMETRIC_REPRESENTATION_ITEM()
RATIONAL_B_SPLINE_SURFACE(((1.00188499121938,0.692112164947285,1.02921962346904),
(1.00188517626665,0.692081939977089,1.02922249192355),(1.00188445707106,
0.692199410855367,1.02921134352975),(1.00188535828696,0.692052209419153,
1.02922531345662),(1.00188512579573,0.69209018372002,1.02922170956375)))
REPRESENTATION_ITEM('')
SURFACE()
);
#1614=(
BOUNDED_SURFACE()
B_SPLINE_SURFACE(3,2,((#43430,#43431,#43432),(#43433,#43434,#43435),(#43436,
#43437,#43438),(#43439,#43440,#43441),(#43442,#43443,#43444)),
 .UNSPECIFIED.,.F.,.F.,.F.)
B_SPLINE_SURFACE_WITH_KNOTS((4,1,4),(3,3),(0.00211122737223723,0.00524610948281742,
0.00837256921945858),(-0.00425993730565382,1.04600237267559),
 .UNSPECIFIED.)
GEOMETRIC_REPRESENTATION_ITEM()
RATIONAL_B_SPLINE_SURFACE(((1.00250639350022,0.692227555543412,1.02819115126479),
(1.00250670366833,0.692189468469,1.02819463994123),(1.00250550329272,0.692336868521937,
1.02818113848175),(1.00250645781776,0.692219657675385,1.02819187468885),
(1.00250621151727,0.692249902129454,1.02818910437593)))
REPRESENTATION_ITEM('')
SURFACE()
);
#1615=(
BOUNDED_SURFACE()
B_SPLINE_SURFACE(3,2,((#43445,#43446,#43447),(#43448,#43449,#43450),(#43451,
#43452,#43453),(#43454,#43455,#43456),(#43457,#43458,#43459)),
 .UNSPECIFIED.,.F.,.F.,.F.)
B_SPLINE_SURFACE_WITH_KNOTS((4,1,4),(3,3),(0.006583329098368,0.00749456862587076,
0.00840580588587755),(-0.00374155041453272,1.03290826060198),
 .UNSPECIFIED.)
GEOMETRIC_REPRESENTATION_ITEM()
RATIONAL_B_SPLINE_SURFACE(((1.00222383231565,0.693003259388743,1.0201277491697),
(1.00222310392596,0.693103812501358,1.02012115656607),(1.00222748707377,
0.692498725470239,1.02016082812728),(1.00220858018415,0.695108793436242,
1.01998970320514),(1.00221230047744,0.694595212485627,1.02002337531687)))
REPRESENTATION_ITEM('')
SURFACE()
);
#1616=(
BOUNDED_SURFACE()
B_SPLINE_SURFACE(3,2,((#43490,#43491,#43492),(#43493,#43494,#43495),(#43496,
#43497,#43498),(#43499,#43500,#43501),(#43502,#43503,#43504)),
 .UNSPECIFIED.,.F.,.F.,.F.)
B_SPLINE_SURFACE_WITH_KNOTS((4,1,4),(3,3),(0.00227074891388854,0.00518182924437649,
0.00809291038442371),(-0.0057448981998482,1.00828145765618),
 .UNSPECIFIED.)
GEOMETRIC_REPRESENTATION_ITEM()
RATIONAL_B_SPLINE_SURFACE(((1.00338492186034,0.702943903419068,1.00489178136424),
(1.00338501455575,0.702935768597727,1.00489191532468),(1.00338425005556,
0.703002860084568,1.00489081049335),(1.00338494782254,0.702941625012127,
1.00489181888398),(1.00338502158477,0.702935151740146,1.00489192548281)))
REPRESENTATION_ITEM('')
SURFACE()
);
#1617=(
BOUNDED_SURFACE()
B_SPLINE_SURFACE(3,2,((#43550,#43551,#43552),(#43553,#43554,#43555),(#43556,
#43557,#43558),(#43559,#43560,#43561),(#43562,#43563,#43564)),
 .UNSPECIFIED.,.F.,.F.,.F.)
B_SPLINE_SURFACE_WITH_KNOTS((4,1,4),(3,3),(0.00345689067726456,0.00436603992331825,
0.00527519124507475),(-0.0036794560107073,1.03264354334434),
 .UNSPECIFIED.)
GEOMETRIC_REPRESENTATION_ITEM()
RATIONAL_B_SPLINE_SURFACE(((1.00217552367056,0.694683016928517,1.01985788040247),
(1.00217188868089,0.695193158047507,1.01982470071745),(1.00219036149319,
0.692600649680304,1.01999331800359),(1.00218608865275,0.693200307946796,
1.01995431610459),(1.00218679920266,0.693100588068842,1.0199608019063)))
REPRESENTATION_ITEM('')
SURFACE()
);
#1618=(
BOUNDED_SURFACE()
B_SPLINE_SURFACE(3,2,((#43565,#43566,#43567),(#43568,#43569,#43570),(#43571,
#43572,#43573),(#43574,#43575,#43576),(#43577,#43578,#43579)),
 .UNSPECIFIED.,.F.,.F.,.F.)
B_SPLINE_SURFACE_WITH_KNOTS((4,1,4),(3,3),(0.00222417800671133,0.00530805645561326,
0.00839192864935772),(-0.00406685372208074,1.04107360049962),
 .UNSPECIFIED.)
GEOMETRIC_REPRESENTATION_ITEM()
RATIONAL_B_SPLINE_SURFACE(((1.00239216177419,0.693766408819533,1.02505033698307),
(1.00239239865957,0.693736083838975,1.02505281760898),(1.00239149665043,
0.693851554916822,1.02504337191296),(1.00239258464149,0.693712275286194,
1.02505476518197),(1.00239228636051,0.693750459849733,1.02505164163115)))
REPRESENTATION_ITEM('')
SURFACE()
);
#1619=(
BOUNDED_SURFACE()
B_SPLINE_SURFACE(3,2,((#43654,#43655,#43656),(#43657,#43658,#43659),(#43660,
#43661,#43662),(#43663,#43664,#43665),(#43666,#43667,#43668)),
 .UNSPECIFIED.,.F.,.F.,.F.)
B_SPLINE_SURFACE_WITH_KNOTS((4,1,4),(3,3),(0.00211355742364673,0.00519233852776365,
0.00827111050613143),(-0.0051509153970441,1.00869647758464),
 .UNSPECIFIED.)
GEOMETRIC_REPRESENTATION_ITEM()
RATIONAL_B_SPLINE_SURFACE(((1.00303335472695,0.702978094692853,1.00513938789791),
(1.00303346790981,0.702967011983877,1.00513957966269),(1.00303238072114,
0.703073467997359,1.00513773764789),(1.00303327408742,0.702985990804776,
1.00513925127101),(1.00303316117799,0.702997046740221,1.0051390599695)))
REPRESENTATION_ITEM('')
SURFACE()
);
#1620=(
BOUNDED_SURFACE()
B_SPLINE_SURFACE(3,2,((#43683,#43684,#43685),(#43686,#43687,#43688),(#43689,
#43690,#43691),(#43692,#43693,#43694),(#43695,#43696,#43697)),
 .UNSPECIFIED.,.F.,.F.,.F.)
B_SPLINE_SURFACE_WITH_KNOTS((4,1,4),(3,3),(0.0022123564208203,0.00528826645871868,
0.00836416483792585),(-0.00574674248185728,1.00871944995166),
 .UNSPECIFIED.)
GEOMETRIC_REPRESENTATION_ITEM()
RATIONAL_B_SPLINE_SURFACE(((1.00338602967336,0.702812271509221,1.00515275950288),
(1.00338615667078,0.702801125099646,1.00515295276378),(1.00338515382689,
0.702889143494477,1.00515142666571),(1.00338636185634,0.702783116211503,
1.00515326500907),(1.00338623721726,0.702794055632565,1.00515307533702)))
REPRESENTATION_ITEM('')
SURFACE()
);
#1621=(
BOUNDED_SURFACE()
B_SPLINE_SURFACE(3,2,((#43698,#43699,#43700),(#43701,#43702,#43703),(#43704,
#43705,#43706),(#43707,#43708,#43709),(#43710,#43711,#43712)),
 .UNSPECIFIED.,.F.,.F.,.F.)
B_SPLINE_SURFACE_WITH_KNOTS((4,1,4),(3,3),(0.00221964849955536,0.00530337508156829,
0.00838709540025036),(-0.00386775963484442,1.04349299216076),
 .UNSPECIFIED.)
GEOMETRIC_REPRESENTATION_ITEM()
RATIONAL_B_SPLINE_SURFACE(((1.00227460680574,0.693114664954495,1.02658760232749),
(1.00227483592651,0.693083752445582,1.02659028049226),(1.00227396352775,
0.693201454716058,1.02658008312926),(1.00227500636979,0.693060756584338,
1.02659227278301),(1.00227472193803,0.693099131539325,1.02658894809484)))
REPRESENTATION_ITEM('')
SURFACE()
);
#1622=(
BOUNDED_SURFACE()
B_SPLINE_SURFACE(3,2,((#43742,#43743,#43744),(#43745,#43746,#43747),(#43748,
#43749,#43750),(#43751,#43752,#43753),(#43754,#43755,#43756)),
 .UNSPECIFIED.,.F.,.F.,.F.)
B_SPLINE_SURFACE_WITH_KNOTS((4,1,4),(3,3),(0.00213713482294571,0.00521861296289499,
0.00830007897582003),(-0.004774040707985,1.04045105083211),
 .UNSPECIFIED.)
GEOMETRIC_REPRESENTATION_ITEM()
RATIONAL_B_SPLINE_SURFACE(((1.00281025847898,0.693710559793116,1.02465716856158),
(1.00281060986467,0.693672262345152,1.02466025161475),(1.0028093248937,
0.693812311042481,1.02464897729744),(1.00281040793758,0.693694270333668,
1.02465847990926),(1.00281012318337,0.69372530563075,1.02465598147983)))
REPRESENTATION_ITEM('')
SURFACE()
);
#1623=(
BOUNDED_SURFACE()
B_SPLINE_SURFACE(3,2,((#43803,#43804,#43805),(#43806,#43807,#43808),(#43809,
#43810,#43811),(#43812,#43813,#43814),(#43815,#43816,#43817)),
 .UNSPECIFIED.,.F.,.F.,.F.)
B_SPLINE_SURFACE_WITH_KNOTS((4,1,4),(3,3),(0.0021088933074858,0.00518762498109073,
0.00826634651087212),(-0.00504323689701123,1.00761456883791),
 .UNSPECIFIED.)
GEOMETRIC_REPRESENTATION_ITEM()
RATIONAL_B_SPLINE_SURFACE(((1.00296962652022,0.703330175196368,1.00449518400848),
(1.00296973954876,0.703318883488138,1.00449535510207),(1.00296866453602,
0.703426278757948,1.00449372783344),(1.00296955720505,0.703337099878823,
1.00449507908469),(1.00296944388406,0.703348420802902,1.00449490754841)))
REPRESENTATION_ITEM('')
SURFACE()
);
#1624=(
BOUNDED_SURFACE()
B_SPLINE_SURFACE(3,2,((#43832,#43833,#43834),(#43835,#43836,#43837),(#43838,
#43839,#43840),(#43841,#43842,#43843),(#43844,#43845,#43846)),
 .UNSPECIFIED.,.F.,.F.,.F.)
B_SPLINE_SURFACE_WITH_KNOTS((4,1,4),(3,3),(0.00220768902546015,0.00528378993761675,
0.00835987926008497),(-0.00604801792390039,1.00690079957375),
 .UNSPECIFIED.)
GEOMETRIC_REPRESENTATION_ITEM()
RATIONAL_B_SPLINE_SURFACE(((1.0035646205897,0.703260866096649,1.00407068626359),
(1.00356475777255,0.703249446222167,1.00407084292215),(1.00356368106794,
0.703339077189256,1.00406961335886),(1.00356496531083,0.703232169564474,
1.00407107992444),(1.00356483141439,0.70324331585921,1.00407092701886)))
REPRESENTATION_ITEM('')
SURFACE()
);
#1625=(
BOUNDED_SURFACE()
B_SPLINE_SURFACE(3,2,((#43847,#43848,#43849),(#43850,#43851,#43852),(#43853,
#43854,#43855),(#43856,#43857,#43858),(#43859,#43860,#43861)),
 .UNSPECIFIED.,.F.,.F.,.F.)
B_SPLINE_SURFACE_WITH_KNOTS((4,1,4),(3,3),(0.00222405182330376,0.00529888890448264,
0.00838256300938198),(0.,1.04068598403832),.UNSPECIFIED.)
GEOMETRIC_REPRESENTATION_ITEM()
RATIONAL_B_SPLINE_SURFACE(((1.,0.695167345048307,1.02480483306745),(1.,
0.695136783885436,1.02480731988941),(1.,0.695255069647583,1.02479769474415),
(1.,0.695114492118214,1.02480913381439),(1.,0.695152707362112,1.02480602416478)))
REPRESENTATION_ITEM('')
SURFACE()
);
#1626=(
BOUNDED_SURFACE()
B_SPLINE_SURFACE(3,2,((#43891,#43892,#43893),(#43894,#43895,#43896),(#43897,
#43898,#43899),(#43900,#43901,#43902),(#43903,#43904,#43905)),
 .UNSPECIFIED.,.F.,.F.,.F.)
B_SPLINE_SURFACE_WITH_KNOTS((4,1,4),(3,3),(0.00213250098277698,0.00521408838432189,
0.00829566364757425),(-0.00540301929015671,1.03776088171629),
 .UNSPECIFIED.)
GEOMETRIC_REPRESENTATION_ITEM()
RATIONAL_B_SPLINE_SURFACE(((1.00318250272087,0.694307713339714,1.02295786527358),
(1.00318290152577,0.694269406511714,1.02296074216329),(1.00318143614362,
0.694410162408009,1.02295017122302),(1.00318268085919,0.694290602431972,
1.02295915032371),(1.00318235429806,0.694321969951759,1.02295679458454)))
REPRESENTATION_ITEM('')
SURFACE()
);
#1627=(
BOUNDED_SURFACE()
B_SPLINE_SURFACE(3,2,((#43951,#43952,#43953),(#43954,#43955,#43956),(#43957,
#43958,#43959),(#43960,#43961,#43962),(#43963,#43964,#43965)),
 .UNSPECIFIED.,.F.,.F.,.F.)
B_SPLINE_SURFACE_WITH_KNOTS((4,1,4),(3,3),(0.00218672559995519,0.00518296150941844,
0.00817918722256176),(-0.00482832253702671,1.00621350692926),
 .UNSPECIFIED.)
GEOMETRIC_REPRESENTATION_ITEM()
RATIONAL_B_SPLINE_SURFACE(((1.00284247866485,0.703807557313486,1.00366299226778),
(1.00284255386132,0.7037997216781,1.00366308917056),(1.00284156785576,0.703902465596022,
1.00366181854335),(1.00284239085209,0.703816707593733,1.00366287910687),
(1.00284231050323,0.703825080118213,1.00366277556442)))
REPRESENTATION_ITEM('')
SURFACE()
);
#1628=(
BOUNDED_SURFACE()
B_SPLINE_SURFACE(3,2,((#43980,#43981,#43982),(#43983,#43984,#43985),(#43986,
#43987,#43988),(#43989,#43990,#43991),(#43992,#43993,#43994)),
 .UNSPECIFIED.,.F.,.F.,.F.)
B_SPLINE_SURFACE_WITH_KNOTS((4,1,4),(3,3),(0.00236713033829012,0.00527934748302146,
0.00819155303031432),(0.,1.00557059275432),.UNSPECIFIED.)
GEOMETRIC_REPRESENTATION_ITEM()
RATIONAL_B_SPLINE_SURFACE(((1.,0.705444427620648,1.00328169827448),(1.,
0.705438897999593,1.00328175988101),(1.,0.705519693531559,1.003280859723),
(1.,0.705423279098818,1.00328193389409),(1.,0.70542771532932,1.00328188446922)))
REPRESENTATION_ITEM('')
SURFACE()
);
#1629=(
BOUNDED_SURFACE()
B_SPLINE_SURFACE(3,2,((#43995,#43996,#43997),(#43998,#43999,#44000),(#44001,
#44002,#44003),(#44004,#44005,#44006),(#44007,#44008,#44009)),
 .UNSPECIFIED.,.F.,.F.,.F.)
B_SPLINE_SURFACE_WITH_KNOTS((4,1,4),(3,3),(0.00221984090545246,0.0052945704827959,
0.00837825146220991),(0.,1.03829076028441),.UNSPECIFIED.)
GEOMETRIC_REPRESENTATION_ITEM()
RATIONAL_B_SPLINE_SURFACE(((1.,0.695868122289244,1.02329088164854),(1.,
0.69583719577093,1.02329325004834),(1.,0.695957181965263,1.02328406132313),
(1.,0.695815936027,1.02329487815185),(1.,0.69585416407111,1.02329195059011)))
REPRESENTATION_ITEM('')
SURFACE()
);
#1630=(
BOUNDED_SURFACE()
B_SPLINE_SURFACE(3,2,((#44039,#44040,#44041),(#44042,#44043,#44044),(#44045,
#44046,#44047),(#44048,#44049,#44050),(#44051,#44052,#44053)),
 .UNSPECIFIED.,.F.,.F.,.F.)
B_SPLINE_SURFACE_WITH_KNOTS((4,1,4),(3,3),(0.00212794996907239,0.00520974641510763,
0.00829153071066992),(-0.00525793491290963,1.0362694004451),
 .UNSPECIFIED.)
GEOMETRIC_REPRESENTATION_ITEM()
RATIONAL_B_SPLINE_SURFACE(((1.00309659972907,0.69479472099637,1.02201939623592),
(1.00309698870907,0.694756382573413,1.02202216220684),(1.00309555288293,
0.694897899641948,1.02201195229036),(1.00309678377646,0.694776581022652,
1.0220207049658),(1.00309646159645,0.694808335543697,1.02201841399828)))
REPRESENTATION_ITEM('')
SURFACE()
);
#1631=(
BOUNDED_SURFACE()
B_SPLINE_SURFACE(3,2,((#44099,#44100,#44101),(#44102,#44103,#44104),(#44105,
#44106,#44107),(#44108,#44109,#44110),(#44111,#44112,#44113)),
 .UNSPECIFIED.,.F.,.F.,.F.)
B_SPLINE_SURFACE_WITH_KNOTS((4,1,4),(3,3),(0.00233053591587337,0.00517834652518091,
0.00802614698836607),(-7.3643504785873E-5,1.00515727646814),
 .UNSPECIFIED.)
GEOMETRIC_REPRESENTATION_ITEM()
RATIONAL_B_SPLINE_SURFACE(((1.00004314960779,0.705526245967311,1.00303714031107),
(1.00004314993106,0.705524039760155,1.00303716306543),(1.00004313623197,
0.705617528983217,1.00303619883726),(1.00004314767456,0.705539439208663,
1.00303700423876),(1.00004314716727,0.705542901193404,1.00303696853258)))
REPRESENTATION_ITEM('')
SURFACE()
);
#1632=(
BOUNDED_SURFACE()
B_SPLINE_SURFACE(3,2,((#44128,#44129,#44130),(#44131,#44132,#44133),(#44134,
#44135,#44136),(#44137,#44138,#44139),(#44140,#44141,#44142)),
 .UNSPECIFIED.,.F.,.F.,.F.)
B_SPLINE_SURFACE_WITH_KNOTS((4,1,4),(3,3),(0.0024368838680126,0.00527506449450404,
0.00811323354646179),(0.,1.0046118093486),.UNSPECIFIED.)
GEOMETRIC_REPRESENTATION_ITEM()
RATIONAL_B_SPLINE_SURFACE(((1.,0.705724192469964,1.00271428784047),(1.,
0.705720922940111,1.00271431799736),(1.,0.705798756048654,1.00271360009445),
(1.,0.705706251659519,1.00271445331966),(1.,0.705708115890236,1.00271443612471)))
REPRESENTATION_ITEM('')
SURFACE()
);
#1633=(
BOUNDED_SURFACE()
B_SPLINE_SURFACE(3,2,((#44143,#44144,#44145),(#44146,#44147,#44148),(#44149,
#44150,#44151),(#44152,#44153,#44154),(#44155,#44156,#44157)),
 .UNSPECIFIED.,.F.,.F.,.F.)
B_SPLINE_SURFACE_WITH_KNOTS((4,1,4),(3,3),(0.00216602181407597,0.0052489536371796,
0.0083318848142593),(-0.0444466707917243,1.0051340701333),.UNSPECIFIED.)
GEOMETRIC_REPRESENTATION_ITEM()
RATIONAL_B_SPLINE_SURFACE(((1.02719646592756,0.69241749798202,1.00302324092364),
(1.027199787454,0.69237993268158,1.00302361015451),(1.02718810626605,0.692512042825083,
1.00302231163853),(1.02719782769207,0.692402096902532,1.00302339230148),
(1.02719527830541,0.692430929572478,1.00302310890399)))
REPRESENTATION_ITEM('')
SURFACE()
);
#1634=(
BOUNDED_SURFACE()
B_SPLINE_SURFACE(3,2,((#44186,#44187,#44188),(#44189,#44190,#44191),(#44192,
#44193,#44194),(#44195,#44196,#44197),(#44198,#44199,#44200)),
 .UNSPECIFIED.,.F.,.F.,.F.)
B_SPLINE_SURFACE_WITH_KNOTS((4,1,4),(3,3),(0.00216545784130295,0.00524970120976066,
0.00833394389446095),(-0.0058777833286939,1.04293073295283),
 .UNSPECIFIED.)
GEOMETRIC_REPRESENTATION_ITEM()
RATIONAL_B_SPLINE_SURFACE(((1.00346373556471,0.692630283187857,1.02623068962352),
(1.00346415610398,0.692592964796872,1.02623387434562),(1.00346268565001,
0.692723451957841,1.02622273867404),(1.00346391422394,0.6926144290796,1.02623204260063),
(1.003463585266,0.692643620600768,1.0262295514192)))
REPRESENTATION_ITEM('')
SURFACE()
);
#1635=(
BOUNDED_SURFACE()
B_SPLINE_SURFACE(3,2,((#44248,#44249,#44250),(#44251,#44252,#44253),(#44254,
#44255,#44256),(#44257,#44258,#44259),(#44260,#44261,#44262)),
 .UNSPECIFIED.,.F.,.F.,.F.)
B_SPLINE_SURFACE_WITH_KNOTS((4,1,4),(3,3),(0.00213816488674072,0.00521583965643689,
0.00829351555392586),(-0.00552986428889216,1.01473434870462),
 .UNSPECIFIED.)
GEOMETRIC_REPRESENTATION_ITEM()
RATIONAL_B_SPLINE_SURFACE(((1.00325771456763,0.701079567892973,1.00875965270882),
(1.00325781626736,0.701070236158245,1.00875992616873),(1.00325673379108,
0.701169561703866,1.00875701550358),(1.00325763395525,0.701086964700353,
1.00875943595059),(1.0032575157888,0.701097807383465,1.00875911821339)))
REPRESENTATION_ITEM('')
SURFACE()
);
#1636=(
BOUNDED_SURFACE()
B_SPLINE_SURFACE(3,2,((#44276,#44277,#44278),(#44279,#44280,#44281),(#44282,
#44283,#44284),(#44285,#44286,#44287),(#44288,#44289,#44290)),
 .UNSPECIFIED.,.F.,.F.,.F.)
B_SPLINE_SURFACE_WITH_KNOTS((4,1,4),(3,3),(0.00213779274189611,0.00521727844313784,
0.00829676872894075),(-0.0154960333971323,1.00577171680884),
 .UNSPECIFIED.)
GEOMETRIC_REPRESENTATION_ITEM()
RATIONAL_B_SPLINE_SURFACE(((1.00921938543943,0.700781197642686,1.00340100781529),
(1.00921966265681,0.700772200443111,1.00340111008007),(1.00921664376362,
0.70087017981592,1.00339999641806),(1.00921913287023,0.700789394876286,
1.00340091464315),(1.00921882744111,0.700799307699139,1.00340080197112)))
REPRESENTATION_ITEM('')
SURFACE()
);
#1637=(
BOUNDED_SURFACE()
B_SPLINE_SURFACE(3,2,((#44291,#44292,#44293),(#44294,#44295,#44296),(#44297,
#44298,#44299),(#44300,#44301,#44302),(#44303,#44304,#44305)),
 .UNSPECIFIED.,.F.,.F.,.F.)
B_SPLINE_SURFACE_WITH_KNOTS((4,1,4),(3,3),(0.00221169983238519,0.0052855296342299,
0.0083684987093601),(-0.00324346846181243,1.03300158810162),
 .UNSPECIFIED.)
GEOMETRIC_REPRESENTATION_ITEM()
RATIONAL_B_SPLINE_SURFACE(((1.00190629916672,0.696403174620331,1.01997150835538),
(1.00190649735207,0.696371611661272,1.01997358466135),(1.00190572425457,
0.696494735014529,1.01996548523845),(1.00190662047827,0.696352002607635,
1.01997487460362),(1.00190637972075,0.69639034560195,1.01997235228663)))
REPRESENTATION_ITEM('')
SURFACE()
);
#1638=(
BOUNDED_SURFACE()
B_SPLINE_SURFACE(3,2,((#44336,#44337,#44338),(#44339,#44340,#44341),(#44342,
#44343,#44344),(#44345,#44346,#44347),(#44348,#44349,#44350)),
 .UNSPECIFIED.,.F.,.F.,.F.)
B_SPLINE_SURFACE_WITH_KNOTS((4,1,4),(3,3),(0.00211921303525452,0.00520188789026804,
0.00828455059289162),(-0.00497615288010077,1.03080289128597),
 .UNSPECIFIED.)
GEOMETRIC_REPRESENTATION_ITEM()
RATIONAL_B_SPLINE_SURFACE(((1.00292983108751,0.696499957967487,1.01860202496771),
(1.00293020100174,0.696461638698849,1.01860437361975),(1.00292882376335,
0.696604306277997,1.01859562928531),(1.00293002052061,0.696480334667596,
1.01860322771257),(1.00292970839583,0.696512667549343,1.01860124597619)))
REPRESENTATION_ITEM('')
SURFACE()
);
#1639=(
BOUNDED_SURFACE()
B_SPLINE_SURFACE(3,2,((#44398,#44399,#44400),(#44401,#44402,#44403),(#44404,
#44405,#44406),(#44407,#44408,#44409),(#44410,#44411,#44412)),
 .UNSPECIFIED.,.F.,.F.,.F.)
B_SPLINE_SURFACE_WITH_KNOTS((4,1,4),(3,3),(0.00247806168022139,0.00516920088530873,
0.00786033004716436),(0.,1.00372616184728),.UNSPECIFIED.)
GEOMETRIC_REPRESENTATION_ITEM()
RATIONAL_B_SPLINE_SURFACE(((1.,0.705967000528768,1.00219122908894),(1.,
0.70596966991393,1.00219120919582),(1.,0.706054739691718,1.0021905752283),
(1.,0.705982858434738,1.0021911109107),(0.999999999999999,0.705982071723989,
1.00219111677352)))
REPRESENTATION_ITEM('')
SURFACE()
);
#1640=(
BOUNDED_SURFACE()
B_SPLINE_SURFACE(3,2,((#44427,#44428,#44429),(#44430,#44431,#44432),(#44433,
#44434,#44435),(#44436,#44437,#44438),(#44439,#44440,#44441)),
 .UNSPECIFIED.,.F.,.F.,.F.)
B_SPLINE_SURFACE_WITH_KNOTS((4,1,4),(3,3),(0.00267720881073118,0.00526764836792767,
0.00785808792512416),(0.,1.00296333742759),.UNSPECIFIED.)
GEOMETRIC_REPRESENTATION_ITEM()
RATIONAL_B_SPLINE_SURFACE(((1.,0.706205515038292,1.00174122438661),(1.,
0.706208745150634,1.00174120524278),(1.,0.706275159085219,1.00174081162899),
(1.,0.706196462696256,1.0017412780369),(1.,0.706191126887914,1.0017413096605)))
REPRESENTATION_ITEM('')
SURFACE()
);
#1641=(
BOUNDED_SURFACE()
B_SPLINE_SURFACE(3,2,((#44442,#44443,#44444),(#44445,#44446,#44447),(#44448,
#44449,#44450),(#44451,#44452,#44453),(#44454,#44455,#44456),(#44457,#44458,
#44459)),.UNSPECIFIED.,.F.,.F.,.F.)
B_SPLINE_SURFACE_WITH_KNOTS((4,1,1,4),(3,3),(0.00207740162366139,0.00585323454960992,
0.00744219878966224,0.00962906509384405),(-0.00992421051928284,1.06115213291247),
 .UNSPECIFIED.)
GEOMETRIC_REPRESENTATION_ITEM()
RATIONAL_B_SPLINE_SURFACE(((1.00587156388292,0.685911998576704,1.03801528924904),
(1.00587229355607,0.685872966116927,1.03802001349906),(1.00587030000394,
0.685979607348392,1.03800710629713),(1.00587241313185,0.685866569640664,
1.0380207876894),(1.00587464193811,0.685747343942645,1.03803521803814),
(1.00587381122293,0.685791781451287,1.03802983959408)))
REPRESENTATION_ITEM('')
SURFACE()
);
#1642=(
BOUNDED_SURFACE()
B_SPLINE_SURFACE(3,2,((#44487,#44488,#44489),(#44490,#44491,#44492),(#44493,
#44494,#44495),(#44496,#44497,#44498),(#44499,#44500,#44501),(#44502,#44503,
#44504)),.UNSPECIFIED.,.F.,.F.,.F.)
B_SPLINE_SURFACE_WITH_KNOTS((4,1,1,4),(3,3),(0.00207839781632833,0.00584816658647622,
0.00743457891160079,0.00961793307792553),(-0.0645166657950686,1.00997111844977),
 .UNSPECIFIED.)
GEOMETRIC_REPRESENTATION_ITEM()
RATIONAL_B_SPLINE_SURFACE(((1.04023391045298,0.684892260072604,1.00589957457065),
(1.0402390319118,0.684852149347703,1.00590032553987),(1.04022544444458,
0.684958564956782,1.00589833318379),(1.04023976549679,0.684846403987535,
1.00590043310683),(1.04025602169469,0.684719087161401,1.00590281678395),
(1.04024986609632,0.684767297158138,1.00590191417689)))
REPRESENTATION_ITEM('')
SURFACE()
);
#1643=(
BOUNDED_SURFACE()
B_SPLINE_SURFACE(3,2,((#44565,#44566,#44567),(#44568,#44569,#44570),(#44571,
#44572,#44573),(#44574,#44575,#44576),(#44577,#44578,#44579),(#44580,#44581,
#44582)),.UNSPECIFIED.,.F.,.F.,.F.)
B_SPLINE_SURFACE_WITH_KNOTS((4,1,1,4),(3,3),(0.00206507808144807,0.00583603875252445,
0.00742295148565546,0.00960699434655795),(-0.0135229107749584,1.00542045039503),
 .UNSPECIFIED.)
GEOMETRIC_REPRESENTATION_ITEM()
RATIONAL_B_SPLINE_SURFACE(((1.00802943361181,0.701486699145671,1.00319274510453),
(1.00802983521136,0.701471768726875,1.00319290479263),(1.00802754903546,
0.701556762755815,1.00319199574011),(1.0080303645787,0.701452088236144,
1.00319311528506),(1.00803378849418,0.701324796030788,1.00319447673718),
(1.00803171445255,0.701401903463793,1.00319365203564)))
REPRESENTATION_ITEM('')
SURFACE()
);
#1644=(
BOUNDED_SURFACE()
B_SPLINE_SURFACE(3,2,((#44596,#44597,#44598),(#44599,#44600,#44601),(#44602,
#44603,#44604),(#44605,#44606,#44607),(#44608,#44609,#44610),(#44611,#44612,
#44613)),.UNSPECIFIED.,.F.,.F.,.F.)
B_SPLINE_SURFACE_WITH_KNOTS((4,1,1,4),(3,3),(0.00206606642132582,0.0058308811139682,
0.00741520747929493,0.00959569080576064),(-0.00535992176287023,1.01476618027226),
 .UNSPECIFIED.)
GEOMETRIC_REPRESENTATION_ITEM()
RATIONAL_B_SPLINE_SURFACE(((1.00315690508187,0.70113658592927,1.00877840586715),
(1.00315704437056,0.701123399504209,1.0087787931872),(1.00315616753589,
0.701206409222792,1.00877635497306),(1.00315726922125,0.701102112945542,
1.00877941842951),(1.00315868258643,0.700968310017838,1.00878334857402),
(1.00315783740284,0.701048323336468,1.00878099837204)))
REPRESENTATION_ITEM('')
SURFACE()
);
#1645=(
BOUNDED_SURFACE()
B_SPLINE_SURFACE(3,2,((#44614,#44615,#44616),(#44617,#44618,#44619),(#44620,
#44621,#44622),(#44623,#44624,#44625),(#44626,#44627,#44628)),
 .UNSPECIFIED.,.F.,.F.,.F.)
B_SPLINE_SURFACE_WITH_KNOTS((4,1,4),(3,3),(0.00221567299324823,0.00529019818489015,
0.00837376654817291),(-0.00338061827446617,1.03561415616917),
 .UNSPECIFIED.)
GEOMETRIC_REPRESENTATION_ITEM()
RATIONAL_B_SPLINE_SURFACE(((1.00198717354311,0.695590668589538,1.02160700592179),
(1.00198737798433,0.695559350832966,1.0216092288594),(1.00198658295342,
0.695681139303956,1.0216005843011),(1.00198751198972,0.695538822937044,
1.02161068593159),(1.00198726154498,0.695577187837766,1.02160796278695)))
REPRESENTATION_ITEM('')
SURFACE()
);
#1646=(
BOUNDED_SURFACE()
B_SPLINE_SURFACE(3,2,((#44658,#44659,#44660),(#44661,#44662,#44663),(#44664,
#44665,#44666),(#44667,#44668,#44669),(#44670,#44671,#44672)),
 .UNSPECIFIED.,.F.,.F.,.F.)
B_SPLINE_SURFACE_WITH_KNOTS((4,1,4),(3,3),(0.00212352061007265,0.00520567904197513,
0.00828782532148532),(-0.00509675325938166,1.03341354675208),
 .UNSPECIFIED.)
GEOMETRIC_REPRESENTATION_ITEM()
RATIONAL_B_SPLINE_SURFACE(((1.00300119491187,0.695690193929004,1.02022970033526),
(1.00300157279743,0.69565187776315,1.02023224749128),(1.00300017187814,
0.695793925677851,1.02022280452661),(1.0030013809653,0.695671328815938,
1.02023095443742),(1.00300106502948,0.695703363512021,1.02022882485668)))
REPRESENTATION_ITEM('')
SURFACE()
);
#1647=(
BOUNDED_SURFACE()
B_SPLINE_SURFACE(3,2,((#44719,#44720,#44721),(#44722,#44723,#44724),(#44725,
#44726,#44727),(#44728,#44729,#44730),(#44731,#44732,#44733)),
 .UNSPECIFIED.,.F.,.F.,.F.)
B_SPLINE_SURFACE_WITH_KNOTS((4,1,4),(3,3),(0.00242089776087212,0.00517364817267956,
0.00792638848906705),(0.,1.00438630646283),.UNSPECIFIED.)
GEOMETRIC_REPRESENTATION_ITEM()
RATIONAL_B_SPLINE_SURFACE(((0.999999999999999,0.705773647857135,1.00258113389988),
(1.,0.705774512519574,1.00258112631453),(1.,0.705862755339751,1.00258035219442),
(1.,0.705788773568408,1.00258100120787),(1.,0.705789544485571,1.00258099444491)))
REPRESENTATION_ITEM('')
SURFACE()
);
#1648=(
BOUNDED_SURFACE()
B_SPLINE_SURFACE(3,2,((#44748,#44749,#44750),(#44751,#44752,#44753),(#44754,
#44755,#44756),(#44757,#44758,#44759),(#44760,#44761,#44762)),
 .UNSPECIFIED.,.F.,.F.,.F.)
B_SPLINE_SURFACE_WITH_KNOTS((4,1,4),(3,3),(0.00243077395143883,0.00527113010473627,
0.00811147475653914),(0.,1.0038266298341),.UNSPECIFIED.)
GEOMETRIC_REPRESENTATION_ITEM()
RATIONAL_B_SPLINE_SURFACE(((0.999999999999999,0.705953422236314,1.00225041481417),
(1.,0.705950011646756,1.0022504409163),(1.,0.706029253698611,1.0022498344563),
(1.,0.705935850122719,1.00225054929812),(1.,0.705937868958441,1.00225053384744)))
REPRESENTATION_ITEM('')
SURFACE()
);
#1649=(
BOUNDED_SURFACE()
B_SPLINE_SURFACE(3,2,((#44763,#44764,#44765),(#44766,#44767,#44768),(#44769,
#44770,#44771),(#44772,#44773,#44774),(#44775,#44776,#44777)),
 .UNSPECIFIED.,.F.,.F.,.F.)
B_SPLINE_SURFACE_WITH_KNOTS((4,1,4),(3,3),(0.00214655059911542,0.00523053798972514,
0.00831451824855835),(-0.0445562277105792,1.00427533437828),
 .UNSPECIFIED.)
GEOMETRIC_REPRESENTATION_ITEM()
RATIONAL_B_SPLINE_SURFACE(((1.02726668218841,0.692655434185802,1.00251544567194),
(1.0272700833989,0.692617096424234,1.00251575944537),(1.02725773849294,
0.692756245725015,1.00251462058513),(1.02726782460646,0.692642557079007,
1.00251555106396),(1.02726517368982,0.692672437679016,1.00251530650774)))
REPRESENTATION_ITEM('')
SURFACE()
);
#1650=(
BOUNDED_SURFACE()
B_SPLINE_SURFACE(3,2,((#44881,#44882,#44883),(#44884,#44885,#44886),(#44887,
#44888,#44889),(#44890,#44891,#44892),(#44893,#44894,#44895)),
 .UNSPECIFIED.,.F.,.F.,.F.)
B_SPLINE_SURFACE_WITH_KNOTS((4,1,4),(3,3),(0.00211840448974134,0.00519733850462133,
0.00827626876039074),(-0.00531044220281859,1.01360741147715),
 .UNSPECIFIED.)
GEOMETRIC_REPRESENTATION_ITEM()
RATIONAL_B_SPLINE_SURFACE(((1.00312779985738,0.701476278137035,1.0080807816251),
(1.00312791614054,0.701465179830938,1.00808108204675),(1.00312679729283,
0.701571964982313,1.00807819146411),(1.00312769672486,0.701486121319756,
1.00808051517857),(1.00312758346358,0.701496931211594,1.00808022256405)))
REPRESENTATION_ITEM('')
SURFACE()
);
#1651=(
BOUNDED_SURFACE()
B_SPLINE_SURFACE(3,2,((#44909,#44910,#44911),(#44912,#44913,#44914),(#44915,
#44916,#44917),(#44918,#44919,#44920),(#44921,#44922,#44923)),
 .UNSPECIFIED.,.F.,.F.,.F.)
B_SPLINE_SURFACE_WITH_KNOTS((4,1,4),(3,3),(0.00211874843791123,0.00519509076672421,
0.00827143358138237),(-0.0125740566466983,1.00548824263856),
 .UNSPECIFIED.)
GEOMETRIC_REPRESENTATION_ITEM()
RATIONAL_B_SPLINE_SURFACE(((1.00745949944159,0.701729219975106,1.0032330898743),
(1.00745977129585,0.701718349784357,1.00323320770114),(1.00745712020765,
0.701824354503976,1.00323205866876),(1.00745927654141,0.701738132719556,
1.0032329932651),(1.00745900509947,0.701748986423287,1.00323287561697)))
REPRESENTATION_ITEM('')
SURFACE()
);
#1652=(
BOUNDED_SURFACE()
B_SPLINE_SURFACE(3,2,((#44924,#44925,#44926),(#44927,#44928,#44929),(#44930,
#44931,#44932),(#44933,#44934,#44935),(#44936,#44937,#44938)),
 .UNSPECIFIED.,.F.,.F.,.F.)
B_SPLINE_SURFACE_WITH_KNOTS((4,1,4),(3,3),(0.00215123432211629,0.00523490276681949,
0.00831856581076139),(-0.0446521768288519,1.00447160747577),
 .UNSPECIFIED.)
GEOMETRIC_REPRESENTATION_ITEM()
RATIONAL_B_SPLINE_SURFACE(((1.02732782824787,0.692565371325594,1.00263143174123),
(1.02733121531728,0.692527267220997,1.0026317578865),(1.02731901536931,
0.692664515100408,1.00263058313781),(1.02732901642887,0.692552004438952,
1.0026315461527),(1.02732639440196,0.692581501911628,1.00263129367436)))
REPRESENTATION_ITEM('')
SURFACE()
);
#1653=(
BOUNDED_SURFACE()
B_SPLINE_SURFACE(3,2,((#45042,#45043,#45044),(#45045,#45046,#45047),(#45048,
#45049,#45050),(#45051,#45052,#45053),(#45054,#45055,#45056)),
 .UNSPECIFIED.,.F.,.F.,.F.)
B_SPLINE_SURFACE_WITH_KNOTS((4,1,4),(3,3),(0.00212311714528586,0.00520198579321628,
0.00828085288284644),(-0.00537925943683262,1.01436188121935),
 .UNSPECIFIED.)
GEOMETRIC_REPRESENTATION_ITEM()
RATIONAL_B_SPLINE_SURFACE(((1.00316854084855,0.701232988150657,1.0085351498297),
(1.00316865374682,0.701222342783812,1.00853545394561),(1.00316754232714,
0.701327140403275,1.00853246009639),(1.00316844120367,0.701242383832614,
1.00853488141468),(1.00316832736094,0.701253118254473,1.00853457475466)))
REPRESENTATION_ITEM('')
SURFACE()
);
#1654=(
BOUNDED_SURFACE()
B_SPLINE_SURFACE(3,2,((#45070,#45071,#45072),(#45073,#45074,#45075),(#45076,
#45077,#45078),(#45079,#45080,#45081),(#45082,#45083,#45084)),
 .UNSPECIFIED.,.F.,.F.,.F.)
B_SPLINE_SURFACE_WITH_KNOTS((4,1,4),(3,3),(0.00212330681955807,0.00520007589671178,
0.00827684772276528),(-0.0121951366433616,1.00556207700585),
 .UNSPECIFIED.)
GEOMETRIC_REPRESENTATION_ITEM()
RATIONAL_B_SPLINE_SURFACE(((1.00723196921242,0.701820535877395,1.00327681207336),
(1.0072322169053,0.701810323315722,1.00327692430324),(1.00722971878562,
0.701913322646367,1.00327579240285),(1.00723177777283,0.701828429073946,
1.0032767253319),(1.00723151977724,0.701839066423805,1.00327660843385)))
REPRESENTATION_ITEM('')
SURFACE()
);
#1655=(
BOUNDED_SURFACE()
B_SPLINE_SURFACE(3,2,((#45085,#45086,#45087),(#45088,#45089,#45090),(#45091,
#45092,#45093),(#45094,#45095,#45096),(#45097,#45098,#45099)),
 .UNSPECIFIED.,.F.,.F.,.F.)
B_SPLINE_SURFACE_WITH_KNOTS((4,1,4),(3,3),(0.00215603338555798,0.00523933845636758,
0.0083226405745289),(-0.0447685632758762,1.00467765051002),
 .UNSPECIFIED.)
GEOMETRIC_REPRESENTATION_ITEM()
RATIONAL_B_SPLINE_SURFACE(((1.02740202841322,0.692466142220858,1.00275323936646),
(1.02740540355604,0.692428262883068,1.00275357848647),(1.02739334485071,
0.692563598125863,1.002752366879),(1.02740326485242,0.692452265623459,1.00275336359862),
(1.02740066994345,0.692481388371397,1.00275310287319)))
REPRESENTATION_ITEM('')
SURFACE()
);
#1656=(
BOUNDED_SURFACE()
B_SPLINE_SURFACE(3,2,((#45128,#45129,#45130),(#45131,#45132,#45133),(#45134,
#45135,#45136),(#45137,#45138,#45139),(#45140,#45141,#45142)),
 .UNSPECIFIED.,.F.,.F.,.F.)
B_SPLINE_SURFACE_WITH_KNOTS((4,1,4),(3,3),(0.002156044127766,0.00523919183544554,
0.00832233675413979),(-0.00548162111442793,1.0454477898263),
 .UNSPECIFIED.)
GEOMETRIC_REPRESENTATION_ITEM()
RATIONAL_B_SPLINE_SURFACE(((1.00322903191596,0.692008598862286,1.02783583820613),
(1.00322943091132,0.691970541901698,1.02783927774176),(1.00322800638677,
0.692106415848783,1.02782699764175),(1.00322918942026,0.691993575792936,
1.02783719597043),(1.00322887542929,0.69202352486771,1.02783448921434)))
REPRESENTATION_ITEM('')
SURFACE()
);
#1657=(
BOUNDED_SURFACE()
B_SPLINE_SURFACE(3,2,((#45190,#45191,#45192),(#45193,#45194,#45195),(#45196,
#45197,#45198),(#45199,#45200,#45201),(#45202,#45203,#45204)),
 .UNSPECIFIED.,.F.,.F.,.F.)
B_SPLINE_SURFACE_WITH_KNOTS((4,1,4),(3,3),(0.00212802408085649,0.00520645763078059,
0.00828489231196136),(-0.00544652756431799,1.01484739119941),
 .UNSPECIFIED.)
GEOMETRIC_REPRESENTATION_ITEM()
RATIONAL_B_SPLINE_SURFACE(((1.00320837001835,0.701069722901491,1.00882788477518),
(1.00320847966809,0.701059506614525,1.00882818647832),(1.00320737445807,
0.701162481251729,1.00882514547411),(1.0032082761041,0.701078473080572,
1.00882762636853),(1.00320816004395,0.701089286637446,1.00882730702706)))
REPRESENTATION_ITEM('')
SURFACE()
);
#1658=(
BOUNDED_SURFACE()
B_SPLINE_SURFACE(3,2,((#45218,#45219,#45220),(#45221,#45222,#45223),(#45224,
#45225,#45226),(#45227,#45228,#45229),(#45230,#45231,#45232)),
 .UNSPECIFIED.,.F.,.F.,.F.)
B_SPLINE_SURFACE_WITH_KNOTS((4,1,4),(3,3),(0.00212780620908921,0.00520535309141684,
0.00828290460668537),(-0.0123335526006055,1.00564508813243),
 .UNSPECIFIED.)
GEOMETRIC_REPRESENTATION_ITEM()
RATIONAL_B_SPLINE_SURFACE(((1.00731501770778,0.701756056773149,1.00332597532949),
(1.00731524864014,0.701746641323926,1.00332608032928),(1.00731281032856,
0.701846054844198,1.00332497168341),(1.00731484685567,0.701763022662945,
1.00332589764685),(1.00731459376117,0.701773341694953,1.00332578257042)))
REPRESENTATION_ITEM('')
SURFACE()
);
#1659=(
BOUNDED_SURFACE()
B_SPLINE_SURFACE(3,2,((#45233,#45234,#45235),(#45236,#45237,#45238),(#45239,
#45240,#45241),(#45242,#45243,#45244),(#45245,#45246,#45247)),
 .UNSPECIFIED.,.F.,.F.,.F.)
B_SPLINE_SURFACE_WITH_KNOTS((4,1,4),(3,3),(0.00216103530262931,0.00524384440588618,
0.00832665287687961),(-0.0446064778924999,1.0048995043461),
 .UNSPECIFIED.)
GEOMETRIC_REPRESENTATION_ITEM()
RATIONAL_B_SPLINE_SURFACE(((1.02729850625157,0.692444146963455,1.00288445000016),
(1.02730185345113,0.692406436078964,1.00288480367628),(1.02728998621801,
0.692540137057693,1.00288354974538),(1.02729979876591,0.692429584981676,
1.00288458657148),(1.02729723696384,0.692458447264937,1.00288431588304)))
REPRESENTATION_ITEM('')
SURFACE()
);
#1660=(
BOUNDED_SURFACE()
B_SPLINE_SURFACE(3,2,((#45276,#45277,#45278),(#45279,#45280,#45281),(#45282,
#45283,#45284),(#45285,#45286,#45287),(#45288,#45289,#45290)),
 .UNSPECIFIED.,.F.,.F.,.F.)
B_SPLINE_SURFACE_WITH_KNOTS((4,1,4),(3,3),(0.00216084865593138,0.0052451443109893,
0.00832943934876088),(-0.00568511307436906,1.04556686179785),
 .UNSPECIFIED.)
GEOMETRIC_REPRESENTATION_ITEM()
RATIONAL_B_SPLINE_SURFACE(((1.00334957403885,0.691908816802213,1.02791189889522),
(1.00334998689027,0.691870843054131,1.02791533917354),(1.00334852263475,
0.692005524123632,1.02790313757674),(1.00334973592382,0.691893926750258,
1.02791324787776),(1.00334941299497,0.691923629491969,1.02791055692142)))
REPRESENTATION_ITEM('')
SURFACE()
);
#1661=(
BOUNDED_SURFACE()
B_SPLINE_SURFACE(3,2,((#45333,#45334,#45335),(#45336,#45337,#45338),(#45339,
#45340,#45341),(#45342,#45343,#45344),(#45345,#45346,#45347)),
 .UNSPECIFIED.,.F.,.F.,.F.)
B_SPLINE_SURFACE_WITH_KNOTS((4,1,4),(3,3),(0.00213302336063595,0.00521101927613581,
0.00828901632118316),(-0.00549073681840203,1.0147633501061),
 .UNSPECIFIED.)
GEOMETRIC_REPRESENTATION_ITEM()
RATIONAL_B_SPLINE_SURFACE(((1.00323454601582,0.701082056419879,1.00877716625763),
(1.00323465179662,0.701072280773333,1.00877745330121),(1.0032335573809,
0.7011734203137,1.0087744835278),(1.00323445964151,0.701090038631704,1.00877693187492),
(1.0032343417967,0.701100929163706,1.00877661209481)))
REPRESENTATION_ITEM('')
SURFACE()
);
#1662=(
BOUNDED_SURFACE()
B_SPLINE_SURFACE(3,2,((#45362,#45363,#45364),(#45365,#45366,#45367),(#45368,
#45369,#45370),(#45371,#45372,#45373),(#45374,#45375,#45376)),
 .UNSPECIFIED.,.F.,.F.,.F.)
B_SPLINE_SURFACE_WITH_KNOTS((4,1,4),(3,3),(0.00213312433381201,0.00521163967845316,
0.00829016000657247),(-0.0156178445535448,1.00571793255727),
 .UNSPECIFIED.)
GEOMETRIC_REPRESENTATION_ITEM()
RATIONAL_B_SPLINE_SURFACE(((1.00929301133279,0.700760075002523,1.00336914940697),
(1.00929331665074,0.70075024360155,1.00336926009895),(1.00929015613772,
0.700852013807781,1.00336811426578),(1.00929275637582,0.70076828475314,
1.0033690569732),(1.00929243233675,0.700778718984092,1.00336893949394)))
REPRESENTATION_ITEM('')
SURFACE()
);
#1663=(
BOUNDED_SURFACE()
B_SPLINE_SURFACE(3,2,((#45377,#45378,#45379),(#45380,#45381,#45382),(#45383,
#45384,#45385),(#45386,#45387,#45388),(#45389,#45390,#45391),(#45392,#45393,
#45394)),.UNSPECIFIED.,.F.,.F.,.F.)
B_SPLINE_SURFACE_WITH_KNOTS((4,1,1,4),(3,3),(0.00208139341848436,0.00585739462970524,
0.00744642968342663,0.0096333934474643),(-0.0100479807687911,1.06113579455401),
 .UNSPECIFIED.)
GEOMETRIC_REPRESENTATION_ITEM()
RATIONAL_B_SPLINE_SURFACE(((1.00594551440041,0.685876484175346,1.0380045120459),
(1.00594626072007,0.685837053347266,1.03800928261959),(1.00594424103948,
0.685943760542502,1.03799637255497),(1.00594637770504,0.685830872598689,
1.03801003040293),(1.00594862274388,0.68571225889319,1.03802438098725),
(1.0059477826065,0.685756646458221,1.03801901071834)))
REPRESENTATION_ITEM('')
SURFACE()
);
#1664=(
BOUNDED_SURFACE()
B_SPLINE_SURFACE(3,2,((#45422,#45423,#45424),(#45425,#45426,#45427),(#45428,
#45429,#45430),(#45431,#45432,#45433),(#45434,#45435,#45436),(#45437,#45438,
#45439)),.UNSPECIFIED.,.F.,.F.,.F.)
B_SPLINE_SURFACE_WITH_KNOTS((4,1,1,4),(3,3),(0.00208246989021945,0.00585173909416552,
0.00743794117493988,0.00962100597940954),(-0.0634120194467482,1.01004449590126),
 .UNSPECIFIED.)
GEOMETRIC_REPRESENTATION_ITEM()
RATIONAL_B_SPLINE_SURFACE(((1.03950397758292,0.685198194337763,1.00594341874322),
(1.03950901710132,0.68515803510341,1.00594417694454),(1.03949563649155,
0.685264663356425,1.00594216381645),(1.03950982841265,0.685151569874148,
1.00594429900726),(1.0395253903989,0.685027558529697,1.00594664032594),
(1.03951949311786,0.68507455315746,1.00594575307324)))
REPRESENTATION_ITEM('')
SURFACE()
);
#1665=(
BOUNDED_SURFACE()
B_SPLINE_SURFACE(3,2,((#45478,#45479,#45480),(#45481,#45482,#45483),(#45484,
#45485,#45486),(#45487,#45488,#45489),(#45490,#45491,#45492),(#45493,#45494,
#45495)),.UNSPECIFIED.,.F.,.F.,.F.)
B_SPLINE_SURFACE_WITH_KNOTS((4,1,1,4),(3,3),(0.00206902137639543,0.0058401154462197,
0.00742708429774716,0.00961120439636198),(-0.0133376601097449,1.00544905730155),
 .UNSPECIFIED.)
GEOMETRIC_REPRESENTATION_ITEM()
RATIONAL_B_SPLINE_SURFACE(((1.00791799171496,0.701532910309794,1.00320968682838),
(1.00791837853318,0.701518329275477,1.00320984363144),(1.0079161281519,
0.701603156941006,1.00320893140275),(1.00791891490684,0.701498110779302,
1.00321006105923),(1.00792225352701,0.701372262169953,1.00321141442326),
(1.00792022918322,0.70144856939801,1.00321059382256)))
REPRESENTATION_ITEM('')
SURFACE()
);
#1666=(
BOUNDED_SURFACE()
B_SPLINE_SURFACE(3,2,((#45510,#45511,#45512),(#45513,#45514,#45515),(#45516,
#45517,#45518),(#45519,#45520,#45521),(#45522,#45523,#45524),(#45525,#45526,
#45527)),.UNSPECIFIED.,.F.,.F.,.F.)
B_SPLINE_SURFACE_WITH_KNOTS((4,1,1,4),(3,3),(0.00206993025455239,0.00583529331732963,
0.00741985043665655,0.00960064723499827),(-0.00538361942335849,1.01460879274893),
 .UNSPECIFIED.)
GEOMETRIC_REPRESENTATION_ITEM()
RATIONAL_B_SPLINE_SURFACE(((1.00317093655876,0.701176112786129,1.00868349075652),
(1.00317107609581,0.701162963042384,1.00868387287349),(1.00317019729362,
0.70124577992633,1.00868146630669),(1.0031713020113,0.701141673135268,1.00868449153458),
(1.00317270302626,0.701009643771633,1.00868832816146),(1.00317186374986,
0.701088735810024,1.00868602983454)))
REPRESENTATION_ITEM('')
SURFACE()
);
#1667=(
BOUNDED_SURFACE()
B_SPLINE_SURFACE(3,2,((#45528,#45529,#45530),(#45531,#45532,#45533),(#45534,
#45535,#45536),(#45537,#45538,#45539),(#45540,#45541,#45542),(#45543,#45544,
#45545)),.UNSPECIFIED.,.F.,.F.,.F.)
B_SPLINE_SURFACE_WITH_KNOTS((4,1,1,4),(3,3),(0.00211869188141098,0.00569878884162654,
0.00720538255197427,0.00927888394959123),(-0.00871872596836085,1.05558447453005),
 .UNSPECIFIED.)
GEOMETRIC_REPRESENTATION_ITEM()
RATIONAL_B_SPLINE_SURFACE(((1.00515221228299,0.687966416849009,1.03437297609083),
(1.00515279666831,0.6879310247041,1.03437687481654),(1.00515125599611,0.68802433247961,
1.03436659622439),(1.00515259663208,0.687943139504264,1.03437554027513),
(1.00515441105761,0.687833252397824,1.03438764521218),(1.00515357264877,
0.687884028976962,1.03438205176893)))
REPRESENTATION_ITEM('')
SURFACE()
);
#1668=(
BOUNDED_SURFACE()
B_SPLINE_SURFACE(3,2,((#45575,#45576,#45577),(#45578,#45579,#45580),(#45581,
#45582,#45583),(#45584,#45585,#45586),(#45587,#45588,#45589),(#45590,#45591,
#45592)),.UNSPECIFIED.,.F.,.F.,.F.)
B_SPLINE_SURFACE_WITH_KNOTS((4,1,1,4),(3,3),(0.00209859031566758,0.00417178913822665,
0.00567815886986545,0.00925772626818232),(-0.00545725414786132,1.05802705461411),
 .UNSPECIFIED.)
GEOMETRIC_REPRESENTATION_ITEM()
RATIONAL_B_SPLINE_SURFACE(((1.00321534304372,0.688219339890755,1.03597632707853),
(1.00321587624839,0.688167636883823,1.03598229308132),(1.00321470970128,
0.688280752909962,1.03596924063877),(1.00321386482928,0.68836267721651,
1.03595978740442),(1.00321482739532,0.688269340527273,1.03597055751203),
(1.00321445716244,0.688305240725027,1.03596641499319)))
REPRESENTATION_ITEM('')
SURFACE()
);
#1669=(
BOUNDED_SURFACE()
B_SPLINE_SURFACE(3,2,((#45607,#45608,#45609),(#45610,#45611,#45612),(#45613,
#45614,#45615),(#45616,#45617,#45618),(#45619,#45620,#45621),(#45622,#45623,
#45624)),.UNSPECIFIED.,.F.,.F.,.F.)
B_SPLINE_SURFACE_WITH_KNOTS((4,1,1,4),(3,3),(0.00606711198524399,0.00688009229885085,
0.00722221478938814,0.00769307340420083),(-0.00991670930616596,1.00217563956271),
 .UNSPECIFIED.)
GEOMETRIC_REPRESENTATION_ITEM()
RATIONAL_B_SPLINE_SURFACE(((1.00594634748185,0.699526756281591,1.00129457713788),
(1.00594486311264,0.699601762532408,1.00129425397641),(1.00595105902295,
0.699288678698464,1.00129560288578),(1.00593196169786,0.700253680362731,
1.00129144521411),(1.00590427588377,0.701652664594436,1.00128541774564),
(1.00591770573521,0.700974044477186,1.00128834155369)))
REPRESENTATION_ITEM('')
SURFACE()
);
#1670=(
BOUNDED_SURFACE()
B_SPLINE_SURFACE(3,2,((#45647,#45648,#45649),(#45650,#45651,#45652),(#45653,
#45654,#45655),(#45656,#45657,#45658),(#45659,#45660,#45661),(#45662,#45663,
#45664)),.UNSPECIFIED.,.F.,.F.,.F.)
B_SPLINE_SURFACE_WITH_KNOTS((4,1,1,4),(3,3),(0.00586170810752336,0.00620302448742682,
0.00654434086733029,0.00722697362713722),(0.,1.),.UNSPECIFIED.)
GEOMETRIC_REPRESENTATION_ITEM()
RATIONAL_B_SPLINE_SURFACE(((1.,0.703291914743876,1.),(1.,0.703291156633914,
1.),(1.,0.702986672263162,1.),(1.,0.7036715161092,1.),(1.,0.704097894613167,
1.),(1.,0.704100348801905,1.)))
REPRESENTATION_ITEM('')
SURFACE()
);
#1671=(
BOUNDED_SURFACE()
B_SPLINE_SURFACE(3,2,((#45687,#45688,#45689),(#45690,#45691,#45692),(#45693,
#45694,#45695),(#45696,#45697,#45698),(#45699,#45700,#45701),(#45702,#45703,
#45704)),.UNSPECIFIED.,.F.,.F.,.F.)
B_SPLINE_SURFACE_WITH_KNOTS((4,1,1,4),(3,3),(0.00207336170120452,0.0058428956621075,
0.00742920796878192,0.00961242447694922),(-0.0132972947360473,1.00601408397336),
 .UNSPECIFIED.)
GEOMETRIC_REPRESENTATION_ITEM()
RATIONAL_B_SPLINE_SURFACE(((1.00789371657458,0.701374858896592,1.00354449933517),
(1.00789409196049,0.70136065776996,1.00354466789394),(1.00789185890845,
0.701445135781318,1.00354366519117),(1.00789463032497,0.701340291043177,
1.00354490963463),(1.00789794199947,0.701215007945169,1.00354639666903),
(1.00789593869161,0.701290794564665,1.00354549712782)))
REPRESENTATION_ITEM('')
SURFACE()
);
#1672=(
BOUNDED_SURFACE()
B_SPLINE_SURFACE(3,2,((#45718,#45719,#45720),(#45721,#45722,#45723),(#45724,
#45725,#45726),(#45727,#45728,#45729),(#45730,#45731,#45732),(#45733,#45734,
#45735)),.UNSPECIFIED.,.F.,.F.,.F.)
B_SPLINE_SURFACE_WITH_KNOTS((4,1,1,4),(3,3),(0.00207669134204795,0.00582595496795364,
0.00740373706151585,0.00957521363909962),(-0.00543600822727895,1.01524353115776),
 .UNSPECIFIED.)
GEOMETRIC_REPRESENTATION_ITEM()
RATIONAL_B_SPLINE_SURFACE(((1.00320196063785,0.70097233288763,1.00906644982378),
(1.00320209762572,0.700959539736781,1.00906683770916),(1.00320123008922,
0.701040558039555,1.00906438125293),(1.00320229942714,0.700940693718888,
1.00906740911607),(1.00320373776939,0.700806368480488,1.00907148182629),
(1.00320290663572,0.700883987161842,1.00906912844579)))
REPRESENTATION_ITEM('')
SURFACE()
);
#1673=(
BOUNDED_SURFACE()
B_SPLINE_SURFACE(3,2,((#45736,#45737,#45738),(#45739,#45740,#45741),(#45742,
#45743,#45744),(#45745,#45746,#45747),(#45748,#45749,#45750)),
 .UNSPECIFIED.,.F.,.F.,.F.)
B_SPLINE_SURFACE_WITH_KNOTS((4,1,4),(3,3),(0.00217622474172813,0.00539216358099794,
0.00861633928504423),(-0.00372387570917386,1.05641859002687),
 .UNSPECIFIED.)
GEOMETRIC_REPRESENTATION_ITEM()
RATIONAL_B_SPLINE_SURFACE(((1.00218965794407,0.689348696115286,1.03491605013112),
(1.00218988124539,0.689317015895015,1.03491961086995),(1.00218900484019,
0.689441353313379,1.03490563580698),(1.00219017995013,0.689274638034762,
1.03492437398368),(1.00218991474363,0.689312263429291,1.0349201450294)))
REPRESENTATION_ITEM('')
SURFACE()
);
#1674=(
BOUNDED_SURFACE()
B_SPLINE_SURFACE(3,2,((#45780,#45781,#45782),(#45783,#45784,#45785),(#45786,
#45787,#45788),(#45789,#45790,#45791),(#45792,#45793,#45794)),
 .UNSPECIFIED.,.F.,.F.,.F.)
B_SPLINE_SURFACE_WITH_KNOTS((4,1,4),(3,3),(0.00212311658518805,0.0053456007449197,
0.00856807426106279),(-0.00599908652418573,1.05456025857004),
 .UNSPECIFIED.)
GEOMETRIC_REPRESENTATION_ITEM()
RATIONAL_B_SPLINE_SURFACE(((1.00353590342769,0.689121530506963,1.03371052402231),
(1.00353634139136,0.689083024513225,1.03371469947142),(1.0035344304439,
0.689251036007775,1.03369648091954),(1.0035358507774,0.689126159547288,
1.03371002206611),(1.00353548205318,0.689158577972859,1.03370650673063)))
REPRESENTATION_ITEM('')
SURFACE()
);
#1675=(
BOUNDED_SURFACE()
B_SPLINE_SURFACE(3,2,((#45809,#45810,#45811),(#45812,#45813,#45814),(#45815,
#45816,#45817),(#45818,#45819,#45820),(#45821,#45822,#45823)),
 .UNSPECIFIED.,.F.,.F.,.F.)
B_SPLINE_SURFACE_WITH_KNOTS((4,1,4),(3,3),(0.00576991625672856,0.00655606720393187,
0.00734221533127076),(-0.057191197943434,1.),.UNSPECIFIED.)
GEOMETRIC_REPRESENTATION_ITEM()
RATIONAL_B_SPLINE_SURFACE(((1.03589548298643,0.686180004290742,1.),(1.03587833722817,
0.686329902866713,1.),(1.03597689454535,0.685468255264237,1.),(1.03568868718054,
0.687987938145351,1.),(1.03574452383035,0.687499780423329,1.)))
REPRESENTATION_ITEM('')
SURFACE()
);
#1676=(
BOUNDED_SURFACE()
B_SPLINE_SURFACE(3,2,((#45838,#45839,#45840),(#45841,#45842,#45843),(#45844,
#45845,#45846),(#45847,#45848,#45849),(#45850,#45851,#45852)),
 .UNSPECIFIED.,.F.,.F.,.F.)
B_SPLINE_SURFACE_WITH_KNOTS((4,1,4),(3,3),(0.00466657533706555,0.00544764278228739,
0.00622871275121123),(0.,1.07164194621731),.UNSPECIFIED.)
GEOMETRIC_REPRESENTATION_ITEM()
RATIONAL_B_SPLINE_SURFACE(((1.,0.682037840892741,1.0455588558038),(1.,0.682033056803698,
1.0455595412867),(1.,0.682024198389298,1.0455608105548),(1.,0.682718710372074,
1.04546129817456),(1.,0.682583619049144,1.04548065458515)))
REPRESENTATION_ITEM('')
SURFACE()
);
#1677=(
BOUNDED_SURFACE()
B_SPLINE_SURFACE(3,2,((#45857,#45858,#45859),(#45860,#45861,#45862),(#45863,
#45864,#45865),(#45866,#45867,#45868),(#45869,#45870,#45871),(#45872,#45873,
#45874)),.UNSPECIFIED.,.F.,.F.,.F.)
B_SPLINE_SURFACE_WITH_KNOTS((4,1,1,4),(3,3),(0.00204566630298345,0.00400993138179308,
0.00543715219179253,0.00882864065979569),(-0.00571744098087493,1.01125109042059),
 .UNSPECIFIED.)
GEOMETRIC_REPRESENTATION_ITEM()
RATIONAL_B_SPLINE_SURFACE(((1.00336919435212,0.702024299561637,1.00666656334336),
(1.00336959338059,0.701989008992314,1.0066673528937),(1.0033687757138,0.702061324451092,
1.00666573499135),(1.00336801089579,0.702128965897631,1.00666422165993),
(1.00336883090118,0.70205644361065,1.00666584418962),(1.0033686873612,0.702069138463297,
1.00666556016969)))
REPRESENTATION_ITEM('')
SURFACE()
);
#1678=(
BOUNDED_SURFACE()
B_SPLINE_SURFACE(3,2,((#45883,#45884,#45885),(#45886,#45887,#45888),(#45889,
#45890,#45891),(#45892,#45893,#45894),(#45895,#45896,#45897)),
 .UNSPECIFIED.,.F.,.F.,.F.)
B_SPLINE_SURFACE_WITH_KNOTS((4,1,4),(3,3),(0.0021959381419612,0.00532325757153969,
0.00845897824613069),(-0.00319606621206401,1.04760710946989),
 .UNSPECIFIED.)
GEOMETRIC_REPRESENTATION_ITEM()
RATIONAL_B_SPLINE_SURFACE(((1.00187832317392,0.692116891994823,1.0292172259266),
(1.00187850752375,0.692086674512343,1.02922009347922),(1.00187779088182,
0.692204142021837,1.02920894614871),(1.00187868898111,0.692056931145811,
1.02922291603959),(1.00187845708403,0.692094942278776,1.02921930889184)))
REPRESENTATION_ITEM('')
SURFACE()
);
#1679=(
BOUNDED_SURFACE()
B_SPLINE_SURFACE(3,2,((#45923,#45924,#45925),(#45926,#45927,#45928),(#45929,
#45930,#45931),(#45932,#45933,#45934),(#45935,#45936,#45937)),
 .UNSPECIFIED.,.F.,.F.,.F.)
B_SPLINE_SURFACE_WITH_KNOTS((4,1,4),(3,3),(0.00211126073213577,0.005246147458561,
0.00837261176721595),(-0.00426982890845349,1.04600228977135),
 .UNSPECIFIED.)
GEOMETRIC_REPRESENTATION_ITEM()
RATIONAL_B_SPLINE_SURFACE(((1.00251223791948,0.692224438834479,1.02819109612041),
(1.00251254913415,0.692186311764292,1.02819458841816),(1.0025113457616,
0.692333737555445,1.02818108476429),(1.00251230256491,0.692216519088568,
1.02819182153966),(1.00251205570066,0.692246762556132,1.02818905135057)))
REPRESENTATION_ITEM('')
SURFACE()
);
#1680=(
BOUNDED_SURFACE()
B_SPLINE_SURFACE(3,2,((#45976,#45977,#45978),(#45979,#45980,#45981),(#45982,
#45983,#45984),(#45985,#45986,#45987),(#45988,#45989,#45990)),
 .UNSPECIFIED.,.F.,.F.,.F.)
B_SPLINE_SURFACE_WITH_KNOTS((4,1,4),(3,3),(0.0020676411228087,0.00523242399231858,
0.00839719713565984),(-0.00487431079868958,1.01404338604498),
 .UNSPECIFIED.)
GEOMETRIC_REPRESENTATION_ITEM()
RATIONAL_B_SPLINE_SURFACE(((1.0028697300377,0.701473052287329,1.00834342667499),
(1.00286987939032,0.701457515709757,1.00834386090144),(1.00286870618288,
0.701579559954994,1.00834044992893),(1.00286959084033,0.701487532452169,
1.00834302197386),(1.00286947935389,0.70149912995714,1.0083426978392)))
REPRESENTATION_ITEM('')
SURFACE()
);
#1681=(
BOUNDED_SURFACE()
B_SPLINE_SURFACE(3,2,((#46006,#46007,#46008),(#46009,#46010,#46011),(#46012,
#46013,#46014),(#46015,#46016,#46017),(#46018,#46019,#46020)),
 .UNSPECIFIED.,.F.,.F.,.F.)
B_SPLINE_SURFACE_WITH_KNOTS((4,1,4),(3,3),(0.00217004352235611,0.00533300005217428,
0.00849594930601141),(-0.00629182520020718,1.01422385876462),
 .UNSPECIFIED.)
GEOMETRIC_REPRESENTATION_ITEM()
RATIONAL_B_SPLINE_SURFACE(((1.00370918483522,0.701018900626283,1.00845140932802),
(1.00370932633503,0.701007494948168,1.00845173173654),(1.0037081879283,
0.701099256915289,1.00844913786707),(1.00370970938845,0.700976618694825,
1.00845260452702),(1.00370951547823,0.700992248945929,1.00845216270093)))
REPRESENTATION_ITEM('')
SURFACE()
);
#1682=(
BOUNDED_SURFACE()
B_SPLINE_SURFACE(3,2,((#46021,#46022,#46023),(#46024,#46025,#46026),(#46027,
#46028,#46029),(#46030,#46031,#46032),(#46033,#46034,#46035)),
 .UNSPECIFIED.,.F.,.F.,.F.)
B_SPLINE_SURFACE_WITH_KNOTS((4,1,4),(3,3),(0.00658134838002377,0.00749225635020362,
0.00840316205258835),(-0.00373012175731709,1.03258272302577),
 .UNSPECIFIED.)
GEOMETRIC_REPRESENTATION_ITEM()
RATIONAL_B_SPLINE_SURFACE(((1.00221701425539,0.693103976914044,1.01992235850238),
(1.00221628705211,0.693204641938182,1.0199158237657),(1.00222066280505,
0.692598916841125,1.01995514481136),(1.00220180759727,0.69520899851706,
1.0197857096315),(1.00220551783436,0.694695399200248,1.01981905027116)))
REPRESENTATION_ITEM('')
SURFACE()
);
#1683=(
BOUNDED_SURFACE()
B_SPLINE_SURFACE(3,2,((#46066,#46067,#46068),(#46069,#46070,#46071),(#46072,
#46073,#46074),(#46075,#46076,#46077),(#46078,#46079,#46080)),
 .UNSPECIFIED.,.F.,.F.,.F.)
B_SPLINE_SURFACE_WITH_KNOTS((4,1,4),(3,3),(0.00227075980744937,0.00518182494025859,
0.00809289088251492),(-0.00521186425511147,1.0082792049588),
 .UNSPECIFIED.)
GEOMETRIC_REPRESENTATION_ITEM()
RATIONAL_B_SPLINE_SURFACE(((1.00306922824857,0.703103283428404,1.0048904399369),
(1.00306931230498,0.703095152370975,1.00489057387051),(1.0030686191024,
0.703162208175352,1.00488946933696),(1.0030692514443,0.703101039627365,
1.00489047689647),(1.00306931856182,0.703094547125393,1.00489058384003)))
REPRESENTATION_ITEM('')
SURFACE()
);
#1684=(
BOUNDED_SURFACE()
B_SPLINE_SURFACE(3,2,((#46124,#46125,#46126),(#46127,#46128,#46129),(#46130,
#46131,#46132),(#46133,#46134,#46135),(#46136,#46137,#46138)),
 .UNSPECIFIED.,.F.,.F.,.F.)
B_SPLINE_SURFACE_WITH_KNOTS((4,1,4),(3,3),(0.0034568776936703,0.00436551562806062,
0.00527415564536653),(-0.0036707976681412,1.03238825219618),
 .UNSPECIFIED.)
GEOMETRIC_REPRESENTATION_ITEM()
RATIONAL_B_SPLINE_SURFACE(((1.00217038145229,0.694762063835327,1.01969767194357),
(1.00216674940448,0.695272867490565,1.01966470866596),(1.00218520712167,
0.692677012510241,1.0198322248681),(1.00218093167134,0.693278302957743,
1.01979342227977),(1.00218164267322,0.693178309130949,1.01979987510022)))
REPRESENTATION_ITEM('')
SURFACE()
);
#1685=(
BOUNDED_SURFACE()
B_SPLINE_SURFACE(3,2,((#46187,#46188,#46189),(#46190,#46191,#46192),(#46193,
#46194,#46195),(#46196,#46197,#46198)),.UNSPECIFIED.,.F.,.F.,.F.)
B_SPLINE_SURFACE_WITH_KNOTS((4,4),(3,3),(0.00370520097294563,0.00941954636052541),
(-0.0101428155788133,1.05214450432649),.UNSPECIFIED.)
GEOMETRIC_REPRESENTATION_ITEM()
RATIONAL_B_SPLINE_SURFACE(((1.00600421848268,0.688427284912467,1.03215134260149),
(1.00599942234611,0.688676167476638,1.03212566028657),(1.00600312517364,
0.688484019234624,1.03214548815872),(1.00600227584133,0.688528093042654,
1.03214094016067)))
REPRESENTATION_ITEM('')
SURFACE()
);
#1686=(
BOUNDED_SURFACE()
B_SPLINE_SURFACE(3,2,((#46229,#46230,#46231),(#46232,#46233,#46234),(#46235,
#46236,#46237),(#46238,#46239,#46240),(#46241,#46242,#46243)),
 .UNSPECIFIED.,.F.,.F.,.F.)
B_SPLINE_SURFACE_WITH_KNOTS((4,1,4),(3,3),(0.00223723210298208,0.00504001293429967,
0.00784280154769125),(-0.0115719706077613,1.02620831455806),
 .UNSPECIFIED.)
GEOMETRIC_REPRESENTATION_ITEM()
RATIONAL_B_SPLINE_SURFACE(((1.00685773465935,0.695837442077627,1.01575618930365),
(1.00685815020969,0.695819011085351,1.01575714406352),(1.00685675136247,
0.695881054452243,1.01575393010109),(1.00685696168086,0.695871726156367,
1.01575441332426),(1.00685966802559,0.695751691075158,1.01576063136594)))
REPRESENTATION_ITEM('')
SURFACE()
);
#1687=(
BOUNDED_SURFACE()
B_SPLINE_SURFACE(3,2,((#46270,#46271,#46272),(#46273,#46274,#46275),(#46276,
#46277,#46278),(#46279,#46280,#46281),(#46282,#46283,#46284),(#46285,#46286,
#46287)),.UNSPECIFIED.,.F.,.F.,.F.)
B_SPLINE_SURFACE_WITH_KNOTS((4,1,1,4),(3,3),(0.0022677946226757,0.00391401491016076,
0.00511014847692749,0.00795245641742074),(-0.023127469090911,1.01566061070927),
 .UNSPECIFIED.)
GEOMETRIC_REPRESENTATION_ITEM()
RATIONAL_B_SPLINE_SURFACE(((1.01388126111192,0.695090628112123,1.0093310039554),
(1.01386984071289,0.695341483323618,1.00932332714653),(1.01389028228548,
0.694892473179237,1.00933706800142),(1.01393022057232,0.694015207212054,
1.00936391457605),(1.0139354303761,0.693900771067822,1.00936741661375),
(1.01394154050068,0.693766558892522,1.0093715238484)))
REPRESENTATION_ITEM('')
SURFACE()
);
#1688=(
BOUNDED_SURFACE()
B_SPLINE_SURFACE(3,2,((#46297,#46298,#46299),(#46300,#46301,#46302),(#46303,
#46304,#46305),(#46306,#46307,#46308),(#46309,#46310,#46311),(#46312,#46313,
#46314),(#46315,#46316,#46317),(#46318,#46319,#46320),(#46321,#46322,#46323),
(#46324,#46325,#46326),(#46327,#46328,#46329),(#46330,#46331,#46332),(#46333,
#46334,#46335),(#46336,#46337,#46338),(#46339,#46340,#46341),(#46342,#46343,
#46344),(#46345,#46346,#46347),(#46348,#46349,#46350),(#46351,#46352,#46353),
(#46354,#46355,#46356)),.UNSPECIFIED.,.F.,.F.,.F.)
B_SPLINE_SURFACE_WITH_KNOTS((4,1,1,1,1,1,1,1,1,1,1,1,1,1,1,1,1,4),(3,3),
(0.00261725296323532,0.00654848262222231,0.00767005292085768,0.00879162321949305,
0.0110347638167638,0.0121563341153991,0.0132779044140345,0.0143994747126699,
0.0155210450113053,0.0160818301606229,0.0166426153099406,0.0172034004592583,
0.017764185608576,0.0183249707578937,0.0188857559072114,0.0200073262058467,
0.0211288965044821,0.0239385696629217),(-0.0168546607502698,1.01516107000004),
 .UNSPECIFIED.)
GEOMETRIC_REPRESENTATION_ITEM()
RATIONAL_B_SPLINE_SURFACE(((1.01001782862897,0.698236966842449,1.00899620838692),
(1.01007197783254,0.69660585210528,1.00904483544348),(1.0100059927647,0.698593493833998,
1.00898557954655),(1.01008063671936,0.696345023931289,1.00905261129522),
(1.0100833239308,0.696264078138843,1.00905502446428),(1.01010437659876,
0.695629917067113,1.0090739301768),(1.01011267293465,0.695380009869258,
1.00908138045063),(1.0101193585501,0.695178621757002,1.00908738426563),
(1.01012286714301,0.695072933820154,1.00909053505151),(1.01011222145419,
0.695393609633978,1.00908097501224),(1.01009640880339,0.695869927770989,
1.00906677493884),(1.01005939440848,0.696984897540488,1.00903353527961),
(1.01003148595116,0.697825572804787,1.00900847293256),(1.0100535225878,
0.697161772039365,1.00902826226842),(1.01007027801628,0.696657054988678,
1.00904330897483),(1.01008761546103,0.696134806095195,1.00905887834337),
(1.01009729394663,0.695843264956113,1.009067569815),(1.01010211520435,0.695698036143758,
1.00907189939986),(1.01010122883875,0.695724735779169,1.009071103426),(1.01010042823197,
0.695748852135982,1.00907038446527)))
REPRESENTATION_ITEM('')
SURFACE()
);
#1689=(
BOUNDED_SURFACE()
B_SPLINE_SURFACE(3,2,((#46395,#46396,#46397),(#46398,#46399,#46400),(#46401,
#46402,#46403),(#46404,#46405,#46406),(#46407,#46408,#46409),(#46410,#46411,
#46412),(#46413,#46414,#46415),(#46416,#46417,#46418),(#46419,#46420,#46421),
(#46422,#46423,#46424),(#46425,#46426,#46427),(#46428,#46429,#46430),(#46431,
#46432,#46433),(#46434,#46435,#46436),(#46437,#46438,#46439),(#46440,#46441,
#46442),(#46443,#46444,#46445),(#46446,#46447,#46448),(#46449,#46450,#46451)),
 .UNSPECIFIED.,.F.,.F.,.F.)
B_SPLINE_SURFACE_WITH_KNOTS((4,1,1,1,1,1,1,1,1,1,1,1,1,1,1,1,4),(3,3),(0.00189550760743663,
0.00466304228864453,0.00576778402465584,0.00687252576066714,0.0074248966286728,
0.00797726749667845,0.0085296383646841,0.00908200923268976,0.00963438010069541,
0.0101867509687011,0.0112914927047124,0.0123962344407237,0.0146057179127463,
0.0168152013847689,0.0179199431207802,0.0190246848567915,0.0228969445771743),
(-0.018513716758316,1.01985338840949),.UNSPECIFIED.)
GEOMETRIC_REPRESENTATION_ITEM()
RATIONAL_B_SPLINE_SURFACE(((1.01111188940034,0.693834894151823,1.01193163048407),
(1.01111283607111,0.693808810598902,1.01193264699219),(1.01111479004412,
0.693754972918195,1.01193474511278),(1.0111066333323,0.69397971422442,1.01192598666784),
(1.01109405899069,0.694326174172893,1.01191248469782),(1.01107262942219,
0.694916621564155,1.01188947423726),(1.01104907236643,0.695565687462041,
1.01186417934145),(1.01104294959085,0.695734387866366,1.01185760487934),
(1.01107741820809,0.694784676483697,1.01189461629922),(1.01110652212194,
0.693982778395654,1.01192586725333),(1.01112142406403,0.693572186235118,
1.01194186853448),(1.01113071500695,0.693316193539388,1.01195184488448),
(1.01112525611268,0.693466602068436,1.01194598327923),(1.01111305723012,
0.693802717020363,1.01193288446644),(1.011091079394,0.694408270790531,1.01190928529172),
(1.01108796371199,0.694494116957465,1.01190593976108),(1.01101183808791,
0.696591600914965,1.01182419823323),(1.01107887545404,0.694744525088673,
1.01189618104843),(1.01102439606068,0.696245591975988,1.01183768262686)))
REPRESENTATION_ITEM('')
SURFACE()
);
#1690=(
BOUNDED_SURFACE()
B_SPLINE_SURFACE(3,2,((#46471,#46472,#46473),(#46474,#46475,#46476),(#46477,
#46478,#46479),(#46480,#46481,#46482),(#46483,#46484,#46485),(#46486,#46487,
#46488)),.UNSPECIFIED.,.F.,.F.,.F.)
B_SPLINE_SURFACE_WITH_KNOTS((4,1,1,4),(3,3),(0.00224117495089493,0.00389489708768512,
0.00509648123116401,0.00783693620606977),(0.,1.02101478396072),
 .UNSPECIFIED.)
GEOMETRIC_REPRESENTATION_ITEM()
RATIONAL_B_SPLINE_SURFACE(((1.,0.700585568194159,1.01258425919824),(1.,
0.700796860676309,1.01257537866651),(1.,0.70043057939319,1.01259077331058),
(1.,0.699548374367667,1.01262785200662),(1.,0.699365641730608,1.0126355321804),
(1.,0.69922285003429,1.0126415336537)))
REPRESENTATION_ITEM('')
SURFACE()
);
#1691=(
BOUNDED_SURFACE()
B_SPLINE_SURFACE(3,2,((#46563,#46564,#46565),(#46566,#46567,#46568),(#46569,
#46570,#46571),(#46572,#46573,#46574),(#46575,#46576,#46577),(#46578,#46579,
#46580),(#46581,#46582,#46583)),.UNSPECIFIED.,.F.,.F.,.F.)
B_SPLINE_SURFACE_WITH_KNOTS((4,1,1,1,4),(3,3),(0.0022673108647627,0.00394001125857995,
0.00515538157865687,0.00637075189873378,0.00792618538211219),(0.,1.00491872988737),
 .UNSPECIFIED.)
GEOMETRIC_REPRESENTATION_ITEM()
RATIONAL_B_SPLINE_SURFACE(((0.999999999999999,0.705232353097564,1.0028997648693),
(1.,0.705372001636867,1.00289839108241),(1.,0.705175813388567,1.00290032107641),
(1.,0.704343570165377,1.00290850823564),(1.,0.704147620189805,1.00291043588564),
(1.,0.704070859823098,1.00291119101266),(1.,0.704099757322705,1.00291090673467)))
REPRESENTATION_ITEM('')
SURFACE()
);
#1692=(
BOUNDED_SURFACE()
B_SPLINE_SURFACE(3,2,((#46621,#46622,#46623),(#46624,#46625,#46626),(#46627,
#46628,#46629),(#46630,#46631,#46632),(#46633,#46634,#46635),(#46636,#46637,
#46638),(#46639,#46640,#46641),(#46642,#46643,#46644),(#46645,#46646,#46647),
(#46648,#46649,#46650),(#46651,#46652,#46653),(#46654,#46655,#46656),(#46657,
#46658,#46659),(#46660,#46661,#46662),(#46663,#46664,#46665),(#46666,#46667,
#46668),(#46669,#46670,#46671),(#46672,#46673,#46674),(#46675,#46676,#46677),
(#46678,#46679,#46680),(#46681,#46682,#46683)),.UNSPECIFIED.,.F.,.F.,.F.)
B_SPLINE_SURFACE_WITH_KNOTS((4,1,1,1,1,1,1,1,1,1,1,1,1,1,1,1,1,1,4),(3,
3),(0.0026099542776046,0.00653870538517126,0.00765956913959363,0.00878043289401599,
0.00990129664843836,0.0110221604028607,0.0121430241572831,0.0132638879117055,
0.0143847516661278,0.0155056154205502,0.0160660472977614,0.0166264791749726,
0.0171869110521838,0.0177473429293949,0.0183077748066061,0.0188682066838173,
0.0199890704382397,0.021109934192662,0.023799829665576),(-0.00915496827453823,
1.00911975686673),.UNSPECIFIED.)
GEOMETRIC_REPRESENTATION_ITEM()
RATIONAL_B_SPLINE_SURFACE(((1.00540015433993,0.702355647466065,1.0053791968233),
(1.00542931479058,0.70074838906034,1.00540824410485),(1.00539359424759,
0.702717224990173,1.00537266219009),(1.00543444598592,0.700465569122908,
1.00541335538647),(1.00543429432824,0.700473928152822,1.00541320431736),
(1.0054419791353,0.700050358884654,1.00542085930037),(1.00544783298105,
0.699727708082337,1.00542669042788),(1.00545126427263,0.699538583014119,
1.00543010840291),(1.00545513095102,0.699325460403949,1.00543396007508),
(1.00545611971578,0.699270961915871,1.00543494500253),(1.00545189388041,
0.699503880450216,1.00543073556724),(1.00544147140227,0.700078343986232,
1.00542035353781),(1.00542302697162,0.701094959489083,1.00540198068835),
(1.00540736527206,0.701958197117509,1.00538637977044),(1.00541940619836,
0.701294528361412,1.00539837396699),(1.00542915527787,0.700757181042318,
1.00540808521119),(1.00543773400721,0.700284340789683,1.00541663064725),
(1.00544231061344,0.700032088555579,1.00542118949208),(1.0054454782231,
0.699857497040831,1.00542434480853),(1.00544494080388,0.699887118378614,
1.00542380947498),(1.0054436718169,0.699957062084557,1.00542254541283)))
REPRESENTATION_ITEM('')
SURFACE()
);
#1693=(
BOUNDED_SURFACE()
B_SPLINE_SURFACE(3,2,((#46706,#46707,#46708),(#46709,#46710,#46711),(#46712,
#46713,#46714),(#46715,#46716,#46717),(#46718,#46719,#46720),(#46721,#46722,
#46723),(#46724,#46725,#46726),(#46727,#46728,#46729),(#46730,#46731,#46732),
(#46733,#46734,#46735),(#46736,#46737,#46738),(#46739,#46740,#46741),(#46742,
#46743,#46744),(#46745,#46746,#46747),(#46748,#46749,#46750),(#46751,#46752,
#46753),(#46754,#46755,#46756),(#46757,#46758,#46759),(#46760,#46761,#46762)),
 .UNSPECIFIED.,.F.,.F.,.F.)
B_SPLINE_SURFACE_WITH_KNOTS((4,1,1,1,1,1,1,1,1,1,1,1,1,1,1,1,4),(3,3),(0.00261602648474055,
0.0065189601614092,0.00763244721963373,0.00874593427785826,0.0109729083943073,
0.0131998825107564,0.0143133695689809,0.0154268566272054,0.0159836001563177,
0.01654034368543,0.0170970872145422,0.0176538307436545,0.0182105742727668,
0.018767317801879,0.0198808048601036,0.0209942919183281,0.0236648513076151),
(-0.00774064349916484,1.01712637670702),.UNSPECIFIED.)
GEOMETRIC_REPRESENTATION_ITEM()
RATIONAL_B_SPLINE_SURFACE(((1.00456041043005,0.700340568355079,1.01018400253521),
(1.00458323931118,0.698840508294276,1.01023498246058),(1.00455494103971,
0.700699955832171,1.01017178865975),(1.00458745716147,0.698563358103575,
1.01024440148079),(1.00458727396229,0.698575395915544,1.01024399237267),
(1.00459859336925,0.69783161043644,1.01026927011268),(1.00460271760422,
0.697560611602978,1.01027848007745),(1.00460401826295,0.697475146783281,
1.01028138462123),(1.00460123571268,0.697657985026857,1.0102751708167),
(1.00459370847254,0.698152591496079,1.01025836148916),(1.00458255918927,
0.698885198338898,1.01023346365796),(1.00456722749737,0.699892626541195,
1.01019922595248),(1.00457157945601,0.699606664242021,1.01020894445446),
(1.00458110377577,0.698980831920699,1.01023021352619),(1.00458980036183,
0.698409389047836,1.01024963415859),(1.00459454344474,0.698097726413681,
1.01026022609304),(1.00459691632312,0.697941807248642,1.01026552504579),
(1.00459766104331,0.697892872523841,1.01026718810495),(1.00459534538961,
0.698045031519126,1.01026201694252)))
REPRESENTATION_ITEM('')
SURFACE()
);
#1694=(
BOUNDED_SURFACE()
B_SPLINE_SURFACE(3,2,((#46775,#46776,#46777),(#46778,#46779,#46780),(#46781,
#46782,#46783),(#46784,#46785,#46786),(#46787,#46788,#46789),(#46790,#46791,
#46792)),.UNSPECIFIED.,.F.,.F.,.F.)
B_SPLINE_SURFACE_WITH_KNOTS((4,1,1,4),(3,3),(0.00298650820277577,0.00587270729901942,
0.00708730098828811,0.00875892826895514),(-0.00731480018610578,1.04923751574683),
 .UNSPECIFIED.)
GEOMETRIC_REPRESENTATION_ITEM()
RATIONAL_B_SPLINE_SURFACE(((1.00433922363568,0.688684065923349,1.0304238586339),
(1.00433990537915,0.68863515449948,1.03042863858276),(1.00433814205992,
0.688761663161044,1.03041627531698),(1.00432100539233,0.689991126798849,
1.0302961239729),(1.00432211189368,0.689911741284742,1.03030388205205),
(1.004322288045,0.68989910337546,1.0303051171124)))
REPRESENTATION_ITEM('')
SURFACE()
);
#1695=(
BOUNDED_SURFACE()
B_SPLINE_SURFACE(3,2,((#46849,#46850,#46851),(#46852,#46853,#46854),(#46855,
#46856,#46857),(#46858,#46859,#46860),(#46861,#46862,#46863)),
 .UNSPECIFIED.,.F.,.F.,.F.)
B_SPLINE_SURFACE_WITH_KNOTS((4,1,4),(3,3),(0.00223740564663838,0.0050827929085138,
0.00792754419391784),(0.,1.02944699552801),.UNSPECIFIED.)
GEOMETRIC_REPRESENTATION_ITEM()
RATIONAL_B_SPLINE_SURFACE(((1.,0.698456271057167,1.01775911367536),(1.,
0.698436923194511,1.01776025314821),(1.,0.698505261200251,1.01775622845031),
(1.,0.698479809865279,1.017757727381),(1.,0.698365201647692,1.01776447711635)))
REPRESENTATION_ITEM('')
SURFACE()
);
#1696=(
BOUNDED_SURFACE()
B_SPLINE_SURFACE(3,2,((#46894,#46895,#46896),(#46897,#46898,#46899),(#46900,
#46901,#46902),(#46903,#46904,#46905)),.UNSPECIFIED.,.F.,.F.,.F.)
B_SPLINE_SURFACE_WITH_KNOTS((4,4),(3,3),(0.00378061934590702,0.00940525617675301),
(-0.0098380819768058,1.05450423974215),.UNSPECIFIED.)
GEOMETRIC_REPRESENTATION_ITEM()
RATIONAL_B_SPLINE_SURFACE(((1.00582192970445,0.687828329926041,1.03368087708045),
(1.00581735048427,0.688073867554131,1.03365438549437),(1.00582100747812,
0.68787777967012,1.03367554184055),(1.00582018844164,0.687921696378225,
1.03367080357187)))
REPRESENTATION_ITEM('')
SURFACE()
);
#1697=(
BOUNDED_SURFACE()
B_SPLINE_SURFACE(3,2,((#46941,#46942,#46943),(#46944,#46945,#46946),(#46947,
#46948,#46949),(#46950,#46951,#46952),(#46953,#46954,#46955),(#46956,#46957,
#46958),(#46959,#46960,#46961),(#46962,#46963,#46964),(#46965,#46966,#46967),
(#46968,#46969,#46970),(#46971,#46972,#46973),(#46974,#46975,#46976),(#46977,
#46978,#46979),(#46980,#46981,#46982),(#46983,#46984,#46985),(#46986,#46987,
#46988),(#46989,#46990,#46991)),.UNSPECIFIED.,.F.,.F.,.F.)
B_SPLINE_SURFACE_WITH_KNOTS((4,1,1,1,1,1,1,1,1,1,1,1,1,1,4),(3,3),(0.00180746184059761,
0.00487438597791521,0.00609862095279201,0.0073228559276688,0.0085470909025456,
0.0109955608522992,0.012219795827176,0.0134440308020528,0.0146682657769296,
0.0158925007518064,0.0171167357266832,0.01834097070156,0.0195652056764368,
0.0207894406513136,0.0250804959149023),(-0.0297036389200334,1.02228150212663),
 .UNSPECIFIED.)
GEOMETRIC_REPRESENTATION_ITEM()
RATIONAL_B_SPLINE_SURFACE(((1.01792057067006,0.691428609233124,1.01334580881894),
(1.01790539739825,0.691689875331743,1.01333450897875),(1.01794456212783,
0.691015504225207,1.01336367573928),(1.01790852581577,0.691636007619508,
1.01333683877409),(1.01801477009808,0.689806604607884,1.01341596102449),
(1.01801439627506,0.689813041405708,1.01341568263098),(1.01805278429309,
0.68915204436873,1.01344427095883),(1.01805069082588,0.689188091440009,
1.01344271191176),(1.01802936526785,0.68955529275428,1.01342683034048),
(1.0179780084348,0.690439597706898,1.01338858387568),(1.01791815953341,
0.691470126202861,1.01334401319706),(1.01791203091527,0.691575653881418,
1.01333944909207),(1.01795792283585,0.69078544836753,1.01337362572682),
(1.01799733489626,0.690106818511361,1.0134029766796),(1.018029784441,0.689548075080012,
1.01342714250714),(1.01804311488889,0.689318540266558,1.01343706995936),
(1.01799270295897,0.690186575085961,1.01339952718289)))
REPRESENTATION_ITEM('')
SURFACE()
);
#1698=(
BOUNDED_SURFACE()
B_SPLINE_SURFACE(3,2,((#47021,#47022,#47023),(#47024,#47025,#47026),(#47027,
#47028,#47029),(#47030,#47031,#47032),(#47033,#47034,#47035),(#47036,#47037,
#47038),(#47039,#47040,#47041),(#47042,#47043,#47044),(#47045,#47046,#47047),
(#47048,#47049,#47050),(#47051,#47052,#47053),(#47054,#47055,#47056),(#47057,
#47058,#47059),(#47060,#47061,#47062),(#47063,#47064,#47065),(#47066,#47067,
#47068)),.UNSPECIFIED.,.F.,.F.,.F.)
B_SPLINE_SURFACE_WITH_KNOTS((4,1,1,1,1,1,1,1,1,1,1,1,1,4),(3,3),(0.00174152498507269,
0.00601094925968871,0.00722900264372801,0.00844705602776732,0.00966510941180663,
0.0108831627958459,0.0121012161798852,0.0133192695639245,0.0145373229479639,
0.0157553763320032,0.0181914831000818,0.0194095364841211,0.0206275898681604,
0.0248970811962703),(-0.0178990764671792,1.06365987093854),
 .UNSPECIFIED.)
GEOMETRIC_REPRESENTATION_ITEM()
RATIONAL_B_SPLINE_SURFACE(((1.01072723796849,0.68092932560185,1.03986769249072),
(1.01074407302893,0.680428584022208,1.03993025985562),(1.01074291317966,
0.680463082547352,1.03992594928526),(1.01072004020438,0.681143415701839,
1.03984094205905),(1.01069798203529,0.681799513283581,1.03975896305336),
(1.01066933012785,0.682651734839026,1.03965247847288),(1.01067408104556,
0.682510423671846,1.03967013521984),(1.01070834185496,0.681491371089037,
1.03979746523874),(1.01073952588273,0.680563834214891,1.03991336042385),
(1.01075250782449,0.680177699692236,1.03996160770461),(1.01075350499417,
0.680148039904642,1.03996531367757),(1.01073183542055,0.680792579112819,
1.03988477888383),(1.01073000021761,0.680847165339321,1.03987795836704),
(1.01062128833396,0.684080688650128,1.03947393153737),(1.01073288101176,
0.680761479076527,1.03988866481501),(1.01059952149607,0.68472812088421,
1.03939303526176)))
REPRESENTATION_ITEM('')
SURFACE()
);
#1699=(
BOUNDED_SURFACE()
B_SPLINE_SURFACE(3,2,((#47076,#47077,#47078),(#47079,#47080,#47081),(#47082,
#47083,#47084),(#47085,#47086,#47087),(#47088,#47089,#47090),(#47091,#47092,
#47093),(#47094,#47095,#47096),(#47097,#47098,#47099),(#47100,#47101,#47102),
(#47103,#47104,#47105),(#47106,#47107,#47108),(#47109,#47110,#47111),(#47112,
#47113,#47114),(#47115,#47116,#47117),(#47118,#47119,#47120),(#47121,#47122,
#47123),(#47124,#47125,#47126)),.UNSPECIFIED.,.F.,.F.,.F.)
B_SPLINE_SURFACE_WITH_KNOTS((4,1,1,1,1,1,1,1,1,1,1,1,1,1,4),(3,3),(0.00226621447219306,
0.00524773882639187,0.00649265357668405,0.00773756832697622,0.0089824830772684,
0.0114723125778527,0.0127172273281449,0.0139621420784371,0.0152070568287293,
0.0164519715790214,0.0176968863293136,0.0189418010796058,0.020186715829898,
0.0214316305801901,0.0256040630347784),(0.,1.0152345218586),
 .UNSPECIFIED.)
GEOMETRIC_REPRESENTATION_ITEM()
RATIONAL_B_SPLINE_SURFACE(((1.,0.702313782623218,1.00907021437126),(1.,
0.702936907568063,1.00905122835008),(1.,0.702063225272511,1.00907784861414),
(1.,0.702911891024781,1.00905199058023),(1.,0.700831363730455,1.00911538225731),
(1.,0.70083848523692,1.00911516527182),(1.,0.70013918089471,1.0091364724064),
(1.,0.700266820798498,1.00913258334059),(1.,0.700674435878907,1.00912016369888),
(1.,0.701686628187104,1.00908932316719),(1.,0.702697815661407,1.00905851325183),
(1.,0.702654729965943,1.00905982603177),(1.,0.70185121745699,1.00908430828954),
(1.,0.701240439049059,1.00910291812355),(1.,0.700774764154181,1.00911710679228),
(1.,0.700672231940488,1.00912023085078),(1.,0.701062661849745,1.00910833482481)))
REPRESENTATION_ITEM('')
SURFACE()
);
#1700=(
BOUNDED_SURFACE()
B_SPLINE_SURFACE(3,2,((#47148,#47149,#47150),(#47151,#47152,#47153),(#47154,
#47155,#47156),(#47157,#47158,#47159),(#47160,#47161,#47162),(#47163,#47164,
#47165),(#47166,#47167,#47168),(#47169,#47170,#47171),(#47172,#47173,#47174),
(#47175,#47176,#47177),(#47178,#47179,#47180),(#47181,#47182,#47183),(#47184,
#47185,#47186),(#47187,#47188,#47189),(#47190,#47191,#47192),(#47193,#47194,
#47195),(#47196,#47197,#47198)),.UNSPECIFIED.,.F.,.F.,.F.)
B_SPLINE_SURFACE_WITH_KNOTS((4,1,1,1,1,1,1,1,1,1,1,1,1,1,4),(3,3),(-0.000294877643038348,
0.00281429782281611,0.00405540675591689,0.00529651568901767,0.00653762462211845,
0.00901984248832001,0.0102609514214208,0.0115020603545216,0.0127431692876223,
0.0139842782207231,0.0152253871538239,0.0164664960869247,0.0177076050200255,
0.0189487139531262,0.0232989706253928),(-0.0100183419747615,1.01952514777027),
 .UNSPECIFIED.)
GEOMETRIC_REPRESENTATION_ITEM()
RATIONAL_B_SPLINE_SURFACE(((1.00594367839033,0.697510790065643,1.0116929060728),
(1.00591694996598,0.698871068908738,1.01164032365921),(1.0059425385726,
0.69756879834631,1.01169066372711),(1.00591857689445,0.698788270298672,
1.0116435242903),(1.00596467551473,0.696442191942373,1.01173421338914),
(1.00596269074434,0.696543202055686,1.01173030878122),(1.00597755291228,
0.695786827780223,1.01175954689308),(1.00597476616083,0.695928652789648,
1.0117540645603),(1.00596594731885,0.696377466532329,1.0117367153896),(1.00594533763073,
0.697426347017788,1.01169617027065),(1.00592631693439,0.698394359590233,
1.01165875115051),(1.00592742439226,0.698337998186643,1.01166092983516),
(1.00594396371463,0.69749626917183,1.01169346738687),(1.00595489070713,
0.696940166181218,1.01171496388929),(1.00596573666354,0.696388187327233,
1.01173630097069),(1.00596720726343,0.696313344684252,1.01173919405899),
(1.00595737839104,0.696813561494266,1.01171985787118)))
REPRESENTATION_ITEM('')
SURFACE()
);
#1701=(
BOUNDED_SURFACE()
B_SPLINE_SURFACE(3,2,((#47200,#47201,#47202),(#47203,#47204,#47205),(#47206,
#47207,#47208),(#47209,#47210,#47211),(#47212,#47213,#47214),(#47215,#47216,
#47217),(#47218,#47219,#47220),(#47221,#47222,#47223),(#47224,#47225,#47226),
(#47227,#47228,#47229),(#47230,#47231,#47232)),.UNSPECIFIED.,.T.,.F.,.F.)
B_SPLINE_SURFACE_WITH_KNOTS((4,1,1,1,1,1,1,1,4),(3,3),(-0.0108993956052043,
-0.00953697115455376,-0.00817454670390322,-0.00681212225325268,-0.00544969780260214,
-0.0040872733519516,-0.00272484890130105,-0.00136242445065051,0.),(0.,1.00123227863135),
 .UNSPECIFIED.)
GEOMETRIC_REPRESENTATION_ITEM()
RATIONAL_B_SPLINE_SURFACE(((1.,0.706745855131733,1.00072274163255),(1.,
0.706745855131732,1.00072274163255),(1.,0.706745855131736,1.00072274163255),
(1.,0.706745855131741,1.00072274163255),(1.,0.706745855131734,1.00072274163255),
(1.,0.70674585513174,1.00072274163255),(1.,0.706745855131737,1.00072274163255),
(1.,0.706745855131739,1.00072274163255),(1.,0.706745855131743,1.00072274163255),
(1.,0.706745855131734,1.00072274163255),(1.,0.706745855131733,1.00072274163255)))
REPRESENTATION_ITEM('')
SURFACE()
);
#1702=(
BOUNDED_SURFACE()
B_SPLINE_SURFACE(3,2,((#47284,#47285,#47286),(#47287,#47288,#47289),(#47290,
#47291,#47292),(#47293,#47294,#47295),(#47296,#47297,#47298),(#47299,#47300,
#47301),(#47302,#47303,#47304),(#47305,#47306,#47307),(#47308,#47309,#47310),
(#47311,#47312,#47313),(#47314,#47315,#47316)),.UNSPECIFIED.,.T.,.F.,.F.)
B_SPLINE_SURFACE_WITH_KNOTS((4,1,1,1,1,1,1,1,4),(3,3),(-0.0121528522847183,
-0.0106337457491285,-0.00911463921353872,-0.00759553267794892,-0.00607642614235913,
-0.00455731960676934,-0.00303821307117955,-0.0015191065355898,0.),(-0.0120606504638825,
1.),.UNSPECIFIED.)
GEOMETRIC_REPRESENTATION_ITEM()
RATIONAL_B_SPLINE_SURFACE(((1.00811883844143,0.663416228430369,1.),(1.00823064312136,
0.658781126855077,1.),(1.0079877964772,0.668848852675098,1.),(1.00697574646344,
0.710805545508091,1.),(1.00731608298849,0.696696168652019,1.),(1.0083525815378,
0.653725909609466,1.),(1.00798713623623,0.668876224373087,1.),(1.00697515363204,
0.710830122598659,1.),(1.00731696839763,0.696659462126846,1.),(1.0080070337615,
0.66805133000566,1.),(1.00811883844143,0.663416228430369,1.)))
REPRESENTATION_ITEM('')
SURFACE()
);
#1703=(
BOUNDED_SURFACE()
B_SPLINE_SURFACE(3,2,((#47450,#47451,#47452),(#47453,#47454,#47455),(#47456,
#47457,#47458),(#47459,#47460,#47461),(#47462,#47463,#47464),(#47465,#47466,
#47467),(#47468,#47469,#47470),(#47471,#47472,#47473),(#47474,#47475,#47476),
(#47477,#47478,#47479),(#47480,#47481,#47482),(#47483,#47484,#47485),(#47486,
#47487,#47488),(#47489,#47490,#47491)),.UNSPECIFIED.,.T.,.F.,.F.)
B_SPLINE_SURFACE_WITH_KNOTS((4,1,1,1,1,1,1,1,3,4),(3,3),(-0.00765457458290781,
-0.00738843513850202,-0.00633294440443031,-0.00527745367035859,-0.00422196293628687,
-0.00316647220221515,-0.00211098146814344,-0.00105549073407172,0.,0.000789351289665934),
(0.,1.05454521855088),.UNSPECIFIED.)
GEOMETRIC_REPRESENTATION_ITEM()
RATIONAL_B_SPLINE_SURFACE(((1.,0.711036106532509,1.03152319744499),(1.,
0.709345031579044,1.03170767755084),(1.,0.70035057317659,1.03268888694945),
(1.,0.683782910015655,1.03449626056544),(1.,0.705801584459776,1.03209423374593),
(1.,0.727101128800789,1.0297706571437),(1.,0.705831990732036,1.03209091671239),
(1.,0.683783260356914,1.03449622234655),(1.,0.705820110962035,1.0320922126817),
(1.,0.720001022829777,1.03054521080754),(1.,0.720006348153552,1.03054462986564),
(1.,0.720010330709774,1.03054419540685),(1.,0.716051718549058,1.03097604213777),
(1.,0.711036106532509,1.03152319744499)))
REPRESENTATION_ITEM('')
SURFACE()
);
#1704=(
BOUNDED_SURFACE()
B_SPLINE_SURFACE(3,2,((#47877,#47878,#47879),(#47880,#47881,#47882),(#47883,
#47884,#47885),(#47886,#47887,#47888),(#47889,#47890,#47891),(#47892,#47893,
#47894),(#47895,#47896,#47897),(#47898,#47899,#47900),(#47901,#47902,#47903),
(#47904,#47905,#47906),(#47907,#47908,#47909)),.UNSPECIFIED.,.T.,.F.,.F.)
B_SPLINE_SURFACE_WITH_KNOTS((4,1,1,1,1,1,1,1,4),(3,3),(0.,0.00105549073407172,
0.00211098146814343,0.00316647220221515,0.00422196293628687,0.00527745367035859,
0.0063329444044303,0.00738843513850202,0.00844392587257374),(0.,1.05454521855088),
 .UNSPECIFIED.)
GEOMETRIC_REPRESENTATION_ITEM()
RATIONAL_B_SPLINE_SURFACE(((1.,0.720006348153552,1.03054462986564),(1.,
0.720011673477327,1.03054404892375),(1.,0.705852062904688,1.03208872703031),
(1.,0.683782910015655,1.03449626056544),(1.,0.705801584459776,1.03209423374593),
(1.,0.727101128800789,1.0297706571437),(1.,0.705831990732036,1.03209091671239),
(1.,0.683783260356914,1.03449622234655),(1.,0.705820110962035,1.0320922126817),
(1.,0.720001022829777,1.03054521080754),(1.,0.720006348153552,1.03054462986564)))
REPRESENTATION_ITEM('')
SURFACE()
);
#1705=(
BOUNDED_SURFACE()
B_SPLINE_SURFACE(3,2,((#47910,#47911,#47912),(#47913,#47914,#47915),(#47916,
#47917,#47918),(#47919,#47920,#47921),(#47922,#47923,#47924),(#47925,#47926,
#47927),(#47928,#47929,#47930),(#47931,#47932,#47933),(#47934,#47935,#47936),
(#47937,#47938,#47939),(#47940,#47941,#47942)),.UNSPECIFIED.,.T.,.F.,.F.)
B_SPLINE_SURFACE_WITH_KNOTS((4,1,1,1,1,1,1,1,4),(3,3),(0.,0.00151910653558979,
0.00303821307117958,0.00455731960676938,0.00607642614235917,0.00759553267794896,
0.00911463921353875,0.0106337457491285,0.0121528522847183),(-0.0120606504638825,
1.),.UNSPECIFIED.)
GEOMETRIC_REPRESENTATION_ITEM()
RATIONAL_B_SPLINE_SURFACE(((1.00811883844143,0.663416228430369,1.),(1.00823064312136,
0.658781126855077,1.),(1.0079877964772,0.668848852675098,1.),(1.00697574646344,
0.710805545508091,1.),(1.00731608298849,0.696696168652019,1.),(1.0083525815378,
0.653725909609466,1.),(1.00798713623623,0.668876224373087,1.),(1.00697515363204,
0.710830122598659,1.),(1.00731696839763,0.696659462126846,1.),(1.0080070337615,
0.66805133000566,1.),(1.00811883844143,0.663416228430369,1.)))
REPRESENTATION_ITEM('')
SURFACE()
);
#1706=(
BOUNDED_SURFACE()
B_SPLINE_SURFACE(3,2,((#47945,#47946,#47947),(#47948,#47949,#47950),(#47951,
#47952,#47953),(#47954,#47955,#47956),(#47957,#47958,#47959),(#47960,#47961,
#47962),(#47963,#47964,#47965),(#47966,#47967,#47968),(#47969,#47970,#47971),
(#47972,#47973,#47974),(#47975,#47976,#47977)),.UNSPECIFIED.,.T.,.F.,.F.)
B_SPLINE_SURFACE_WITH_KNOTS((4,1,1,1,1,1,1,1,4),(3,3),(0.,0.00136242445065054,
0.00272484890130108,0.00408727335195162,0.00544969780260216,0.0068121222532527,
0.00817454670390325,0.00953697115455379,0.0108993956052043),(0.,1.00123227863135),
 .UNSPECIFIED.)
GEOMETRIC_REPRESENTATION_ITEM()
RATIONAL_B_SPLINE_SURFACE(((1.,0.706745855131733,1.00072274163255),(1.,
0.706745855131732,1.00072274163255),(1.,0.706745855131736,1.00072274163255),
(1.,0.706745855131741,1.00072274163255),(1.,0.706745855131734,1.00072274163255),
(1.,0.70674585513174,1.00072274163255),(1.,0.706745855131737,1.00072274163255),
(1.,0.706745855131739,1.00072274163255),(1.,0.706745855131743,1.00072274163255),
(1.,0.706745855131734,1.00072274163255),(1.,0.706745855131733,1.00072274163255)))
REPRESENTATION_ITEM('')
SURFACE()
);
#1707=(
BOUNDED_SURFACE()
B_SPLINE_SURFACE(3,2,((#49132,#49133,#49134),(#49135,#49136,#49137),(#49138,
#49139,#49140),(#49141,#49142,#49143),(#49144,#49145,#49146),(#49147,#49148,
#49149),(#49150,#49151,#49152),(#49153,#49154,#49155),(#49156,#49157,#49158),
(#49159,#49160,#49161),(#49162,#49163,#49164)),.UNSPECIFIED.,.T.,.F.,.F.)
B_SPLINE_SURFACE_WITH_KNOTS((4,1,1,1,1,1,1,1,4),(3,3),(-0.010465367918601,
-0.00915719692877588,-0.00784902593895075,-0.00654085494912563,-0.00523268395930051,
-0.00392451296947538,-0.00261634197965026,-0.00130817098982514,0.),(-9.28189933853903E-5,
1.00709936745582),.UNSPECIFIED.)
GEOMETRIC_REPRESENTATION_ITEM()
RATIONAL_B_SPLINE_SURFACE(((1.00005816990851,0.684423875674772,1.00448036293941),
(1.0000582548459,0.683963083961899,1.00448690498728),(1.00005264871468,
0.714376767023455,1.00405510952515),(1.00004410969851,0.760701571366749,
1.00339741738511),(1.00005214672296,0.717100109865145,1.00401644511616),
(1.000061052267,0.66878686428705,1.00470236796737),(1.00005266324573,0.714297935018859,
1.00405622873527),(1.00004410774396,0.760712174947014,1.00339726684175),
(1.00005213909035,0.717141517300695,1.00401585723791),(1.00005808497112,
0.684884667387646,1.00447382089153),(1.00005816990851,0.684423875674772,
1.00448036293941)))
REPRESENTATION_ITEM('')
SURFACE()
);
#1708=(
BOUNDED_SURFACE()
B_SPLINE_SURFACE(3,2,((#49225,#49226,#49227),(#49228,#49229,#49230),(#49231,
#49232,#49233),(#49234,#49235,#49236),(#49237,#49238,#49239),(#49240,#49241,
#49242),(#49243,#49244,#49245),(#49246,#49247,#49248),(#49249,#49250,#49251),
(#49252,#49253,#49254),(#49255,#49256,#49257)),.UNSPECIFIED.,.T.,.F.,.F.)
B_SPLINE_SURFACE_WITH_KNOTS((4,1,1,1,1,1,1,1,4),(3,3),(-0.010465367918601,
-0.00915719692877587,-0.00784902593895075,-0.00654085494912562,-0.00523268395930049,
-0.00392451296947537,-0.00261634197965024,-0.00130817098982511,0.),(-9.28189933903628E-5,
1.0070993674559),.UNSPECIFIED.)
GEOMETRIC_REPRESENTATION_ITEM()
RATIONAL_B_SPLINE_SURFACE(((1.00005816990851,0.684423875674746,1.00448036293946),
(1.0000582548459,0.683963083961873,1.00448690498733),(1.00005264871469,
0.714376767023432,1.0040551095252),(1.00004410969851,0.760701571366722,
1.00339741738514),(1.00005214672296,0.717100109865137,1.00401644511621),
(1.000061052267,0.668786864287018,1.00470236796742),(1.00005266324573,0.714297935018832,
1.00405622873532),(1.00004410774396,0.760712174947011,1.00339726684179),
(1.00005213909036,0.717141517300666,1.00401585723796),(1.00005808497112,
0.684884667387618,1.00447382089158),(1.00005816990851,0.684423875674746,
1.00448036293946)))
REPRESENTATION_ITEM('')
SURFACE()
);
#1709=(
BOUNDED_SURFACE()
B_SPLINE_SURFACE(3,2,((#49318,#49319,#49320),(#49321,#49322,#49323),(#49324,
#49325,#49326),(#49327,#49328,#49329),(#49330,#49331,#49332),(#49333,#49334,
#49335),(#49336,#49337,#49338),(#49339,#49340,#49341),(#49342,#49343,#49344),
(#49345,#49346,#49347),(#49348,#49349,#49350)),.UNSPECIFIED.,.T.,.F.,.F.)
B_SPLINE_SURFACE_WITH_KNOTS((4,1,1,1,1,1,1,1,4),(3,3),(-0.010465367918601,
-0.00915719692877587,-0.00784902593895075,-0.00654085494912562,-0.00523268395930049,
-0.00392451296947537,-0.00261634197965024,-0.00130817098982511,0.),(-9.28189933861358E-5,
1.00709936745573),.UNSPECIFIED.)
GEOMETRIC_REPRESENTATION_ITEM()
RATIONAL_B_SPLINE_SURFACE(((1.00005816990851,0.6844238756748,1.00448036293935),
(1.0000582548459,0.683963083961927,1.00448690498722),(1.00005264871468,
0.714376767023479,1.0040551095251),(1.00004410969851,0.760701571366764,
1.00339741738506),(1.00005214672296,0.717100109865185,1.00401644511611),
(1.000061052267,0.668786864287076,1.00470236796731),(1.00005266324573,0.714297935018881,
1.00405622873522),(1.00004410774396,0.760712174947052,1.00339726684171),
(1.00005213909035,0.717141517300717,1.00401585723786),(1.00005808497112,
0.684884667387673,1.00447382089148),(1.00005816990851,0.6844238756748,1.00448036293935)))
REPRESENTATION_ITEM('')
SURFACE()
);
#1710=(
BOUNDED_SURFACE()
B_SPLINE_SURFACE(3,2,((#49411,#49412,#49413),(#49414,#49415,#49416),(#49417,
#49418,#49419),(#49420,#49421,#49422),(#49423,#49424,#49425),(#49426,#49427,
#49428),(#49429,#49430,#49431),(#49432,#49433,#49434),(#49435,#49436,#49437),
(#49438,#49439,#49440),(#49441,#49442,#49443)),.UNSPECIFIED.,.T.,.F.,.F.)
B_SPLINE_SURFACE_WITH_KNOTS((4,1,1,1,1,1,1,1,4),(3,3),(-0.0104653679186011,
-0.00915719692877597,-0.00784902593895083,-0.0065408549491257,-0.00523268395930056,
-0.00392451296947543,-0.0026163419796503,-0.00130817098982516,0.),(-9.28189933908896E-5,
1.00709936745538),.UNSPECIFIED.)
GEOMETRIC_REPRESENTATION_ITEM()
RATIONAL_B_SPLINE_SURFACE(((1.00005816990851,0.684423875674909,1.00448036293913),
(1.0000582548459,0.683963083962039,1.004486904987),(1.00005264871469,0.714376767023586,
1.0040551095249),(1.00004410969851,0.760701571366847,1.00339741738489),
(1.00005214672296,0.717100109865272,1.00401644511591),(1.000061052267,0.668786864287198,
1.00470236796707),(1.00005266324573,0.714297935018957,1.00405622873502),
(1.00004410774396,0.760712174947142,1.00339726684154),(1.00005213909036,
0.717141517300806,1.00401585723766),(1.00005808497112,0.68488466738778,
1.00447382089125),(1.00005816990851,0.684423875674909,1.00448036293913)))
REPRESENTATION_ITEM('')
SURFACE()
);
#1711=(
BOUNDED_SURFACE()
B_SPLINE_SURFACE(3,2,((#49504,#49505,#49506),(#49507,#49508,#49509),(#49510,
#49511,#49512),(#49513,#49514,#49515),(#49516,#49517,#49518),(#49519,#49520,
#49521),(#49522,#49523,#49524),(#49525,#49526,#49527),(#49528,#49529,#49530),
(#49531,#49532,#49533),(#49534,#49535,#49536)),.UNSPECIFIED.,.T.,.F.,.F.)
B_SPLINE_SURFACE_WITH_KNOTS((4,1,1,1,1,1,1,1,4),(3,3),(-0.010465367918601,
-0.00915719692877588,-0.00784902593895076,-0.00654085494912564,-0.00523268395930052,
-0.0039245129694754,-0.00261634197965027,-0.00130817098982515,0.),(-9.28189933859035E-5,
1.00709936745473),.UNSPECIFIED.)
GEOMETRIC_REPRESENTATION_ITEM()
RATIONAL_B_SPLINE_SURFACE(((1.00005816990851,0.684423875675114,1.00448036293871),
(1.0000582548459,0.683963083962243,1.00448690498659),(1.00005264871468,
0.71437676702377,1.00405510952452),(1.00004410969851,0.760701571367001,
1.00339741738458),(1.00005214672296,0.717100109865461,1.00401644511554),
(1.000061052267,0.668786864287407,1.00470236796664),(1.00005266324573,0.714297935019167,
1.00405622873464),(1.00004410774396,0.760712174947296,1.00339726684123),
(1.00005213909035,0.717141517300991,1.00401585723729),(1.00005808497112,
0.684884667387984,1.00447382089084),(1.00005816990851,0.684423875675114,
1.00448036293871)))
REPRESENTATION_ITEM('')
SURFACE()
);
#1712=(
BOUNDED_SURFACE()
B_SPLINE_SURFACE(3,2,((#51569,#51570,#51571),(#51572,#51573,#51574),(#51575,
#51576,#51577),(#51578,#51579,#51580),(#51581,#51582,#51583),(#51584,#51585,
#51586),(#51587,#51588,#51589),(#51590,#51591,#51592),(#51593,#51594,#51595),
(#51596,#51597,#51598),(#51599,#51600,#51601),(#51602,#51603,#51604),(#51605,
#51606,#51607),(#51608,#51609,#51610),(#51611,#51612,#51613),(#51614,#51615,
#51616),(#51617,#51618,#51619),(#51620,#51621,#51622),(#51623,#51624,#51625),
(#51626,#51627,#51628),(#51629,#51630,#51631),(#51632,#51633,#51634),(#51635,
#51636,#51637),(#51638,#51639,#51640),(#51641,#51642,#51643),(#51644,#51645,
#51646),(#51647,#51648,#51649),(#51650,#51651,#51652),(#51653,#51654,#51655),
(#51656,#51657,#51658),(#51659,#51660,#51661),(#51662,#51663,#51664),(#51665,
#51666,#51667),(#51668,#51669,#51670),(#51671,#51672,#51673),(#51674,#51675,
#51676),(#51677,#51678,#51679),(#51680,#51681,#51682),(#51683,#51684,#51685),
(#51686,#51687,#51688),(#51689,#51690,#51691),(#51692,#51693,#51694),(#51695,
#51696,#51697),(#51698,#51699,#51700),(#51701,#51702,#51703),(#51704,#51705,
#51706),(#51707,#51708,#51709),(#51710,#51711,#51712),(#51713,#51714,#51715),
(#51716,#51717,#51718),(#51719,#51720,#51721)),.UNSPECIFIED.,.F.,.F.,.F.)
B_SPLINE_SURFACE_WITH_KNOTS((4,1,1,1,1,1,1,1,1,1,1,1,1,1,1,1,1,1,1,1,1,
1,1,1,1,1,1,1,1,1,1,1,1,1,1,1,1,1,1,1,1,1,1,1,1,1,1,1,4),(3,3),(0.0518556011495693,
0.0527138134588282,0.053572025768087,0.0544302380773458,0.0552884503866047,
0.0557175565412341,0.0561466626958635,0.056575768850493,0.0570048750051224,
0.0572194280824371,0.0574339811597518,0.0576485342370665,0.0577558107757239,
0.0578630873143813,0.0579703638530386,0.058077640391696,0.0581849169303533,
0.058238555199682,0.0582921934690107,0.058319012603675,0.0583324221710072,
0.0583458317383393,0.0583525365220054,0.0583592413056715,0.0583726508730037,
0.058399470007668,0.0584262891423324,0.0584531082769967,0.058479927411661,
0.0585067465463254,0.0585335656809897,0.0585603848156541,0.0586140230849827,
0.0586676613543114,0.0587212996236401,0.0588285761622974,0.0589358527009548,
0.0591504057782695,0.0593649588555842,0.0595795119328989,0.0597940650102137,
0.0600086180875284,0.0604377242421578,0.0608668303967872,0.0612959365514166,
0.0621541488606755,0.0630123611699343,0.0638705734791932,0.0655869980977109),
(0.,0.992792082539057),.UNSPECIFIED.)
GEOMETRIC_REPRESENTATION_ITEM()
RATIONAL_B_SPLINE_SURFACE(((1.,0.972633129448393,0.999605483711799),(1.,
0.972466377099184,0.99960307983746),(1.,0.972148941685609,0.99959850374094),
(1.,0.971773197203986,0.99959308707052),(1.,0.971559616448449,0.999590008125606),
(1.,0.971579911851545,0.999590300700786),(1.,0.971765309373093,0.999592973360852),
(1.,0.972004806824618,0.999596425916577),(1.,0.972363384740146,0.999601595116614),
(1.,0.972780617477487,0.99960760987488),(1.,0.973200212475753,0.999613658687109),
(1.,0.973562382687643,0.999618879673097),(1.,0.973908001496278,0.999623862056788),
(1.,0.974213764697866,0.999628269888628),(1.,0.974458567755711,0.999631798929098),
(1.,0.974719713112157,0.999635563557447),(1.,0.974998257795603,0.999639579011622),
(1.,0.975245417202801,0.999643142020835),(1.,0.975453404959813,0.999646140338006),
(1.,0.975586309882469,0.999648056273432),(1.,0.975684096253627,0.999649465945616),
(1.,0.975736704855896,0.999650224342542),(1.,0.975779062452084,0.999650834962656),
(1.,0.975792003625264,0.999651021520472),(1.,0.975908768836828,0.999652704788487),
(1.,0.976065613949059,0.999654965841733),(1.,0.976313695495099,0.999658542144348),
(1.,0.976550038655931,0.999661949228339),(1.,0.976622806276155,0.99966299823434),
(1.,0.975803080158142,0.999651181197942),(1.,0.974689019040623,0.999635121076779),
(1.,0.973731835785377,0.999621322480981),(1.,0.972580633402563,0.999604726937469),
(1.,0.971352050442573,0.99958701588833),(1.,0.970101157684635,0.999568983224826),
(1.,0.968635702989752,0.999547857471859),(1.,0.96708115063371,0.999525447301717),
(1.,0.964966417199759,0.999494961653629),(1.,0.962813822852091,0.99946393020886),
(1.,0.960726792115487,0.999433843918284),(1.,0.958985775800798,0.999408745714495),
(1.,0.957502218932609,0.999387359003586),(1.,0.955794846906811,0.999362745810312),
(1.,0.954070061596803,0.999337881590007),(1.,0.952465322779582,0.999314747940125),
(1.,0.950801594537222,0.999290763908429),(1.,0.949428667831148,0.999270972023674),
(1.,0.948542326646378,0.99925819467547),(1.,0.948107945986102,0.999251932715578),
(1.,0.948414256938409,0.999256348443701),(1.,0.948789582111737,0.999261759069442)))
REPRESENTATION_ITEM('')
SURFACE()
);
#1713=(
BOUNDED_SURFACE()
B_SPLINE_SURFACE(3,2,((#51924,#51925,#51926),(#51927,#51928,#51929),(#51930,
#51931,#51932),(#51933,#51934,#51935),(#51936,#51937,#51938),(#51939,#51940,
#51941),(#51942,#51943,#51944),(#51945,#51946,#51947),(#51948,#51949,#51950),
(#51951,#51952,#51953),(#51954,#51955,#51956)),.UNSPECIFIED.,.F.,.F.,.F.)
B_SPLINE_SURFACE_WITH_KNOTS((4,1,1,1,1,1,1,1,4),(3,3),(0.0274600167716821,
0.0306293591014511,0.0337987014312201,0.036968043760989,0.040137386090758,
0.043306728420527,0.046476070750296,0.049645413080065,0.0528147554098339),
(0.,0.999158823292938),.UNSPECIFIED.)
GEOMETRIC_REPRESENTATION_ITEM()
RATIONAL_B_SPLINE_SURFACE(((1.,0.972499180711492,0.999953733902779),(1.,
0.969563181973315,0.999948794515278),(1.,0.964404879424878,0.999940116427374),
(1.,0.959820144441259,0.999932403282822),(1.,0.957768745632045,0.999928952105031),
(1.,0.957323191790612,0.999928202526005),(1.,0.957772770292401,0.999928958875932),
(1.,0.959817788845774,0.999932399319878),(1.,0.964400556847234,0.999940109155271),
(1.,0.969511549840245,0.999948707651782),(1.,0.972457626668796,0.999953663994193)))
REPRESENTATION_ITEM('')
SURFACE()
);
#1714=(
BOUNDED_SURFACE()
B_SPLINE_SURFACE(3,2,((#52002,#52003,#52004),(#52005,#52006,#52007),(#52008,
#52009,#52010),(#52011,#52012,#52013),(#52014,#52015,#52016),(#52017,#52018,
#52019),(#52020,#52021,#52022),(#52023,#52024,#52025),(#52026,#52027,#52028),
(#52029,#52030,#52031),(#52032,#52033,#52034),(#52035,#52036,#52037),(#52038,
#52039,#52040),(#52041,#52042,#52043),(#52044,#52045,#52046),(#52047,#52048,
#52049),(#52050,#52051,#52052),(#52053,#52054,#52055),(#52056,#52057,#52058),
(#52059,#52060,#52061),(#52062,#52063,#52064),(#52065,#52066,#52067),(#52068,
#52069,#52070),(#52071,#52072,#52073),(#52074,#52075,#52076),(#52077,#52078,
#52079),(#52080,#52081,#52082),(#52083,#52084,#52085),(#52086,#52087,#52088),
(#52089,#52090,#52091),(#52092,#52093,#52094),(#52095,#52096,#52097),(#52098,
#52099,#52100),(#52101,#52102,#52103),(#52104,#52105,#52106),(#52107,#52108,
#52109),(#52110,#52111,#52112),(#52113,#52114,#52115),(#52116,#52117,#52118),
(#52119,#52120,#52121),(#52122,#52123,#52124),(#52125,#52126,#52127),(#52128,
#52129,#52130),(#52131,#52132,#52133),(#52134,#52135,#52136),(#52137,#52138,
#52139),(#52140,#52141,#52142),(#52143,#52144,#52145),(#52146,#52147,#52148),
(#52149,#52150,#52151),(#52152,#52153,#52154)),.UNSPECIFIED.,.F.,.F.,.F.)
B_SPLINE_SURFACE_WITH_KNOTS((4,1,1,1,1,1,1,1,1,1,1,1,1,1,1,1,1,1,1,1,1,
1,1,1,1,1,1,1,1,1,1,1,1,1,1,1,1,1,1,1,1,1,1,1,1,1,1,1,4),(3,3),(0.0549773880899424,
0.0558467220379677,0.056716055985993,0.0575853899340184,0.0584547238820437,
0.0588893908560563,0.059324057830069,0.0597587248040816,0.0601933917780943,
0.0604107252651006,0.060628058752107,0.0608453922391133,0.0609540589826165,
0.0610627257261196,0.0611713924696228,0.061280059213126,0.0613343925848776,
0.0613887259566291,0.0614430593283807,0.0614702260142565,0.0614973927001323,
0.0615109760430702,0.0615177677145391,0.0615245593860081,0.061538142728946,
0.0615517260718839,0.0616060594436355,0.0616332261295112,0.061660392815387,
0.0617147261871386,0.0617690595588902,0.0618233929306418,0.0618777263023934,
0.061932059674145,0.0620407264176481,0.0621493931611513,0.0622580599046544,
0.0623667266481576,0.0625840601351639,0.0628013936221703,0.0630187271091766,
0.0632360605961829,0.0636707275701956,0.0641053945442083,0.0645400615182209,
0.0654093954662462,0.0662787294142715,0.0671480633622969,0.0688867312583475),
(0.0071934162772836,1.),.UNSPECIFIED.)
GEOMETRIC_REPRESENTATION_ITEM()
RATIONAL_B_SPLINE_SURFACE(((0.999606865695227,0.972674019574369,1.),(0.999604493486164,
0.972509132059776,1.),(0.999599985924059,0.972195820419529,1.),(0.99959469878352,
0.97182832183922,1.),(0.999591787920345,0.971625993553036,1.),(0.999592262320468,
0.971658968158147,1.),(0.999595111580877,0.971857014559129,1.),(0.999598719790412,
0.972107813998253,1.),(0.999604075332896,0.972480067061186,1.),(0.999610278894004,
0.972911264205102,1.),(0.999616504333946,0.973343982103104,1.),(0.999621872051548,
0.973717081434168,1.),(0.999626989683936,0.974072797841428,1.),(0.999631514141331,
0.97438728383948,1.),(0.999635134621242,0.974638936167879,1.),(0.999638995891387,
0.974907325344667,1.),(0.999642423004491,0.975145537132501,1.),(0.999645303509732,
0.975345755299341,1.),(0.999647519951942,0.975499815771031,1.),(0.999649466882302,
0.975635143012321,1.),(0.999650966259817,0.975739361749083,1.),(0.999652131141739,
0.975820330365203,1.),(0.999652527992851,0.975847914693448,1.),(0.999653424322134,
0.975910216751927,1.),(0.99965486617898,0.976010437341898,1.),(0.999656495605389,
0.976123695517568,1.),(0.999660353374776,0.976391841363585,1.),(0.999665654480073,
0.976760310606368,1.),(0.999660382980781,0.97639389921788,1.),(0.999642122172533,
0.975124626903821,1.),(0.999618855766348,0.973507425473537,1.),(0.999597068940179,
0.971993066695347,1.),(0.999578353121333,0.970692167503353,1.),(0.999561988209168,
0.969554675139877,1.),(0.999542407463857,0.968193656636564,1.),(0.999521161635198,
0.966716901514952,1.),(0.99949931886217,0.965198653982345,1.),(0.999480183940009,
0.963868623755846,1.),(0.999457441535243,0.962287844617692,1.),(0.999433158062626,
0.960599948930796,1.),(0.999408652723323,0.958896631733652,1.),(0.999387680310542,
0.957438881203672,1.),(0.99936345490367,0.955755021550734,1.),(0.99933892884738,
0.954050264357146,1.),(0.999316157675712,0.952467485689127,1.),(0.999292552850348,
0.950826761417559,1.),(0.999273004213266,0.949467974693082,1.),(0.999260366937433,
0.948589582886857,1.),(0.999254191533472,0.94816034288997,1.),(0.999258647490592,
0.948470067570712,1.),(0.999264080382697,0.948847697051352,1.)))
REPRESENTATION_ITEM('')
SURFACE()
);
#1715=(
BOUNDED_SURFACE()
B_SPLINE_SURFACE(3,2,((#52310,#52311,#52312),(#52313,#52314,#52315),(#52316,
#52317,#52318),(#52319,#52320,#52321),(#52322,#52323,#52324),(#52325,#52326,
#52327),(#52328,#52329,#52330),(#52331,#52332,#52333),(#52334,#52335,#52336),
(#52337,#52338,#52339),(#52340,#52341,#52342),(#52343,#52344,#52345),(#52346,
#52347,#52348),(#52349,#52350,#52351),(#52352,#52353,#52354),(#52355,#52356,
#52357),(#52358,#52359,#52360),(#52361,#52362,#52363),(#52364,#52365,#52366),
(#52367,#52368,#52369),(#52370,#52371,#52372),(#52373,#52374,#52375),(#52376,
#52377,#52378),(#52379,#52380,#52381),(#52382,#52383,#52384),(#52385,#52386,
#52387),(#52388,#52389,#52390),(#52391,#52392,#52393),(#52394,#52395,#52396),
(#52397,#52398,#52399),(#52400,#52401,#52402),(#52403,#52404,#52405),(#52406,
#52407,#52408),(#52409,#52410,#52411),(#52412,#52413,#52414),(#52415,#52416,
#52417),(#52418,#52419,#52420),(#52421,#52422,#52423),(#52424,#52425,#52426),
(#52427,#52428,#52429),(#52430,#52431,#52432),(#52433,#52434,#52435),(#52436,
#52437,#52438),(#52439,#52440,#52441),(#52442,#52443,#52444),(#52445,#52446,
#52447),(#52448,#52449,#52450),(#52451,#52452,#52453),(#52454,#52455,#52456)),
 .UNSPECIFIED.,.F.,.F.,.F.)
B_SPLINE_SURFACE_WITH_KNOTS((4,1,1,1,1,1,1,1,1,1,1,1,1,1,1,1,1,1,1,1,1,
1,1,1,1,1,1,1,1,1,1,1,1,1,1,1,1,1,1,1,1,1,1,1,1,1,4),(3,3),(0.0264470415813064,
0.0280904658576036,0.0289121779957522,0.0297338901339008,0.0305556022720494,
0.031377314410198,0.0317881704792723,0.0321990265483466,0.0326098826174209,
0.0330207386864952,0.0332261667210323,0.0334315947555695,0.0336370227901066,
0.0338424508246438,0.0339451648419123,0.0340478788591809,0.0341505928764495,
0.0342533068937181,0.0343046639023524,0.0343560209109866,0.0344073779196209,
0.0344587349282552,0.0344844134325724,0.0344908330586516,0.0344972526847309,
0.0345036723108102,0.0345100919368895,0.0345229311890481,0.0345357704412066,
0.0345614489455238,0.0345871274498409,0.0346128059541581,0.0346641629627924,
0.0347155199714267,0.034766876980061,0.0348695909973295,0.0349723050145981,
0.0350750190318667,0.0352804470664038,0.035485875100941,0.0358967311700153,
0.0363075872390896,0.0367184433081639,0.0371292993772382,0.0379510115153868,
0.0387727236535354,0.039594435791684),(0.0092590728241763,1.00003353933066),
 .UNSPECIFIED.)
GEOMETRIC_REPRESENTATION_ITEM()
RATIONAL_B_SPLINE_SURFACE(((0.99978961747398,0.988638737368156,1.0000007692208),
(0.999781382332911,0.988194016020487,1.00000079933091),(0.999768697684378,
0.987509008448325,1.00000084570974),(0.999753627458576,0.986695172829483,
1.00000090081095),(0.999744161654649,0.986183992141261,1.00000093542073),
(0.999737468268737,0.985822530014733,1.00000095989373),(0.99973519309943,
0.985699664316171,1.00000096821242),(0.99973614054353,0.985750829027678,
1.00000096474829),(0.999738491598624,0.985877792777406,1.00000095615213),
(0.999742772930425,0.986108997031503,1.00000094049832),(0.999748231548623,
0.986403778143447,1.00000092053999),(0.999753939590464,0.986712028850878,
1.0000008996697),(0.999758950041984,0.986982607670794,1.00000088135001),
(0.999764751091548,0.987295881063196,1.00000086013965),(0.999770296259429,
0.98759533610742,1.00000083986488),(0.999775187421617,0.98785947295972,
1.00000082198134),(0.999779088017462,0.988070116375048,1.00000080771961),
(0.999783226816312,0.988293623439104,1.00000079258693),(0.999786866208497,
0.988490161104194,1.00000077928024),(0.999789885779805,0.988653226655847,
1.00000076823979),(0.999792201848896,0.988778301060619,1.00000075977156),
(0.999794571142586,0.988906249747113,1.00000075110872),(0.999796573339135,
0.989014374130155,1.0000007437881),(0.999797909962534,0.989086555645273,
1.00000073890101),(0.999798507874639,0.989118844621846,1.00000073671486),
(0.999798847443193,0.989137182302254,1.0000007354733),(0.999799031432296,
0.989147118243971,1.00000073480058),(0.999802525289213,0.989335796585208,
1.000000722026),(0.999804716867525,0.989454148129176,1.00000071401295),
(0.99980662464054,0.989557173369326,1.00000070703756),(0.999804818702909,
0.989459647533336,1.00000071364061),(0.99979931983484,0.989162692812403,
1.00000073374609),(0.999790180893756,0.988669163659588,1.00000076716077),
(0.999777974706557,0.98800999437815,1.0000008117902),(0.99976387234001,
0.987248425947972,1.00000086335263),(0.999746122600327,0.986289888858417,
1.00000092825093),(0.999726420849751,0.985225937555842,1.00000100028637),
(0.999705699374946,0.9841069182065,1.00000107605021),(0.99968115178329,
0.982781277522072,1.00000116580347),(0.999655015039571,0.98136981804707,
1.00000126136715),(0.999620253220177,0.979492579632052,1.00000138846665),
(0.999586859443545,0.977689219468202,1.00000151056418),(0.999556749601363,
0.976063201227523,1.00000162065468),(0.999533861409886,0.974827172934429,
1.00000170434069),(0.9995106558406,0.973574005325064,1.00000178918712),
(0.999492456288907,0.97259117709081,1.00000185573007),(0.999482414904449,
0.972048913395374,1.00000189244434),(0.999481440401765,0.971996287442349,
1.00000189600741),(0.999482031626613,0.972028215287785,1.00000189384572)))
REPRESENTATION_ITEM('')
SURFACE()
);
#1716=(
BOUNDED_SURFACE()
B_SPLINE_SURFACE(3,2,((#52650,#52651,#52652),(#52653,#52654,#52655),(#52656,
#52657,#52658),(#52659,#52660,#52661),(#52662,#52663,#52664),(#52665,#52666,
#52667),(#52668,#52669,#52670),(#52671,#52672,#52673),(#52674,#52675,#52676)),
 .UNSPECIFIED.,.F.,.F.,.F.)
B_SPLINE_SURFACE_WITH_KNOTS((4,1,1,1,1,1,4),(3,3),(0.0199977630484638,0.0246245671030636,
0.026855473567606,0.0290863800321484,0.0313172864966908,0.0335481929612332,
0.0381749960364376),(0.,0.999290254333488),.UNSPECIFIED.)
GEOMETRIC_REPRESENTATION_ITEM()
RATIONAL_B_SPLINE_SURFACE(((1.,0.988770559028899,0.999984059905866),(1.,
0.986589245178597,0.999980963549762),(1.,0.984866673614857,0.999978518374356),
(1.,0.98480091247204,0.999978425026984),(1.,0.984960622739239,0.999978651734324),
(1.,0.984785723305408,0.999978403466094),(1.,0.984833323646006,0.999978471034365),
(1.,0.986526872930274,0.999980875012895),(1.,0.988716343491653,0.999983982947382)))
REPRESENTATION_ITEM('')
SURFACE()
);
#1717=(
BOUNDED_SURFACE()
B_SPLINE_SURFACE(3,2,((#52692,#52693,#52694),(#52695,#52696,#52697),(#52698,
#52699,#52700),(#52701,#52702,#52703),(#52704,#52705,#52706),(#52707,#52708,
#52709),(#52710,#52711,#52712),(#52713,#52714,#52715),(#52716,#52717,#52718),
(#52719,#52720,#52721),(#52722,#52723,#52724),(#52725,#52726,#52727),(#52728,
#52729,#52730),(#52731,#52732,#52733),(#52734,#52735,#52736),(#52737,#52738,
#52739),(#52740,#52741,#52742),(#52743,#52744,#52745),(#52746,#52747,#52748),
(#52749,#52750,#52751),(#52752,#52753,#52754),(#52755,#52756,#52757),(#52758,
#52759,#52760),(#52761,#52762,#52763),(#52764,#52765,#52766),(#52767,#52768,
#52769),(#52770,#52771,#52772),(#52773,#52774,#52775),(#52776,#52777,#52778),
(#52779,#52780,#52781),(#52782,#52783,#52784),(#52785,#52786,#52787),(#52788,
#52789,#52790),(#52791,#52792,#52793),(#52794,#52795,#52796),(#52797,#52798,
#52799),(#52800,#52801,#52802),(#52803,#52804,#52805),(#52806,#52807,#52808),
(#52809,#52810,#52811),(#52812,#52813,#52814),(#52815,#52816,#52817),(#52818,
#52819,#52820),(#52821,#52822,#52823),(#52824,#52825,#52826),(#52827,#52828,
#52829),(#52830,#52831,#52832),(#52833,#52834,#52835),(#52836,#52837,#52838),
(#52839,#52840,#52841),(#52842,#52843,#52844),(#52845,#52846,#52847),(#52848,
#52849,#52850),(#52851,#52852,#52853),(#52854,#52855,#52856)),
 .UNSPECIFIED.,.F.,.F.,.F.)
B_SPLINE_SURFACE_WITH_KNOTS((4,1,1,1,1,1,1,1,1,1,1,1,1,1,1,1,1,1,1,1,1,
1,1,1,1,1,1,1,1,1,1,1,1,1,1,1,1,1,1,1,1,1,1,1,1,1,1,1,1,1,1,1,4),(3,3),
(0.0486184959373272,0.0502403308116338,0.051051248248787,0.0518621656859403,
0.0526730831230936,0.0534840005602469,0.0538894592788235,0.0542949179974001,
0.0547003767159768,0.0551058354345534,0.0553085647938417,0.0555112941531301,
0.0557140235124184,0.0559167528717067,0.056119482230995,0.0562208469106392,
0.0563222115902833,0.0564869291947051,0.0564932644871829,0.0564995997796606,
0.0565059350721384,0.0565091027183773,0.0565122703646161,0.0565138541877356,
0.056515438010855,0.0565170218339745,0.0565186056570939,0.0565217733033328,
0.0565249409495717,0.0565376115345272,0.0565502821194827,0.0565629527044382,
0.0565756232893937,0.0566009644593048,0.0566263056292158,0.0566516467991268,
0.0566769879690379,0.05672767030886,0.0567783526486821,0.0568290349885041,
0.0569303996681483,0.0570317643477925,0.0571331290274366,0.0572344937070808,
0.0573358583867249,0.0575385877460133,0.0577413171053016,0.0579440464645899,
0.0583495051831665,0.0591604226203198,0.0599713400574731,0.0607822574946264,
0.0615931749317796),(0.,0.991165909752447),.UNSPECIFIED.)
GEOMETRIC_REPRESENTATION_ITEM()
RATIONAL_B_SPLINE_SURFACE(((1.,0.988579705956782,0.999798224183537),(1.,
0.988129226965691,0.999790265039413),(1.,0.987439893836455,0.999778085777264),
(1.,0.986625048090304,0.999763688935546),(1.,0.986111622194986,0.999754617634157),
(1.,0.9857486338806,0.999748204291101),(1.,0.985627260338365,0.999746059841449),
(1.,0.985683472003575,0.999747052999296),(1.,0.985816599097477,0.999749405112821),
(1.,0.986057632374737,0.999753663732267),(1.,0.98636574427647,0.99975910750896),
(1.,0.986689926424631,0.999764835217667),(1.,0.986975306492696,0.999769877364219),
(1.,0.987306481284958,0.999775728620225),(1.,0.987687389316159,0.999782458572072),
(1.,0.988049270371101,0.999788852351869),(1.,0.988366516495903,0.999794457513663),
(1.,0.988670704507122,0.99979983196235),(1.,0.988911877377787,0.999804093048157),
(1.,0.989074395964705,0.999806964455887),(1.,0.98909185437314,0.999807272914197),
(1.,0.989106320171297,0.99980752849853),(1.,0.989117495068773,0.999807725938636),
(1.,0.989127192857273,0.999807897280914),(1.,0.989121479139524,0.999807796329917),
(1.,0.989175325491616,0.999808747696985),(1.,0.989270871665965,0.999810435824039),
(1.,0.989370384575404,0.999812194036085),(1.,0.989462621663806,0.999813823697611),
(1.,0.989543515522181,0.999815252944901),(1.,0.989328957337217,0.999811462092163),
(1.,0.989016983430099,0.999805950080862),(1.,0.988696686701124,0.999800291020443),
(1.,0.988288392274654,0.999793077200821),(1.,0.987809951865198,0.99978462402931),
(1.,0.987281787718638,0.999775292329838),(1.,0.986791762419011,0.999766634474397),
(1.,0.986187018253921,0.999755949745335),(1.,0.985502666806469,0.999743858500439),
(1.,0.984765419501987,0.999730832681994),(1.,0.983869626093595,0.999715005642368),
(1.,0.982881120683453,0.999697540550362),(1.,0.981843977689429,0.999679216120743),
(1.,0.980929669268354,0.999663061954532),(1.,0.980110711771224,0.999648592465655),
(1.,0.979123821893318,0.999631155917163),(1.,0.978054517766649,0.999612263258849),
(1.,0.97696770723055,0.999593061294133),(1.,0.975726567304752,0.999571132609905),
(1.,0.973998108141452,0.999540593881429),(1.,0.972431575764954,0.99951291610465),
(1.,0.971422011780473,0.99949507894595),(1.,0.971014932146137,0.999487886589495),
(1.,0.971036354184058,0.999488265077928),(1.,0.971102653860526,0.999489436472578)))
REPRESENTATION_ITEM('')
SURFACE()
);
#1718=(
BOUNDED_SURFACE()
B_SPLINE_SURFACE(3,2,((#53134,#53135,#53136),(#53137,#53138,#53139),(#53140,
#53141,#53142),(#53143,#53144,#53145),(#53146,#53147,#53148),(#53149,#53150,
#53151),(#53152,#53153,#53154),(#53155,#53156,#53157),(#53158,#53159,#53160),
(#53161,#53162,#53163),(#53164,#53165,#53166),(#53167,#53168,#53169),(#53170,
#53171,#53172),(#53173,#53174,#53175)),.UNSPECIFIED.,.F.,.F.,.F.)
B_SPLINE_SURFACE_WITH_KNOTS((4,1,1,1,1,1,1,1,1,1,1,4),(3,3),(2.60208521396521E-18,
0.00224502843470091,0.00336754265205136,0.00449005686940182,0.00673508530410272,
0.00785759952145318,0.00898011373880363,0.0112251421735045,0.0134701706082054,
0.0157151990429064,0.0168377132602568,0.0179602274776073),(0.,1.),
 .UNSPECIFIED.)
GEOMETRIC_REPRESENTATION_ITEM()
RATIONAL_B_SPLINE_SURFACE(((1.,0.946871694682909,1.),(1.,0.946299968542447,
1.),(1.,0.946816109299184,1.),(1.,0.948892577451966,1.),(1.,0.949020476847393,
1.),(1.,0.94867679597236,1.),(1.,0.950073546741643,1.),(1.,0.9463002894051,
1.),(1.,0.930830476264166,1.),(1.,0.904147532449761,1.),(1.,0.881006864817563,
1.),(1.,0.861569290206786,1.),(1.,0.850439810109567,1.),(1.,0.84434427061595,
1.)))
REPRESENTATION_ITEM('')
SURFACE()
);
#1719=(
BOUNDED_SURFACE()
B_SPLINE_SURFACE(3,2,((#53231,#53232,#53233),(#53234,#53235,#53236),(#53237,
#53238,#53239),(#53240,#53241,#53242),(#53243,#53244,#53245),(#53246,#53247,
#53248),(#53249,#53250,#53251),(#53252,#53253,#53254),(#53255,#53256,#53257),
(#53258,#53259,#53260),(#53261,#53262,#53263),(#53264,#53265,#53266),(#53267,
#53268,#53269),(#53270,#53271,#53272),(#53273,#53274,#53275),(#53276,#53277,
#53278)),.UNSPECIFIED.,.F.,.F.,.F.)
B_SPLINE_SURFACE_WITH_KNOTS((4,1,1,1,1,1,1,1,1,1,1,1,1,4),(3,3),(-0.00203692429636695,
0.00254615537045871,0.00318269421307338,0.00381923305568806,0.00509231074091741,
0.00636538842614676,0.00700192726876144,0.00763846611137611,0.00891154379660546,
0.0101846214818348,0.0127307768522935,0.0152769322227522,0.0178230875932109,
0.0203692429636696),(-0.00168930119361338,1.00677133507503),
 .UNSPECIFIED.)
GEOMETRIC_REPRESENTATION_ITEM()
RATIONAL_B_SPLINE_SURFACE(((1.00008496330189,0.974681960965966,1.00034229172858),
(1.00010212847963,0.969566945066644,1.00041144509514),(1.00010690360001,
0.968144016797988,1.00043068262677),(1.00009873080779,0.970579410288973,
1.00039775689162),(1.00010107133118,0.969881962553438,1.00040718616024),
(1.00009941607801,0.970375208030169,1.00040051764035),(1.00009727006519,
0.971014693961847,1.00039187199664),(1.00009252792433,0.972427794734359,
1.00037276732959),(1.00009494037177,0.971708914498314,1.00038248635871),
(1.00009557216839,0.971520646726924,1.0003850316783),(1.00009294321431,
0.972304043329874,1.00037444040869),(1.00010749982106,0.96796635011755,
1.00043308462303),(1.00016473057531,0.950912275737492,1.00066365021269),
(1.0002312640321,0.931086108219379,1.00093169360822),(1.000274044616,0.918338010288713,
1.00110404378395),(1.00029567557767,0.911892244649696,1.00119118845814)))
REPRESENTATION_ITEM('')
SURFACE()
);
#1720=(
BOUNDED_SURFACE()
B_SPLINE_SURFACE(3,2,((#53459,#53460,#53461),(#53462,#53463,#53464),(#53465,
#53466,#53467),(#53468,#53469,#53470),(#53471,#53472,#53473),(#53474,#53475,
#53476),(#53477,#53478,#53479),(#53480,#53481,#53482),(#53483,#53484,#53485),
(#53486,#53487,#53488),(#53489,#53490,#53491),(#53492,#53493,#53494),(#53495,
#53496,#53497),(#53498,#53499,#53500),(#53501,#53502,#53503)),
 .UNSPECIFIED.,.F.,.F.,.F.)
B_SPLINE_SURFACE_WITH_KNOTS((4,1,1,1,1,1,1,1,1,1,1,1,4),(3,3),(-0.00112697568940802,
0.00227630595534438,0.00341445893301658,0.00398353542185268,0.00455261191068878,
0.00682891786603319,0.00796707084370539,0.00910522382137759,0.011381529776722,
0.0136578357320664,0.0159341416874108,0.017072294665083,0.0192306646931621),
(-0.0052660988655586,1.00285157929027),.UNSPECIFIED.)
GEOMETRIC_REPRESENTATION_ITEM()
RATIONAL_B_SPLINE_SURFACE(((1.00054177139849,0.948413008428147,1.00029266321785),
(1.00057240532917,0.945496072745762,1.00030921157155),(1.00056048610494,
0.946631010695459,1.00030277284384),(1.00054277515829,0.948317431311034,
1.00029320544576),(1.00052730480877,0.949790504257771,1.00028484841125),
(1.00054259713588,0.948334382447352,1.00029310927861),(1.00053010590215,
0.949523786632503,1.00028636155315),(1.00051694701969,0.950776763737995,
1.00027925316593),(1.00055340254948,0.947305500557184,1.0002989463293),
(1.00071450524393,0.931965445020424,1.00038597350182),(1.00099633115592,
0.905130231890504,1.0005382149795),(1.00124584768938,0.881371489098238,
1.0006730030318),(1.00149815795622,0.857346729494382,1.00080930025014),
(1.00167734639862,0.840284565094988,1.00090609728723),(1.00181930116002,
0.826767758744447,1.0009827808061)))
REPRESENTATION_ITEM('')
SURFACE()
);
#1721=(
BOUNDED_SURFACE()
B_SPLINE_SURFACE(3,2,((#53661,#53662,#53663),(#53664,#53665,#53666),(#53667,
#53668,#53669),(#53670,#53671,#53672)),.UNSPECIFIED.,.F.,.F.,.F.)
B_SPLINE_SURFACE_WITH_KNOTS((4,4),(3,3),(-2.25514051876985E-17,0.00236214428547912),
(-0.00620223654517092,1.),.UNSPECIFIED.)
GEOMETRIC_REPRESENTATION_ITEM()
RATIONAL_B_SPLINE_SURFACE(((1.00099729942381,0.919601629465039,1.),(1.00115637496513,
0.906777582835632,1.),(1.00126632012954,0.89791423462212,1.),(1.00133134190946,
0.892672433583815,1.)))
REPRESENTATION_ITEM('')
SURFACE()
);
#1722=(
BOUNDED_SURFACE()
B_SPLINE_SURFACE(3,2,((#53734,#53735,#53736),(#53737,#53738,#53739),(#53740,
#53741,#53742),(#53743,#53744,#53745),(#53746,#53747,#53748)),
 .UNSPECIFIED.,.F.,.F.,.F.)
B_SPLINE_SURFACE_WITH_KNOTS((4,1,4),(3,3),(3.14159265358979,3.92699081698724,
4.71238898038469),(0.,1.),.UNSPECIFIED.)
GEOMETRIC_REPRESENTATION_ITEM()
RATIONAL_B_SPLINE_SURFACE(((1.,0.48655776526455,1.),(1.,0.486557766002833,
1.),(1.,0.547974422145333,1.),(1.,0.658371714258051,1.),(1.,0.707106781186546,
1.)))
REPRESENTATION_ITEM('')
SURFACE()
);
#1723=(
BOUNDED_SURFACE()
B_SPLINE_SURFACE(3,2,((#53766,#53767,#53768),(#53769,#53770,#53771),(#53772,
#53773,#53774),(#53775,#53776,#53777)),.UNSPECIFIED.,.F.,.F.,.F.)
B_SPLINE_SURFACE_WITH_KNOTS((4,4),(3,3),(4.33680868994202E-19,0.0023350688542472),
(0.,1.00547355602571),.UNSPECIFIED.)
GEOMETRIC_REPRESENTATION_ITEM()
RATIONAL_B_SPLINE_SURFACE(((1.,0.921781046509973,1.0008562716484),(1.,0.909146339862613,
1.00099458519781),(1.,0.900351741222426,1.00109086065457),(1.,0.895068725056835,
1.0011486944245)))
REPRESENTATION_ITEM('')
SURFACE()
);
#1724=(
BOUNDED_SURFACE()
B_SPLINE_SURFACE(3,2,((#53836,#53837,#53838),(#53839,#53840,#53841),(#53842,
#53843,#53844),(#53845,#53846,#53847),(#53848,#53849,#53850)),
 .UNSPECIFIED.,.F.,.F.,.F.)
B_SPLINE_SURFACE_WITH_KNOTS((4,1,4),(3,3),(4.71238898038469,5.49778714378214,
6.28318530717959),(0.,1.),.UNSPECIFIED.)
GEOMETRIC_REPRESENTATION_ITEM()
RATIONAL_B_SPLINE_SURFACE(((1.,0.707106781186548,1.),(1.,0.658371714258676,
1.),(1.,0.547974422145018,1.),(1.,0.486557766002833,1.),(1.,0.48655776526455,
1.)))
REPRESENTATION_ITEM('')
SURFACE()
);
#1725=(
BOUNDED_SURFACE()
B_SPLINE_SURFACE(3,2,((#53860,#53861,#53862),(#53863,#53864,#53865),(#53866,
#53867,#53868),(#53869,#53870,#53871)),.UNSPECIFIED.,.F.,.F.,.F.)
B_SPLINE_SURFACE_WITH_KNOTS((4,4),(3,3),(2.5804011705155E-17,0.00269592513607839),
(0.,1.),.UNSPECIFIED.)
GEOMETRIC_REPRESENTATION_ITEM()
RATIONAL_B_SPLINE_SURFACE(((1.,0.887940178746615,1.),(1.,0.872219487795338,
1.),(1.,0.861659279393505,1.),(1.,0.854938173458171,1.)))
REPRESENTATION_ITEM('')
SURFACE()
);
#1726=(
BOUNDED_SURFACE()
B_SPLINE_SURFACE(3,2,((#53930,#53931,#53932),(#53933,#53934,#53935),(#53936,
#53937,#53938),(#53939,#53940,#53941),(#53942,#53943,#53944)),
 .UNSPECIFIED.,.F.,.F.,.F.)
B_SPLINE_SURFACE_WITH_KNOTS((4,1,4),(3,3),(-0.000302909321607987,0.00578886195052519,
0.0118806332226584),(0.,1.03312425876202),.UNSPECIFIED.)
GEOMETRIC_REPRESENTATION_ITEM()
RATIONAL_B_SPLINE_SURFACE(((1.,0.894876494760464,1.00696427637905),(1.,
0.874392201020365,1.00832133047186),(1.,0.77515446292856,1.01489568350288),
(1.,0.867433891531754,1.00878230815995),(0.999999999999999,0.887390355972598,
1.00746022197573)))
REPRESENTATION_ITEM('')
SURFACE()
);
#1727=(
BOUNDED_SURFACE()
B_SPLINE_SURFACE(3,2,((#53952,#53953,#53954),(#53955,#53956,#53957),(#53958,
#53959,#53960),(#53961,#53962,#53963),(#53964,#53965,#53966)),
 .UNSPECIFIED.,.F.,.F.,.F.)
B_SPLINE_SURFACE_WITH_KNOTS((4,1,4),(3,3),(-0.00116263837286272,0.0058131918643132,
0.0127890221014908),(-0.020297547916368,1.),.UNSPECIFIED.)
GEOMETRIC_REPRESENTATION_ITEM()
RATIONAL_B_SPLINE_SURFACE(((1.0039429407102,0.902871501364518,0.999999999999999),
(1.00444247717786,0.890566161090803,1.),(1.00958527090562,0.763881062256417,
1.),(1.00474383084143,0.883142760372419,1.),(1.00423046655648,0.89578872842398,
0.999999999999999)))
REPRESENTATION_ITEM('')
SURFACE()
);
#1728=(
BOUNDED_SURFACE()
B_SPLINE_SURFACE(3,2,((#53970,#53971,#53972),(#53973,#53974,#53975),(#53976,
#53977,#53978),(#53979,#53980,#53981)),.UNSPECIFIED.,.F.,.F.,.F.)
B_SPLINE_SURFACE_WITH_KNOTS((4,4),(3,3),(-1.68094704822153E-15,0.00269464124111705),
(0.,1.),.UNSPECIFIED.)
GEOMETRIC_REPRESENTATION_ITEM()
RATIONAL_B_SPLINE_SURFACE(((1.,0.888319363951509,1.),(1.,0.87265918860752,
1.),(1.,0.862124260711793,1.),(1.,0.855384875699737,1.)))
REPRESENTATION_ITEM('')
SURFACE()
);
#1729=(
BOUNDED_SURFACE()
B_SPLINE_SURFACE(3,2,((#54121,#54122,#54123),(#54124,#54125,#54126),(#54127,
#54128,#54129),(#54130,#54131,#54132)),.UNSPECIFIED.,.F.,.F.,.F.)
B_SPLINE_SURFACE_WITH_KNOTS((4,4),(3,3),(0.000203890603018781,0.000876640979146271),
(0.,1.00234872771707),.UNSPECIFIED.)
GEOMETRIC_REPRESENTATION_ITEM()
RATIONAL_B_SPLINE_SURFACE(((1.,0.706418854765374,1.00137908434605),(1.,
0.794166685486793,1.00096689282179),(1.,0.870219940196321,1.00060963604717),
(1.,0.870219885219157,1.00060963630542)))
REPRESENTATION_ITEM('')
SURFACE()
);
#1730=(
BOUNDED_SURFACE()
B_SPLINE_SURFACE(3,2,((#54135,#54136,#54137),(#54138,#54139,#54140),(#54141,
#54142,#54143),(#54144,#54145,#54146),(#54147,#54148,#54149),(#54150,#54151,
#54152),(#54153,#54154,#54155),(#54156,#54157,#54158),(#54159,#54160,#54161),
(#54162,#54163,#54164),(#54165,#54166,#54167)),.UNSPECIFIED.,.T.,.F.,.F.)
B_SPLINE_SURFACE_WITH_KNOTS((4,1,1,1,1,1,1,1,4),(3,3),(0.,0.00130817098982512,
0.00261634197965024,0.00392451296947536,0.00523268395930048,0.0065408549491256,
0.00784902593895073,0.00915719692877585,0.010465367918601),(-9.28189933859035E-5,
1.00709936745473),.UNSPECIFIED.)
GEOMETRIC_REPRESENTATION_ITEM()
RATIONAL_B_SPLINE_SURFACE(((1.00005816990851,0.684423875675114,1.00448036293871),
(1.0000582548459,0.683963083962243,1.00448690498659),(1.00005264871468,
0.71437676702377,1.00405510952452),(1.00004410969851,0.760701571367001,
1.00339741738458),(1.00005214672296,0.717100109865461,1.00401644511554),
(1.000061052267,0.668786864287407,1.00470236796664),(1.00005266324573,0.714297935019167,
1.00405622873464),(1.00004410774396,0.760712174947296,1.00339726684123),
(1.00005213909035,0.717141517300991,1.00401585723729),(1.00005808497112,
0.684884667387984,1.00447382089084),(1.00005816990851,0.684423875675114,
1.00448036293871)))
REPRESENTATION_ITEM('')
SURFACE()
);
#1731=(
BOUNDED_SURFACE()
B_SPLINE_SURFACE(3,2,((#54168,#54169,#54170),(#54171,#54172,#54173),(#54174,
#54175,#54176),(#54177,#54178,#54179),(#54180,#54181,#54182),(#54183,#54184,
#54185),(#54186,#54187,#54188),(#54189,#54190,#54191),(#54192,#54193,#54194),
(#54195,#54196,#54197),(#54198,#54199,#54200)),.UNSPECIFIED.,.T.,.F.,.F.)
B_SPLINE_SURFACE_WITH_KNOTS((4,1,1,1,1,1,1,1,4),(3,3),(0.,0.00130817098982513,
0.00261634197965027,0.0039245129694754,0.00523268395930054,0.00654085494912567,
0.0078490259389508,0.00915719692877594,0.0104653679186011),(-9.28189933908896E-5,
1.00709936745538),.UNSPECIFIED.)
GEOMETRIC_REPRESENTATION_ITEM()
RATIONAL_B_SPLINE_SURFACE(((1.00005816990851,0.684423875674909,1.00448036293913),
(1.0000582548459,0.683963083962039,1.004486904987),(1.00005264871469,0.714376767023586,
1.0040551095249),(1.00004410969851,0.760701571366847,1.00339741738489),
(1.00005214672296,0.717100109865272,1.00401644511591),(1.000061052267,0.668786864287198,
1.00470236796707),(1.00005266324573,0.714297935018957,1.00405622873502),
(1.00004410774396,0.760712174947142,1.00339726684154),(1.00005213909036,
0.717141517300806,1.00401585723766),(1.00005808497112,0.68488466738778,
1.00447382089125),(1.00005816990851,0.684423875674909,1.00448036293913)))
REPRESENTATION_ITEM('')
SURFACE()
);
#1732=(
BOUNDED_SURFACE()
B_SPLINE_SURFACE(3,2,((#54201,#54202,#54203),(#54204,#54205,#54206),(#54207,
#54208,#54209),(#54210,#54211,#54212),(#54213,#54214,#54215),(#54216,#54217,
#54218),(#54219,#54220,#54221),(#54222,#54223,#54224),(#54225,#54226,#54227),
(#54228,#54229,#54230),(#54231,#54232,#54233)),.UNSPECIFIED.,.T.,.F.,.F.)
B_SPLINE_SURFACE_WITH_KNOTS((4,1,1,1,1,1,1,1,4),(3,3),(0.,0.00130817098982513,
0.00261634197965025,0.00392451296947538,0.00523268395930051,0.00654085494912563,
0.00784902593895076,0.00915719692877589,0.010465367918601),(-9.28189933861358E-5,
1.00709936745573),.UNSPECIFIED.)
GEOMETRIC_REPRESENTATION_ITEM()
RATIONAL_B_SPLINE_SURFACE(((1.00005816990851,0.6844238756748,1.00448036293935),
(1.0000582548459,0.683963083961927,1.00448690498722),(1.00005264871468,
0.714376767023479,1.0040551095251),(1.00004410969851,0.760701571366764,
1.00339741738506),(1.00005214672296,0.717100109865185,1.00401644511611),
(1.000061052267,0.668786864287076,1.00470236796731),(1.00005266324573,0.714297935018881,
1.00405622873522),(1.00004410774396,0.760712174947052,1.00339726684171),
(1.00005213909035,0.717141517300717,1.00401585723786),(1.00005808497112,
0.684884667387673,1.00447382089148),(1.00005816990851,0.6844238756748,1.00448036293935)))
REPRESENTATION_ITEM('')
SURFACE()
);
#1733=(
BOUNDED_SURFACE()
B_SPLINE_SURFACE(3,2,((#54234,#54235,#54236),(#54237,#54238,#54239),(#54240,
#54241,#54242),(#54243,#54244,#54245),(#54246,#54247,#54248),(#54249,#54250,
#54251),(#54252,#54253,#54254),(#54255,#54256,#54257),(#54258,#54259,#54260),
(#54261,#54262,#54263),(#54264,#54265,#54266)),.UNSPECIFIED.,.T.,.F.,.F.)
B_SPLINE_SURFACE_WITH_KNOTS((4,1,1,1,1,1,1,1,4),(3,3),(0.,0.00130817098982513,
0.00261634197965025,0.00392451296947538,0.00523268395930051,0.00654085494912563,
0.00784902593895076,0.00915719692877589,0.010465367918601),(-9.28189933903628E-5,
1.0070993674559),.UNSPECIFIED.)
GEOMETRIC_REPRESENTATION_ITEM()
RATIONAL_B_SPLINE_SURFACE(((1.00005816990851,0.684423875674746,1.00448036293946),
(1.0000582548459,0.683963083961873,1.00448690498733),(1.00005264871469,
0.714376767023432,1.0040551095252),(1.00004410969851,0.760701571366722,
1.00339741738514),(1.00005214672296,0.717100109865137,1.00401644511621),
(1.000061052267,0.668786864287018,1.00470236796742),(1.00005266324573,0.714297935018832,
1.00405622873532),(1.00004410774396,0.760712174947011,1.00339726684179),
(1.00005213909036,0.717141517300666,1.00401585723796),(1.00005808497112,
0.684884667387618,1.00447382089158),(1.00005816990851,0.684423875674746,
1.00448036293946)))
REPRESENTATION_ITEM('')
SURFACE()
);
#1734=(
BOUNDED_SURFACE()
B_SPLINE_SURFACE(3,2,((#54267,#54268,#54269),(#54270,#54271,#54272),(#54273,
#54274,#54275),(#54276,#54277,#54278),(#54279,#54280,#54281),(#54282,#54283,
#54284),(#54285,#54286,#54287),(#54288,#54289,#54290),(#54291,#54292,#54293),
(#54294,#54295,#54296),(#54297,#54298,#54299)),.UNSPECIFIED.,.T.,.F.,.F.)
B_SPLINE_SURFACE_WITH_KNOTS((4,1,1,1,1,1,1,1,4),(3,3),(0.,0.00130817098982512,
0.00261634197965025,0.00392451296947537,0.00523268395930049,0.00654085494912562,
0.00784902593895074,0.00915719692877586,0.010465367918601),(-9.28189933853903E-5,
1.00709936745582),.UNSPECIFIED.)
GEOMETRIC_REPRESENTATION_ITEM()
RATIONAL_B_SPLINE_SURFACE(((1.00005816990851,0.684423875674772,1.00448036293941),
(1.0000582548459,0.683963083961899,1.00448690498728),(1.00005264871468,
0.714376767023455,1.00405510952515),(1.00004410969851,0.760701571366749,
1.00339741738511),(1.00005214672296,0.717100109865145,1.00401644511616),
(1.000061052267,0.66878686428705,1.00470236796737),(1.00005266324573,0.714297935018859,
1.00405622873527),(1.00004410774396,0.760712174947014,1.00339726684175),
(1.00005213909035,0.717141517300695,1.00401585723791),(1.00005808497112,
0.684884667387646,1.00447382089153),(1.00005816990851,0.684423875674772,
1.00448036293941)))
REPRESENTATION_ITEM('')
SURFACE()
);
#1735=(
BOUNDED_SURFACE()
B_SPLINE_SURFACE(3,2,((#54302,#54303,#54304),(#54305,#54306,#54307),(#54308,
#54309,#54310),(#54311,#54312,#54313),(#54314,#54315,#54316),(#54317,#54318,
#54319),(#54320,#54321,#54322),(#54323,#54324,#54325)),.UNSPECIFIED.,.F.,
 .F.,.F.)
B_SPLINE_SURFACE_WITH_KNOTS((4,1,1,1,1,4),(3,3),(-1.90819582357449E-17,
0.000564455951974709,0.00112891190394944,0.00169336785592416,0.00197559583191153,
0.00225782380789889),(0.,1.),.UNSPECIFIED.)
GEOMETRIC_REPRESENTATION_ITEM()
RATIONAL_B_SPLINE_SURFACE(((1.,0.991835613598268,1.),(1.,0.992614005712327,
1.),(1.,0.994141544760846,1.),(1.,0.99631583526732,1.),(1.,0.998003041423521,
1.),(1.,0.999172568373962,1.),(1.,0.999639015745245,1.),(1.,0.999648793303385,
1.)))
REPRESENTATION_ITEM('')
SURFACE()
);
#1736=(
BOUNDED_SURFACE()
B_SPLINE_SURFACE(3,2,((#54327,#54328,#54329),(#54330,#54331,#54332),(#54333,
#54334,#54335),(#54336,#54337,#54338),(#54339,#54340,#54341),(#54342,#54343,
#54344),(#54345,#54346,#54347)),.UNSPECIFIED.,.F.,.F.,.F.)
B_SPLINE_SURFACE_WITH_KNOTS((4,1,1,1,4),(3,3),(-0.000237302740885216,0.000593256852870235,
0.00118651370574085,0.00177977055861147,0.00261032859115487),(0.,1.01493592684462),
 .UNSPECIFIED.)
GEOMETRIC_REPRESENTATION_ITEM()
RATIONAL_B_SPLINE_SURFACE(((1.,0.999079384901643,1.00002750047952),(1.,
0.999827499951708,1.0000051528962),(1.,0.998481551946456,1.00004535885809),
(1.,0.996274060209497,1.00011130072828),(1.,0.993792671277815,1.00018542441539),
(1.,0.99189007799518,1.00024225840356),(1.,0.990734532561305,1.00027677668769)))
REPRESENTATION_ITEM('')
SURFACE()
);
#1737=(
BOUNDED_SURFACE()
B_SPLINE_SURFACE(3,2,((#54353,#54354,#54355),(#54356,#54357,#54358),(#54359,
#54360,#54361),(#54362,#54363,#54364),(#54365,#54366,#54367),(#54368,#54369,
#54370),(#54371,#54372,#54373),(#54374,#54375,#54376)),.UNSPECIFIED.,.F.,
 .F.,.F.)
B_SPLINE_SURFACE_WITH_KNOTS((4,1,1,1,1,4),(3,3),(-0.00022248774067706,0.000871734875690068,
0.00174346975138016,0.00261520462707025,0.0030510720649153,0.00370942724411761),
(0.,1.00163938212957),.UNSPECIFIED.)
GEOMETRIC_REPRESENTATION_ITEM()
RATIONAL_B_SPLINE_SURFACE(((1.,0.984069198332286,1.00005223334313),(1.,
0.986023953875702,1.00004582416052),(1.,0.9893454078424,1.00003493389596),
(1.,0.993616993324213,1.00002092837415),(1.,0.996528307451787,1.00001138286145),
(1.,0.998741040052508,1.00000412783288),(1.,0.999581963593584,1.00000137064283),
(1.,0.999053363005491,1.00000310379954)))
REPRESENTATION_ITEM('')
SURFACE()
);
#1738=(
BOUNDED_SURFACE()
B_SPLINE_SURFACE(3,2,((#54378,#54379,#54380),(#54381,#54382,#54383),(#54384,
#54385,#54386),(#54387,#54388,#54389),(#54390,#54391,#54392),(#54393,#54394,
#54395),(#54396,#54397,#54398),(#54399,#54400,#54401)),.UNSPECIFIED.,.F.,
 .F.,.F.)
B_SPLINE_SURFACE_WITH_KNOTS((4,1,1,1,1,4),(3,3),(-0.000293385255678526,
0.000366731569601773,0.000733463139204117,0.0014669262784088,0.00220038941761349,
0.00322723781250381),(-0.0485261900086986,1.),.UNSPECIFIED.)
GEOMETRIC_REPRESENTATION_ITEM()
RATIONAL_B_SPLINE_SURFACE(((1.00012540024569,0.998707911689922,1.),(0.999997586898636,
1.00002486390713,1.),(1.00010833407507,0.998883756636833,1.),(1.00035522793121,
0.99633983287021,1.),(1.00065835344187,0.993216514198341,1.),(1.00111105184117,
0.988552039208393,1.),(1.00146600902586,0.984894661773356,1.),(1.00168082818161,
0.982681226557189,1.)))
REPRESENTATION_ITEM('')
SURFACE()
);
#1739=(
BOUNDED_SURFACE()
B_SPLINE_SURFACE(3,2,((#54406,#54407,#54408),(#54409,#54410,#54411),(#54412,
#54413,#54414),(#54415,#54416,#54417),(#54418,#54419,#54420),(#54421,#54422,
#54423),(#54424,#54425,#54426),(#54427,#54428,#54429)),.UNSPECIFIED.,.F.,
 .F.,.F.)
B_SPLINE_SURFACE_WITH_KNOTS((4,1,1,1,1,4),(3,3),(-0.000291172064625148,
0.000727930161563534,0.00145586032312702,0.00218379048469051,0.00254775556547226,
0.00320288287705394),(-0.00425992492820294,1.00188056036606),
 .UNSPECIFIED.)
GEOMETRIC_REPRESENTATION_ITEM()
RATIONAL_B_SPLINE_SURFACE(((1.00014547214641,0.982893257690745,1.00006406708988),
(1.00012675132083,0.985094726129536,1.00005582228945),(1.00009615646836,
0.988692516292073,1.00004234807317),(1.00005704155094,0.993292220284361,
1.00002512155255),(1.00003091594257,0.996364451368782,1.00001361562691),
(1.00000928508564,0.99890812384817,1.00000408922554),(0.99999986210703,
1.00001621547194,0.99999993927084),(1.00001068993421,0.998742921209425,
1.00000470793202)))
REPRESENTATION_ITEM('')
SURFACE()
);
#1740=(
BOUNDED_SURFACE()
B_SPLINE_SURFACE(3,2,((#54431,#54432,#54433),(#54434,#54435,#54436),(#54437,
#54438,#54439),(#54440,#54441,#54442),(#54443,#54444,#54445),(#54446,#54447,
#54448),(#54449,#54450,#54451),(#54452,#54453,#54454)),.UNSPECIFIED.,.F.,
 .F.,.F.)
B_SPLINE_SURFACE_WITH_KNOTS((4,1,1,1,1,4),(3,3),(-0.000348982146594615,
0.000436227682637781,0.000872455365275428,0.00174491073055072,0.00261736609582601,
0.00383880360636252),(0.,1.00191159842478),.UNSPECIFIED.)
GEOMETRIC_REPRESENTATION_ITEM()
RATIONAL_B_SPLINE_SURFACE(((1.,0.998610437460761,1.00000531257112),(1.,
0.999703499185041,1.00000113358098),(1.,0.998779073849389,1.00000466784101),
(1.,0.996351424872412,1.00001394922093),(1.,0.993352180114163,1.00002541592404),
(1.,0.988814006533964,1.00004276625498),(1.,0.985173580066159,1.00005668432198),
(1.,0.982918980573743,1.00006530409966)))
REPRESENTATION_ITEM('')
SURFACE()
);
#1741=(
BOUNDED_SURFACE()
B_SPLINE_SURFACE(3,2,((#54462,#54463,#54464),(#54465,#54466,#54467),(#54468,
#54469,#54470),(#54471,#54472,#54473),(#54474,#54475,#54476),(#54477,#54478,
#54479),(#54480,#54481,#54482)),.UNSPECIFIED.,.F.,.F.,.F.)
B_SPLINE_SURFACE_WITH_KNOTS((4,1,1,1,4),(3,3),(-0.000234670538907357,0.000586676321783697,
0.00117335264356738,0.00176002896535107,0.00258134363634634),(0.,1.01053582586227),
 .UNSPECIFIED.)
GEOMETRIC_REPRESENTATION_ITEM()
RATIONAL_B_SPLINE_SURFACE(((1.,0.990705352673112,1.00019585357137),(1.,
0.991867802793339,1.00017135882729),(1.,0.993772696303182,1.00013121957468),
(1.,0.99626757911702,1.00007864827294),(1.,0.998507262784341,1.00003145443872),
(1.,0.999812010880492,1.00000396124125),(1.,0.999030864962552,1.00002042127598)))
REPRESENTATION_ITEM('')
SURFACE()
);
#1742=(
BOUNDED_SURFACE()
B_SPLINE_SURFACE(3,2,((#54484,#54485,#54486),(#54487,#54488,#54489),(#54490,
#54491,#54492),(#54493,#54494,#54495),(#54496,#54497,#54498),(#54499,#54500,
#54501),(#54502,#54503,#54504),(#54505,#54506,#54507)),.UNSPECIFIED.,.F.,
 .F.,.F.)
B_SPLINE_SURFACE_WITH_KNOTS((4,1,1,1,1,4),(3,3),(-0.000226104302166867,
0.000282630377695824,0.000565260755392034,0.00113052151078445,0.00169578226617687,
0.00248714732372626),(-0.0106186671104657,1.),.UNSPECIFIED.)
GEOMETRIC_REPRESENTATION_ITEM()
RATIONAL_B_SPLINE_SURFACE(((1.00001672252316,0.999212588407443,0.999999999999999),
(1.00000032168945,0.999984852644386,1.),(1.00001379719143,0.999350333178205,
1.),(1.00004410049111,0.997923445068481,1.),(1.00008037719364,0.99621528800171,
1.),(1.00013303469651,0.993735810006735,1.),(1.00017300194076,0.991853876811405,
1.),(1.00019675009217,0.990735650241147,1.)))
REPRESENTATION_ITEM('')
SURFACE()
);
#1743=SHAPE_REPRESENTATION_RELATIONSHIP('SRR','None',#54630,#1757);
#1744=SHAPE_REPRESENTATION_RELATIONSHIP('SRR','None',#54631,#1758);
#1745=SHAPE_REPRESENTATION_RELATIONSHIP('SRR','None',#54632,#1759);
#1746=SHAPE_REPRESENTATION_RELATIONSHIP('SRR','None',#54633,#1760);
#1747=SHAPE_REPRESENTATION_RELATIONSHIP('SRR','None',#54634,#1761);
#1748=SHAPE_REPRESENTATION_RELATIONSHIP('SRR','None',#54635,#1762);
#1749=SHAPE_REPRESENTATION_RELATIONSHIP('SRR','None',#54636,#1763);
#1750=SHAPE_REPRESENTATION_RELATIONSHIP('SRR','None',#54637,#1764);
#1751=SHAPE_REPRESENTATION_RELATIONSHIP('SRR','None',#54638,#1765);
#1752=SHAPE_REPRESENTATION_RELATIONSHIP('SRR','None',#54639,#1766);
#1753=SHAPE_REPRESENTATION_RELATIONSHIP('SRR','None',#54640,#1767);
#1754=SHAPE_REPRESENTATION_RELATIONSHIP('SRR','None',#54641,#1768);
#1755=SHAPE_REPRESENTATION_RELATIONSHIP('SRR','None',#54642,#1769);
#1756=SHAPE_REPRESENTATION_RELATIONSHIP('SRR','None',#54643,#1770);
#1757=ADVANCED_BREP_SHAPE_REPRESENTATION('',(#1801),#54566);
#1758=ADVANCED_BREP_SHAPE_REPRESENTATION('',(#1802),#54567);
#1759=ADVANCED_BREP_SHAPE_REPRESENTATION('',(#1803),#54568);
#1760=ADVANCED_BREP_SHAPE_REPRESENTATION('',(#1804),#54569);
#1761=ADVANCED_BREP_SHAPE_REPRESENTATION('',(#1805),#54570);
#1762=ADVANCED_BREP_SHAPE_REPRESENTATION('',(#1806),#54571);
#1763=ADVANCED_BREP_SHAPE_REPRESENTATION('',(#1807),#54572);
#1764=ADVANCED_BREP_SHAPE_REPRESENTATION('',(#1808),#54573);
#1765=ADVANCED_BREP_SHAPE_REPRESENTATION('',(#1809),#54574);
#1766=ADVANCED_BREP_SHAPE_REPRESENTATION('',(#1810),#54575);
#1767=ADVANCED_BREP_SHAPE_REPRESENTATION('',(#1811),#54576);
#1768=ADVANCED_BREP_SHAPE_REPRESENTATION('',(#1812),#54577);
#1769=ADVANCED_BREP_SHAPE_REPRESENTATION('',(#1813),#54578);
#1770=ADVANCED_BREP_SHAPE_REPRESENTATION('',(#1814),#54579);
#1771=STYLED_ITEM('',(#54709),#1801);
#1772=STYLED_ITEM('',(#54712),#16847);
#1773=STYLED_ITEM('',(#54712),#16848);
#1774=STYLED_ITEM('',(#54711),#16850);
#1775=STYLED_ITEM('',(#54712),#16868);
#1776=STYLED_ITEM('',(#54712),#16869);
#1777=STYLED_ITEM('',(#54712),#16871);
#1778=STYLED_ITEM('',(#54712),#16872);
#1779=STYLED_ITEM('',(#54712),#16873);
#1780=STYLED_ITEM('',(#54712),#16874);
#1781=STYLED_ITEM('',(#54712),#16875);
#1782=STYLED_ITEM('',(#54712),#16876);
#1783=STYLED_ITEM('',(#54712),#16895);
#1784=STYLED_ITEM('',(#54710),#1802);
#1785=STYLED_ITEM('',(#54713),#1803);
#1786=STYLED_ITEM('',(#54714),#1804);
#1787=STYLED_ITEM('',(#54715),#17257);
#1788=STYLED_ITEM('',(#54713),#17258);
#1789=STYLED_ITEM('',(#54713),#17272);
#1790=STYLED_ITEM('',(#54713),#17284);
#1791=STYLED_ITEM('',(#54709),#1805);
#1792=STYLED_ITEM('',(#54716),#1806);
#1793=STYLED_ITEM('',(#54717),#1807);
#1794=STYLED_ITEM('',(#54712),#1808);
#1795=STYLED_ITEM('',(#54709),#1809);
#1796=STYLED_ITEM('',(#54716),#1810);
#1797=STYLED_ITEM('',(#54712),#1811);
#1798=STYLED_ITEM('',(#54712),#1812);
#1799=STYLED_ITEM('',(#54710),#1813);
#1800=STYLED_ITEM('',(#54716),#1814);
#1801=MANIFOLD_SOLID_BREP('Body1',#17666);
#1802=MANIFOLD_SOLID_BREP('Body1',#17667);
#1803=MANIFOLD_SOLID_BREP('Body1',#17668);
#1804=MANIFOLD_SOLID_BREP('Body1',#17669);
#1805=MANIFOLD_SOLID_BREP('Body1',#17670);
#1806=MANIFOLD_SOLID_BREP('Body1',#17671);
#1807=MANIFOLD_SOLID_BREP('Body1',#17672);
#1808=MANIFOLD_SOLID_BREP('Body1',#17673);
#1809=MANIFOLD_SOLID_BREP('Body1',#17674);
#1810=MANIFOLD_SOLID_BREP('Body1',#17675);
#1811=MANIFOLD_SOLID_BREP('Body1',#17676);
#1812=MANIFOLD_SOLID_BREP('Body1',#17677);
#1813=MANIFOLD_SOLID_BREP('Body1',#17678);
#1814=MANIFOLD_SOLID_BREP('Body1',#17679);
#1815=LINE('',#24101,#2408);
#1816=LINE('',#24103,#2409);
#1817=LINE('',#24107,#2410);
#1818=LINE('',#24110,#2411);
#1819=LINE('',#24113,#2412);
#1820=LINE('',#24115,#2413);
#1821=LINE('',#24119,#2414);
#1822=LINE('',#24121,#2415);
#1823=LINE('',#24125,#2416);
#1824=LINE('',#24127,#2417);
#1825=LINE('',#24131,#2418);
#1826=LINE('',#24134,#2419);
#1827=LINE('',#24137,#2420);
#1828=LINE('',#24140,#2421);
#1829=LINE('',#24143,#2422);
#1830=LINE('',#24145,#2423);
#1831=LINE('',#24149,#2424);
#1832=LINE('',#24152,#2425);
#1833=LINE('',#24155,#2426);
#1834=LINE('',#24157,#2427);
#1835=LINE('',#24161,#2428);
#1836=LINE('',#24163,#2429);
#1837=LINE('',#24167,#2430);
#1838=LINE('',#24169,#2431);
#1839=LINE('',#24173,#2432);
#1840=LINE('',#24175,#2433);
#1841=LINE('',#24179,#2434);
#1842=LINE('',#24182,#2435);
#1843=LINE('',#24185,#2436);
#1844=LINE('',#24187,#2437);
#1845=LINE('',#24191,#2438);
#1846=LINE('',#24193,#2439);
#1847=LINE('',#24197,#2440);
#1848=LINE('',#24199,#2441);
#1849=LINE('',#24203,#2442);
#1850=LINE('',#24206,#2443);
#1851=LINE('',#24209,#2444);
#1852=LINE('',#24212,#2445);
#1853=LINE('',#24215,#2446);
#1854=LINE('',#24217,#2447);
#1855=LINE('',#24221,#2448);
#1856=LINE('',#24224,#2449);
#1857=LINE('',#24227,#2450);
#1858=LINE('',#24229,#2451);
#1859=LINE('',#24233,#2452);
#1860=LINE('',#24235,#2453);
#1861=LINE('',#24239,#2454);
#1862=LINE('',#24241,#2455);
#1863=LINE('',#24245,#2456);
#1864=LINE('',#24248,#2457);
#1865=LINE('',#24251,#2458);
#1866=LINE('',#24253,#2459);
#1867=LINE('',#24257,#2460);
#1868=LINE('',#24259,#2461);
#1869=LINE('',#24263,#2462);
#1870=LINE('',#24265,#2463);
#1871=LINE('',#24269,#2464);
#1872=LINE('',#24272,#2465);
#1873=LINE('',#24275,#2466);
#1874=LINE('',#24277,#2467);
#1875=LINE('',#24281,#2468);
#1876=LINE('',#24283,#2469);
#1877=LINE('',#24287,#2470);
#1878=LINE('',#24290,#2471);
#1879=LINE('',#24293,#2472);
#1880=LINE('',#24295,#2473);
#1881=LINE('',#24299,#2474);
#1882=LINE('',#24301,#2475);
#1883=LINE('',#24305,#2476);
#1884=LINE('',#24307,#2477);
#1885=LINE('',#24311,#2478);
#1886=LINE('',#24314,#2479);
#1887=LINE('',#24317,#2480);
#1888=LINE('',#24319,#2481);
#1889=LINE('',#24323,#2482);
#1890=LINE('',#24325,#2483);
#1891=LINE('',#24329,#2484);
#1892=LINE('',#24331,#2485);
#1893=LINE('',#24335,#2486);
#1894=LINE('',#24338,#2487);
#1895=LINE('',#24341,#2488);
#1896=LINE('',#24343,#2489);
#1897=LINE('',#24347,#2490);
#1898=LINE('',#24349,#2491);
#1899=LINE('',#24353,#2492);
#1900=LINE('',#24356,#2493);
#1901=LINE('',#24359,#2494);
#1902=LINE('',#24361,#2495);
#1903=LINE('',#24365,#2496);
#1904=LINE('',#24367,#2497);
#1905=LINE('',#24606,#2498);
#1906=LINE('',#24607,#2499);
#1907=LINE('',#24609,#2500);
#1908=LINE('',#24611,#2501);
#1909=LINE('',#24614,#2502);
#1910=LINE('',#24616,#2503);
#1911=LINE('',#24619,#2504);
#1912=LINE('',#24621,#2505);
#1913=LINE('',#24624,#2506);
#1914=LINE('',#24626,#2507);
#1915=LINE('',#24629,#2508);
#1916=LINE('',#24631,#2509);
#1917=LINE('',#24634,#2510);
#1918=LINE('',#24636,#2511);
#1919=LINE('',#24639,#2512);
#1920=LINE('',#24641,#2513);
#1921=LINE('',#24644,#2514);
#1922=LINE('',#24646,#2515);
#1923=LINE('',#24649,#2516);
#1924=LINE('',#24651,#2517);
#1925=LINE('',#24654,#2518);
#1926=LINE('',#24656,#2519);
#1927=LINE('',#24659,#2520);
#1928=LINE('',#24661,#2521);
#1929=LINE('',#24664,#2522);
#1930=LINE('',#24666,#2523);
#1931=LINE('',#24669,#2524);
#1932=LINE('',#24671,#2525);
#1933=LINE('',#24674,#2526);
#1934=LINE('',#24676,#2527);
#1935=LINE('',#24679,#2528);
#1936=LINE('',#24681,#2529);
#1937=LINE('',#24684,#2530);
#1938=LINE('',#24686,#2531);
#1939=LINE('',#24689,#2532);
#1940=LINE('',#24691,#2533);
#1941=LINE('',#24694,#2534);
#1942=LINE('',#24696,#2535);
#1943=LINE('',#24699,#2536);
#1944=LINE('',#24701,#2537);
#1945=LINE('',#24704,#2538);
#1946=LINE('',#24706,#2539);
#1947=LINE('',#24709,#2540);
#1948=LINE('',#24711,#2541);
#1949=LINE('',#24714,#2542);
#1950=LINE('',#24716,#2543);
#1951=LINE('',#24719,#2544);
#1952=LINE('',#24721,#2545);
#1953=LINE('',#24724,#2546);
#1954=LINE('',#24726,#2547);
#1955=LINE('',#24729,#2548);
#1956=LINE('',#24731,#2549);
#1957=LINE('',#24734,#2550);
#1958=LINE('',#24736,#2551);
#1959=LINE('',#24739,#2552);
#1960=LINE('',#24741,#2553);
#1961=LINE('',#24744,#2554);
#1962=LINE('',#24746,#2555);
#1963=LINE('',#24749,#2556);
#1964=LINE('',#24751,#2557);
#1965=LINE('',#24754,#2558);
#1966=LINE('',#24756,#2559);
#1967=LINE('',#24759,#2560);
#1968=LINE('',#24761,#2561);
#1969=LINE('',#24764,#2562);
#1970=LINE('',#24766,#2563);
#1971=LINE('',#24769,#2564);
#1972=LINE('',#24771,#2565);
#1973=LINE('',#24774,#2566);
#1974=LINE('',#24776,#2567);
#1975=LINE('',#24779,#2568);
#1976=LINE('',#24781,#2569);
#1977=LINE('',#24784,#2570);
#1978=LINE('',#24786,#2571);
#1979=LINE('',#24789,#2572);
#1980=LINE('',#24791,#2573);
#1981=LINE('',#24794,#2574);
#1982=LINE('',#24796,#2575);
#1983=LINE('',#24799,#2576);
#1984=LINE('',#24801,#2577);
#1985=LINE('',#24804,#2578);
#1986=LINE('',#24806,#2579);
#1987=LINE('',#24809,#2580);
#1988=LINE('',#24811,#2581);
#1989=LINE('',#24814,#2582);
#1990=LINE('',#24816,#2583);
#1991=LINE('',#24819,#2584);
#1992=LINE('',#24821,#2585);
#1993=LINE('',#24824,#2586);
#1994=LINE('',#24826,#2587);
#1995=LINE('',#24829,#2588);
#1996=LINE('',#24831,#2589);
#1997=LINE('',#24834,#2590);
#1998=LINE('',#24836,#2591);
#1999=LINE('',#24839,#2592);
#2000=LINE('',#25302,#2593);
#2001=LINE('',#25310,#2594);
#2002=LINE('',#25320,#2595);
#2003=LINE('',#25328,#2596);
#2004=LINE('',#25346,#2597);
#2005=LINE('',#25354,#2598);
#2006=LINE('',#25360,#2599);
#2007=LINE('',#25368,#2600);
#2008=LINE('',#25378,#2601);
#2009=LINE('',#25386,#2602);
#2010=LINE('',#25392,#2603);
#2011=LINE('',#25402,#2604);
#2012=LINE('',#25408,#2605);
#2013=LINE('',#25418,#2606);
#2014=LINE('',#25424,#2607);
#2015=LINE('',#25434,#2608);
#2016=LINE('',#25440,#2609);
#2017=LINE('',#27007,#2610);
#2018=LINE('',#27155,#2611);
#2019=LINE('',#27232,#2612);
#2020=LINE('',#27654,#2613);
#2021=LINE('',#27771,#2614);
#2022=LINE('',#27891,#2615);
#2023=LINE('',#27999,#2616);
#2024=LINE('',#28107,#2617);
#2025=LINE('',#28178,#2618);
#2026=LINE('',#28255,#2619);
#2027=LINE('',#28350,#2620);
#2028=LINE('',#28491,#2621);
#2029=LINE('',#28632,#2622);
#2030=LINE('',#28740,#2623);
#2031=LINE('',#28848,#2624);
#2032=LINE('',#30659,#2625);
#2033=LINE('',#30713,#2626);
#2034=LINE('',#30767,#2627);
#2035=LINE('',#30821,#2628);
#2036=LINE('',#30875,#2629);
#2037=LINE('',#30929,#2630);
#2038=LINE('',#30981,#2631);
#2039=LINE('',#31014,#2632);
#2040=LINE('',#31047,#2633);
#2041=LINE('',#31080,#2634);
#2042=LINE('',#31138,#2635);
#2043=LINE('',#31195,#2636);
#2044=LINE('',#31395,#2637);
#2045=LINE('',#31435,#2638);
#2046=LINE('',#31536,#2639);
#2047=LINE('',#31910,#2640);
#2048=LINE('',#32077,#2641);
#2049=LINE('',#32285,#2642);
#2050=LINE('',#32314,#2643);
#2051=LINE('',#32385,#2644);
#2052=LINE('',#32431,#2645);
#2053=LINE('',#32477,#2646);
#2054=LINE('',#32523,#2647);
#2055=LINE('',#32606,#2648);
#2056=LINE('',#32652,#2649);
#2057=LINE('',#32735,#2650);
#2058=LINE('',#32777,#2651);
#2059=LINE('',#32885,#2652);
#2060=LINE('',#32931,#2653);
#2061=LINE('',#33051,#2654);
#2062=LINE('',#33104,#2655);
#2063=LINE('',#33156,#2656);
#2064=LINE('',#33202,#2657);
#2065=LINE('',#33322,#2658);
#2066=LINE('',#33364,#2659);
#2067=LINE('',#33472,#2660);
#2068=LINE('',#33514,#2661);
#2069=LINE('',#33622,#2662);
#2070=LINE('',#33664,#2663);
#2071=LINE('',#33772,#2664);
#2072=LINE('',#33814,#2665);
#2073=LINE('',#33922,#2666);
#2074=LINE('',#33975,#2667);
#2075=LINE('',#34484,#2668);
#2076=LINE('',#34526,#2669);
#2077=LINE('',#35085,#2670);
#2078=LINE('',#35086,#2671);
#2079=LINE('',#35143,#2672);
#2080=LINE('',#35147,#2673);
#2081=LINE('',#35167,#2674);
#2082=LINE('',#35214,#2675);
#2083=LINE('',#35926,#2676);
#2084=LINE('',#35952,#2677);
#2085=LINE('',#36068,#2678);
#2086=LINE('',#36165,#2679);
#2087=LINE('',#47685,#2680);
#2088=LINE('',#47709,#2681);
#2089=LINE('',#47710,#2682);
#2090=LINE('',#47712,#2683);
#2091=LINE('',#47713,#2684);
#2092=LINE('',#47719,#2685);
#2093=LINE('',#47720,#2686);
#2094=LINE('',#47722,#2687);
#2095=LINE('',#47723,#2688);
#2096=LINE('',#47730,#2689);
#2097=LINE('',#47745,#2690);
#2098=LINE('',#47751,#2691);
#2099=LINE('',#47767,#2692);
#2100=LINE('',#47872,#2693);
#2101=LINE('',#47988,#2694);
#2102=LINE('',#47990,#2695);
#2103=LINE('',#47992,#2696);
#2104=LINE('',#47994,#2697);
#2105=LINE('',#47996,#2698);
#2106=LINE('',#47998,#2699);
#2107=LINE('',#48000,#2700);
#2108=LINE('',#48002,#2701);
#2109=LINE('',#48004,#2702);
#2110=LINE('',#48012,#2703);
#2111=LINE('',#48014,#2704);
#2112=LINE('',#48016,#2705);
#2113=LINE('',#48018,#2706);
#2114=LINE('',#48019,#2707);
#2115=LINE('',#48025,#2708);
#2116=LINE('',#48027,#2709);
#2117=LINE('',#48029,#2710);
#2118=LINE('',#48031,#2711);
#2119=LINE('',#48033,#2712);
#2120=LINE('',#48035,#2713);
#2121=LINE('',#48037,#2714);
#2122=LINE('',#48039,#2715);
#2123=LINE('',#48041,#2716);
#2124=LINE('',#48043,#2717);
#2125=LINE('',#48045,#2718);
#2126=LINE('',#48047,#2719);
#2127=LINE('',#48049,#2720);
#2128=LINE('',#48051,#2721);
#2129=LINE('',#48062,#2722);
#2130=LINE('',#48064,#2723);
#2131=LINE('',#48066,#2724);
#2132=LINE('',#48067,#2725);
#2133=LINE('',#48071,#2726);
#2134=LINE('',#48072,#2727);
#2135=LINE('',#48073,#2728);
#2136=LINE('',#48077,#2729);
#2137=LINE('',#48078,#2730);
#2138=LINE('',#48079,#2731);
#2139=LINE('',#48083,#2732);
#2140=LINE('',#48084,#2733);
#2141=LINE('',#48085,#2734);
#2142=LINE('',#48089,#2735);
#2143=LINE('',#48090,#2736);
#2144=LINE('',#48091,#2737);
#2145=LINE('',#48095,#2738);
#2146=LINE('',#48096,#2739);
#2147=LINE('',#48097,#2740);
#2148=LINE('',#48101,#2741);
#2149=LINE('',#48102,#2742);
#2150=LINE('',#48103,#2743);
#2151=LINE('',#48107,#2744);
#2152=LINE('',#48108,#2745);
#2153=LINE('',#48109,#2746);
#2154=LINE('',#48113,#2747);
#2155=LINE('',#48114,#2748);
#2156=LINE('',#48115,#2749);
#2157=LINE('',#48119,#2750);
#2158=LINE('',#48123,#2751);
#2159=LINE('',#48128,#2752);
#2160=LINE('',#48130,#2753);
#2161=LINE('',#48132,#2754);
#2162=LINE('',#48133,#2755);
#2163=LINE('',#48137,#2756);
#2164=LINE('',#48138,#2757);
#2165=LINE('',#48139,#2758);
#2166=LINE('',#48143,#2759);
#2167=LINE('',#48144,#2760);
#2168=LINE('',#48145,#2761);
#2169=LINE('',#48149,#2762);
#2170=LINE('',#48150,#2763);
#2171=LINE('',#48151,#2764);
#2172=LINE('',#48153,#2765);
#2173=LINE('',#48154,#2766);
#2174=LINE('',#48161,#2767);
#2175=LINE('',#48245,#2768);
#2176=LINE('',#48249,#2769);
#2177=LINE('',#48254,#2770);
#2178=LINE('',#48256,#2771);
#2179=LINE('',#48258,#2772);
#2180=LINE('',#48259,#2773);
#2181=LINE('',#48263,#2774);
#2182=LINE('',#48265,#2775);
#2183=LINE('',#48267,#2776);
#2184=LINE('',#48268,#2777);
#2185=LINE('',#48272,#2778);
#2186=LINE('',#48273,#2779);
#2187=LINE('',#48274,#2780);
#2188=LINE('',#48278,#2781);
#2189=LINE('',#48279,#2782);
#2190=LINE('',#48280,#2783);
#2191=LINE('',#48284,#2784);
#2192=LINE('',#48285,#2785);
#2193=LINE('',#48286,#2786);
#2194=LINE('',#48290,#2787);
#2195=LINE('',#48291,#2788);
#2196=LINE('',#48292,#2789);
#2197=LINE('',#48296,#2790);
#2198=LINE('',#48297,#2791);
#2199=LINE('',#48298,#2792);
#2200=LINE('',#48302,#2793);
#2201=LINE('',#48303,#2794);
#2202=LINE('',#48304,#2795);
#2203=LINE('',#48308,#2796);
#2204=LINE('',#48309,#2797);
#2205=LINE('',#48310,#2798);
#2206=LINE('',#48314,#2799);
#2207=LINE('',#48315,#2800);
#2208=LINE('',#48316,#2801);
#2209=LINE('',#48320,#2802);
#2210=LINE('',#48321,#2803);
#2211=LINE('',#48322,#2804);
#2212=LINE('',#48326,#2805);
#2213=LINE('',#48327,#2806);
#2214=LINE('',#48328,#2807);
#2215=LINE('',#48332,#2808);
#2216=LINE('',#48333,#2809);
#2217=LINE('',#48334,#2810);
#2218=LINE('',#48338,#2811);
#2219=LINE('',#48340,#2812);
#2220=LINE('',#48342,#2813);
#2221=LINE('',#48343,#2814);
#2222=LINE('',#48347,#2815);
#2223=LINE('',#48349,#2816);
#2224=LINE('',#48351,#2817);
#2225=LINE('',#48359,#2818);
#2226=LINE('',#48363,#2819);
#2227=LINE('',#48365,#2820);
#2228=LINE('',#48367,#2821);
#2229=LINE('',#48369,#2822);
#2230=LINE('',#48371,#2823);
#2231=LINE('',#48373,#2824);
#2232=LINE('',#48375,#2825);
#2233=LINE('',#48377,#2826);
#2234=LINE('',#48379,#2827);
#2235=LINE('',#48380,#2828);
#2236=LINE('',#48386,#2829);
#2237=LINE('',#48388,#2830);
#2238=LINE('',#48390,#2831);
#2239=LINE('',#48394,#2832);
#2240=LINE('',#48402,#2833);
#2241=LINE('',#48404,#2834);
#2242=LINE('',#48406,#2835);
#2243=LINE('',#48408,#2836);
#2244=LINE('',#48410,#2837);
#2245=LINE('',#48412,#2838);
#2246=LINE('',#48414,#2839);
#2247=LINE('',#48416,#2840);
#2248=LINE('',#48418,#2841);
#2249=LINE('',#48419,#2842);
#2250=LINE('',#48428,#2843);
#2251=LINE('',#48527,#2844);
#2252=LINE('',#48535,#2845);
#2253=LINE('',#48538,#2846);
#2254=LINE('',#48541,#2847);
#2255=LINE('',#48543,#2848);
#2256=LINE('',#48544,#2849);
#2257=LINE('',#48549,#2850);
#2258=LINE('',#48552,#2851);
#2259=LINE('',#48553,#2852);
#2260=LINE('',#48568,#2853);
#2261=LINE('',#48576,#2854);
#2262=LINE('',#48636,#2855);
#2263=LINE('',#48644,#2856);
#2264=LINE('',#48647,#2857);
#2265=LINE('',#48650,#2858);
#2266=LINE('',#48652,#2859);
#2267=LINE('',#48653,#2860);
#2268=LINE('',#48656,#2861);
#2269=LINE('',#48657,#2862);
#2270=LINE('',#48660,#2863);
#2271=LINE('',#48661,#2864);
#2272=LINE('',#48664,#2865);
#2273=LINE('',#48665,#2866);
#2274=LINE('',#48668,#2867);
#2275=LINE('',#48669,#2868);
#2276=LINE('',#48672,#2869);
#2277=LINE('',#48673,#2870);
#2278=LINE('',#48676,#2871);
#2279=LINE('',#48677,#2872);
#2280=LINE('',#48680,#2873);
#2281=LINE('',#48681,#2874);
#2282=LINE('',#48684,#2875);
#2283=LINE('',#48685,#2876);
#2284=LINE('',#48688,#2877);
#2285=LINE('',#48689,#2878);
#2286=LINE('',#48692,#2879);
#2287=LINE('',#48693,#2880);
#2288=LINE('',#48696,#2881);
#2289=LINE('',#48697,#2882);
#2290=LINE('',#48700,#2883);
#2291=LINE('',#48701,#2884);
#2292=LINE('',#48704,#2885);
#2293=LINE('',#48705,#2886);
#2294=LINE('',#48708,#2887);
#2295=LINE('',#48709,#2888);
#2296=LINE('',#48712,#2889);
#2297=LINE('',#48713,#2890);
#2298=LINE('',#48716,#2891);
#2299=LINE('',#48717,#2892);
#2300=LINE('',#48720,#2893);
#2301=LINE('',#48721,#2894);
#2302=LINE('',#48724,#2895);
#2303=LINE('',#48725,#2896);
#2304=LINE('',#48727,#2897);
#2305=LINE('',#48735,#2898);
#2306=LINE('',#48739,#2899);
#2307=LINE('',#48776,#2900);
#2308=LINE('',#48786,#2901);
#2309=LINE('',#48796,#2902);
#2310=LINE('',#48806,#2903);
#2311=LINE('',#48890,#2904);
#2312=LINE('',#48894,#2905);
#2313=LINE('',#48899,#2906);
#2314=LINE('',#48901,#2907);
#2315=LINE('',#48903,#2908);
#2316=LINE('',#48904,#2909);
#2317=LINE('',#48908,#2910);
#2318=LINE('',#48910,#2911);
#2319=LINE('',#48912,#2912);
#2320=LINE('',#48913,#2913);
#2321=LINE('',#48918,#2914);
#2322=LINE('',#48922,#2915);
#2323=LINE('',#48924,#2916);
#2324=LINE('',#48925,#2917);
#2325=LINE('',#48929,#2918);
#2326=LINE('',#48931,#2919);
#2327=LINE('',#48933,#2920);
#2328=LINE('',#48934,#2921);
#2329=LINE('',#48938,#2922);
#2330=LINE('',#48942,#2923);
#2331=LINE('',#48972,#2924);
#2332=LINE('',#48974,#2925);
#2333=LINE('',#48978,#2926);
#2334=LINE('',#48979,#2927);
#2335=LINE('',#48985,#2928);
#2336=LINE('',#48987,#2929);
#2337=LINE('',#49011,#2930);
#2338=LINE('',#49013,#2931);
#2339=LINE('',#49023,#2932);
#2340=LINE('',#49605,#2933);
#2341=LINE('',#49609,#2934);
#2342=LINE('',#49617,#2935);
#2343=LINE('',#49624,#2936);
#2344=LINE('',#49627,#2937);
#2345=LINE('',#49631,#2938);
#2346=LINE('',#49635,#2939);
#2347=LINE('',#49675,#2940);
#2348=LINE('',#49679,#2941);
#2349=LINE('',#49695,#2942);
#2350=LINE('',#49698,#2943);
#2351=LINE('',#49736,#2944);
#2352=LINE('',#49764,#2945);
#2353=LINE('',#49768,#2946);
#2354=LINE('',#49773,#2947);
#2355=LINE('',#49774,#2948);
#2356=LINE('',#49775,#2949);
#2357=LINE('',#49779,#2950);
#2358=LINE('',#49783,#2951);
#2359=LINE('',#49787,#2952);
#2360=LINE('',#49789,#2953);
#2361=LINE('',#49790,#2954);
#2362=LINE('',#49797,#2955);
#2363=LINE('',#49801,#2956);
#2364=LINE('',#49803,#2957);
#2365=LINE('',#49807,#2958);
#2366=LINE('',#49811,#2959);
#2367=LINE('',#49814,#2960);
#2368=LINE('',#49837,#2961);
#2369=LINE('',#49841,#2962);
#2370=LINE('',#49845,#2963);
#2371=LINE('',#49849,#2964);
#2372=LINE('',#49883,#2965);
#2373=LINE('',#49887,#2966);
#2374=LINE('',#49925,#2967);
#2375=LINE('',#49932,#2968);
#2376=LINE('',#49968,#2969);
#2377=LINE('',#49983,#2970);
#2378=LINE('',#49985,#2971);
#2379=LINE('',#49987,#2972);
#2380=LINE('',#49991,#2973);
#2381=LINE('',#50007,#2974);
#2382=LINE('',#50036,#2975);
#2383=LINE('',#50040,#2976);
#2384=LINE('',#50041,#2977);
#2385=LINE('',#50667,#2978);
#2386=LINE('',#50933,#2979);
#2387=LINE('',#51382,#2980);
#2388=LINE('',#51385,#2981);
#2389=LINE('',#51388,#2982);
#2390=LINE('',#51393,#2983);
#2391=LINE('',#51529,#2984);
#2392=LINE('',#51531,#2985);
#2393=LINE('',#51535,#2986);
#2394=LINE('',#51537,#2987);
#2395=LINE('',#51551,#2988);
#2396=LINE('',#51555,#2989);
#2397=LINE('',#51560,#2990);
#2398=LINE('',#51561,#2991);
#2399=LINE('',#51562,#2992);
#2400=LINE('',#51565,#2993);
#2401=LINE('',#51567,#2994);
#2402=LINE('',#51568,#2995);
#2403=LINE('',#54511,#2996);
#2404=LINE('',#54513,#2997);
#2405=LINE('',#54515,#2998);
#2406=LINE('',#54517,#2999);
#2407=LINE('',#54532,#3000);
#2408=VECTOR('',#19979,1.);
#2409=VECTOR('',#19980,1.);
#2410=VECTOR('',#19985,1.);
#2411=VECTOR('',#19988,1.);
#2412=VECTOR('',#19991,1.);
#2413=VECTOR('',#19992,1.);
#2414=VECTOR('',#19997,1.);
#2415=VECTOR('',#19998,1.);
#2416=VECTOR('',#20003,1.);
#2417=VECTOR('',#20004,1.);
#2418=VECTOR('',#20009,1.);
#2419=VECTOR('',#20012,1.);
#2420=VECTOR('',#20015,1.);
#2421=VECTOR('',#20018,1.);
#2422=VECTOR('',#20021,1.);
#2423=VECTOR('',#20022,1.);
#2424=VECTOR('',#20027,1.);
#2425=VECTOR('',#20030,1.);
#2426=VECTOR('',#20033,1.);
#2427=VECTOR('',#20034,1.);
#2428=VECTOR('',#20039,1.);
#2429=VECTOR('',#20040,1.);
#2430=VECTOR('',#20045,1.);
#2431=VECTOR('',#20046,1.);
#2432=VECTOR('',#20051,1.);
#2433=VECTOR('',#20052,1.);
#2434=VECTOR('',#20057,1.);
#2435=VECTOR('',#20060,1.);
#2436=VECTOR('',#20063,1.);
#2437=VECTOR('',#20064,1.);
#2438=VECTOR('',#20069,1.);
#2439=VECTOR('',#20070,1.);
#2440=VECTOR('',#20075,1.);
#2441=VECTOR('',#20076,1.);
#2442=VECTOR('',#20081,1.);
#2443=VECTOR('',#20084,1.);
#2444=VECTOR('',#20087,1.);
#2445=VECTOR('',#20090,1.);
#2446=VECTOR('',#20093,1.);
#2447=VECTOR('',#20094,1.);
#2448=VECTOR('',#20099,1.);
#2449=VECTOR('',#20102,1.);
#2450=VECTOR('',#20105,1.);
#2451=VECTOR('',#20106,1.);
#2452=VECTOR('',#20111,1.);
#2453=VECTOR('',#20112,1.);
#2454=VECTOR('',#20117,1.);
#2455=VECTOR('',#20118,1.);
#2456=VECTOR('',#20123,1.);
#2457=VECTOR('',#20126,1.);
#2458=VECTOR('',#20129,1.);
#2459=VECTOR('',#20130,1.);
#2460=VECTOR('',#20135,1.);
#2461=VECTOR('',#20136,1.);
#2462=VECTOR('',#20141,1.);
#2463=VECTOR('',#20142,1.);
#2464=VECTOR('',#20147,1.);
#2465=VECTOR('',#20150,1.);
#2466=VECTOR('',#20153,1.);
#2467=VECTOR('',#20154,1.);
#2468=VECTOR('',#20159,1.);
#2469=VECTOR('',#20160,1.);
#2470=VECTOR('',#20165,1.);
#2471=VECTOR('',#20168,1.);
#2472=VECTOR('',#20171,1.);
#2473=VECTOR('',#20172,1.);
#2474=VECTOR('',#20177,1.);
#2475=VECTOR('',#20178,1.);
#2476=VECTOR('',#20183,1.);
#2477=VECTOR('',#20184,1.);
#2478=VECTOR('',#20189,1.);
#2479=VECTOR('',#20192,1.);
#2480=VECTOR('',#20195,1.);
#2481=VECTOR('',#20196,1.);
#2482=VECTOR('',#20201,1.);
#2483=VECTOR('',#20202,1.);
#2484=VECTOR('',#20207,1.);
#2485=VECTOR('',#20208,1.);
#2486=VECTOR('',#20213,1.);
#2487=VECTOR('',#20216,1.);
#2488=VECTOR('',#20219,1.);
#2489=VECTOR('',#20220,1.);
#2490=VECTOR('',#20225,1.);
#2491=VECTOR('',#20226,1.);
#2492=VECTOR('',#20231,1.);
#2493=VECTOR('',#20234,1.);
#2494=VECTOR('',#20237,1.);
#2495=VECTOR('',#20238,1.);
#2496=VECTOR('',#20243,1.);
#2497=VECTOR('',#20244,1.);
#2498=VECTOR('',#20531,1.);
#2499=VECTOR('',#20532,1.);
#2500=VECTOR('',#20535,1.);
#2501=VECTOR('',#20538,1.);
#2502=VECTOR('',#20543,1.);
#2503=VECTOR('',#20546,1.);
#2504=VECTOR('',#20551,1.);
#2505=VECTOR('',#20554,1.);
#2506=VECTOR('',#20559,1.);
#2507=VECTOR('',#20562,1.);
#2508=VECTOR('',#20567,1.);
#2509=VECTOR('',#20570,1.);
#2510=VECTOR('',#20575,1.);
#2511=VECTOR('',#20578,1.);
#2512=VECTOR('',#20583,1.);
#2513=VECTOR('',#20586,1.);
#2514=VECTOR('',#20591,1.);
#2515=VECTOR('',#20594,1.);
#2516=VECTOR('',#20599,1.);
#2517=VECTOR('',#20602,1.);
#2518=VECTOR('',#20607,1.);
#2519=VECTOR('',#20610,1.);
#2520=VECTOR('',#20615,1.);
#2521=VECTOR('',#20618,1.);
#2522=VECTOR('',#20623,1.);
#2523=VECTOR('',#20626,1.);
#2524=VECTOR('',#20631,1.);
#2525=VECTOR('',#20634,1.);
#2526=VECTOR('',#20639,1.);
#2527=VECTOR('',#20642,1.);
#2528=VECTOR('',#20647,1.);
#2529=VECTOR('',#20650,1.);
#2530=VECTOR('',#20655,1.);
#2531=VECTOR('',#20658,1.);
#2532=VECTOR('',#20663,1.);
#2533=VECTOR('',#20666,1.);
#2534=VECTOR('',#20671,1.);
#2535=VECTOR('',#20674,1.);
#2536=VECTOR('',#20679,1.);
#2537=VECTOR('',#20682,1.);
#2538=VECTOR('',#20687,1.);
#2539=VECTOR('',#20690,1.);
#2540=VECTOR('',#20695,1.);
#2541=VECTOR('',#20698,1.);
#2542=VECTOR('',#20703,1.);
#2543=VECTOR('',#20706,1.);
#2544=VECTOR('',#20711,1.);
#2545=VECTOR('',#20714,1.);
#2546=VECTOR('',#20719,1.);
#2547=VECTOR('',#20722,1.);
#2548=VECTOR('',#20727,1.);
#2549=VECTOR('',#20730,1.);
#2550=VECTOR('',#20735,1.);
#2551=VECTOR('',#20738,1.);
#2552=VECTOR('',#20743,1.);
#2553=VECTOR('',#20746,1.);
#2554=VECTOR('',#20751,1.);
#2555=VECTOR('',#20754,1.);
#2556=VECTOR('',#20759,1.);
#2557=VECTOR('',#20762,1.);
#2558=VECTOR('',#20767,1.);
#2559=VECTOR('',#20770,1.);
#2560=VECTOR('',#20775,1.);
#2561=VECTOR('',#20778,1.);
#2562=VECTOR('',#20783,1.);
#2563=VECTOR('',#20786,1.);
#2564=VECTOR('',#20791,1.);
#2565=VECTOR('',#20794,1.);
#2566=VECTOR('',#20799,1.);
#2567=VECTOR('',#20802,1.);
#2568=VECTOR('',#20807,1.);
#2569=VECTOR('',#20810,1.);
#2570=VECTOR('',#20815,1.);
#2571=VECTOR('',#20818,1.);
#2572=VECTOR('',#20823,1.);
#2573=VECTOR('',#20826,1.);
#2574=VECTOR('',#20831,1.);
#2575=VECTOR('',#20834,1.);
#2576=VECTOR('',#20839,1.);
#2577=VECTOR('',#20842,1.);
#2578=VECTOR('',#20847,1.);
#2579=VECTOR('',#20850,1.);
#2580=VECTOR('',#20855,1.);
#2581=VECTOR('',#20858,1.);
#2582=VECTOR('',#20863,1.);
#2583=VECTOR('',#20866,1.);
#2584=VECTOR('',#20871,1.);
#2585=VECTOR('',#20874,1.);
#2586=VECTOR('',#20879,1.);
#2587=VECTOR('',#20882,1.);
#2588=VECTOR('',#20887,1.);
#2589=VECTOR('',#20890,1.);
#2590=VECTOR('',#20895,1.);
#2591=VECTOR('',#20898,1.);
#2592=VECTOR('',#20903,0.009);
#2593=VECTOR('',#20912,0.005);
#2594=VECTOR('',#20921,0.0074756477610481);
#2595=VECTOR('',#20932,0.00932888901198444);
#2596=VECTOR('',#20941,0.00932888901198444);
#2597=VECTOR('',#20962,0.00898940279602035);
#2598=VECTOR('',#20971,0.00912888901198444);
#2599=VECTOR('',#20978,0.00932888901198444);
#2600=VECTOR('',#20987,0.00932888901198444);
#2601=VECTOR('',#20998,0.00898940279602035);
#2602=VECTOR('',#21007,0.00912888901198443);
#2603=VECTOR('',#21014,0.00932888901198444);
#2604=VECTOR('',#21025,0.0091288890119844);
#2605=VECTOR('',#21032,0.00932888901198444);
#2606=VECTOR('',#21043,0.00912888901198441);
#2607=VECTOR('',#21050,0.00932888901198444);
#2608=VECTOR('',#21061,0.00912888901198442);
#2609=VECTOR('',#21068,0.00932888901198444);
#2610=VECTOR('',#21179,0.01);
#2611=VECTOR('',#21180,0.01);
#2612=VECTOR('',#21181,0.01);
#2613=VECTOR('',#21182,0.01);
#2614=VECTOR('',#21183,0.01);
#2615=VECTOR('',#21184,0.01);
#2616=VECTOR('',#21185,0.01);
#2617=VECTOR('',#21186,0.01);
#2618=VECTOR('',#21187,0.01);
#2619=VECTOR('',#21188,0.01);
#2620=VECTOR('',#21189,0.01);
#2621=VECTOR('',#21190,0.01);
#2622=VECTOR('',#21191,0.01);
#2623=VECTOR('',#21192,0.01);
#2624=VECTOR('',#21193,0.01);
#2625=VECTOR('',#21200,0.01);
#2626=VECTOR('',#21201,0.01);
#2627=VECTOR('',#21202,0.01);
#2628=VECTOR('',#21203,0.01);
#2629=VECTOR('',#21204,0.01);
#2630=VECTOR('',#21205,0.01);
#2631=VECTOR('',#21206,0.01);
#2632=VECTOR('',#21207,0.01);
#2633=VECTOR('',#21208,0.01);
#2634=VECTOR('',#21209,0.01);
#2635=VECTOR('',#21210,0.01);
#2636=VECTOR('',#21211,0.01);
#2637=VECTOR('',#21212,0.01);
#2638=VECTOR('',#21213,0.01);
#2639=VECTOR('',#21214,0.01);
#2640=VECTOR('',#21219,0.01);
#2641=VECTOR('',#21222,0.01);
#2642=VECTOR('',#21225,0.01);
#2643=VECTOR('',#21226,0.01);
#2644=VECTOR('',#21227,0.01);
#2645=VECTOR('',#21228,0.01);
#2646=VECTOR('',#21229,0.01);
#2647=VECTOR('',#21230,0.01);
#2648=VECTOR('',#21231,0.01);
#2649=VECTOR('',#21232,0.01);
#2650=VECTOR('',#21233,0.01);
#2651=VECTOR('',#21234,0.01);
#2652=VECTOR('',#21235,0.01);
#2653=VECTOR('',#21236,0.01);
#2654=VECTOR('',#21237,0.01);
#2655=VECTOR('',#21238,0.01);
#2656=VECTOR('',#21239,0.01);
#2657=VECTOR('',#21240,0.01);
#2658=VECTOR('',#21241,0.01);
#2659=VECTOR('',#21242,0.01);
#2660=VECTOR('',#21243,0.01);
#2661=VECTOR('',#21244,0.01);
#2662=VECTOR('',#21245,0.01);
#2663=VECTOR('',#21246,0.01);
#2664=VECTOR('',#21247,0.01);
#2665=VECTOR('',#21248,0.01);
#2666=VECTOR('',#21249,0.01);
#2667=VECTOR('',#21250,0.01);
#2668=VECTOR('',#21251,0.01);
#2669=VECTOR('',#21252,0.01);
#2670=VECTOR('',#21253,0.01);
#2671=VECTOR('',#21254,0.01);
#2672=VECTOR('',#21261,1.);
#2673=VECTOR('',#21264,1.);
#2674=VECTOR('',#21269,1.);
#2675=VECTOR('',#21274,1.);
#2676=VECTOR('',#21297,1.);
#2677=VECTOR('',#21298,1.);
#2678=VECTOR('',#21301,1.);
#2679=VECTOR('',#21304,1.);
#2680=VECTOR('',#21727,0.0055);
#2681=VECTOR('',#21754,1.);
#2682=VECTOR('',#21755,1.);
#2683=VECTOR('',#21758,1.);
#2684=VECTOR('',#21759,1.);
#2685=VECTOR('',#21762,1.);
#2686=VECTOR('',#21763,1.);
#2687=VECTOR('',#21766,1.);
#2688=VECTOR('',#21767,1.);
#2689=VECTOR('',#21778,0.00278445714771807);
#2690=VECTOR('',#21797,0.00116635989804114);
#2691=VECTOR('',#21806,0.00184479343283513);
#2692=VECTOR('',#21811,0.00134583534834952);
#2693=VECTOR('',#21824,0.00125);
#2694=VECTOR('',#21845,0.999999999999999);
#2695=VECTOR('',#21846,1.);
#2696=VECTOR('',#21847,1.);
#2697=VECTOR('',#21848,1.);
#2698=VECTOR('',#21849,1.);
#2699=VECTOR('',#21850,1.);
#2700=VECTOR('',#21851,1.);
#2701=VECTOR('',#21852,1.);
#2702=VECTOR('',#21853,1.);
#2703=VECTOR('',#21860,1.);
#2704=VECTOR('',#21861,1.);
#2705=VECTOR('',#21862,1.);
#2706=VECTOR('',#21863,1.);
#2707=VECTOR('',#21864,1.);
#2708=VECTOR('',#21869,1.);
#2709=VECTOR('',#21870,1.);
#2710=VECTOR('',#21871,1.);
#2711=VECTOR('',#21872,1.);
#2712=VECTOR('',#21873,1.);
#2713=VECTOR('',#21874,1.);
#2714=VECTOR('',#21875,1.);
#2715=VECTOR('',#21876,1.);
#2716=VECTOR('',#21877,0.999999999999999);
#2717=VECTOR('',#21878,1.);
#2718=VECTOR('',#21879,1.);
#2719=VECTOR('',#21880,1.);
#2720=VECTOR('',#21881,1.);
#2721=VECTOR('',#21882,1.);
#2722=VECTOR('',#21893,1.);
#2723=VECTOR('',#21894,1.);
#2724=VECTOR('',#21895,1.);
#2725=VECTOR('',#21896,1.);
#2726=VECTOR('',#21899,1.);
#2727=VECTOR('',#21900,1.);
#2728=VECTOR('',#21901,1.);
#2729=VECTOR('',#21904,1.);
#2730=VECTOR('',#21905,1.);
#2731=VECTOR('',#21906,1.);
#2732=VECTOR('',#21909,1.);
#2733=VECTOR('',#21910,0.999999999999999);
#2734=VECTOR('',#21911,0.999999999999999);
#2735=VECTOR('',#21914,1.);
#2736=VECTOR('',#21915,1.);
#2737=VECTOR('',#21916,1.);
#2738=VECTOR('',#21919,1.);
#2739=VECTOR('',#21920,1.);
#2740=VECTOR('',#21921,1.);
#2741=VECTOR('',#21924,1.);
#2742=VECTOR('',#21925,1.);
#2743=VECTOR('',#21926,1.);
#2744=VECTOR('',#21929,1.);
#2745=VECTOR('',#21930,1.);
#2746=VECTOR('',#21931,1.);
#2747=VECTOR('',#21934,1.);
#2748=VECTOR('',#21935,1.);
#2749=VECTOR('',#21936,1.);
#2750=VECTOR('',#21939,1.);
#2751=VECTOR('',#21942,1.);
#2752=VECTOR('',#21947,1.);
#2753=VECTOR('',#21948,1.);
#2754=VECTOR('',#21949,1.);
#2755=VECTOR('',#21950,1.);
#2756=VECTOR('',#21953,1.);
#2757=VECTOR('',#21954,1.);
#2758=VECTOR('',#21955,1.);
#2759=VECTOR('',#21958,1.);
#2760=VECTOR('',#21959,1.);
#2761=VECTOR('',#21960,1.);
#2762=VECTOR('',#21963,1.);
#2763=VECTOR('',#21964,1.);
#2764=VECTOR('',#21965,1.);
#2765=VECTOR('',#21968,1.);
#2766=VECTOR('',#21969,1.);
#2767=VECTOR('',#21976,0.0005);
#2768=VECTOR('',#22139,1.);
#2769=VECTOR('',#22142,1.);
#2770=VECTOR('',#22147,1.);
#2771=VECTOR('',#22148,1.);
#2772=VECTOR('',#22149,1.);
#2773=VECTOR('',#22150,1.);
#2774=VECTOR('',#22153,1.);
#2775=VECTOR('',#22154,1.);
#2776=VECTOR('',#22155,1.);
#2777=VECTOR('',#22156,1.);
#2778=VECTOR('',#22159,1.);
#2779=VECTOR('',#22160,1.);
#2780=VECTOR('',#22161,1.);
#2781=VECTOR('',#22164,1.);
#2782=VECTOR('',#22165,1.);
#2783=VECTOR('',#22166,1.);
#2784=VECTOR('',#22169,1.);
#2785=VECTOR('',#22170,1.);
#2786=VECTOR('',#22171,1.);
#2787=VECTOR('',#22174,1.);
#2788=VECTOR('',#22175,0.999999999999999);
#2789=VECTOR('',#22176,0.999999999999999);
#2790=VECTOR('',#22179,1.);
#2791=VECTOR('',#22180,1.);
#2792=VECTOR('',#22181,1.);
#2793=VECTOR('',#22184,1.);
#2794=VECTOR('',#22185,1.);
#2795=VECTOR('',#22186,1.);
#2796=VECTOR('',#22189,1.);
#2797=VECTOR('',#22190,1.);
#2798=VECTOR('',#22191,1.);
#2799=VECTOR('',#22194,1.);
#2800=VECTOR('',#22195,1.);
#2801=VECTOR('',#22196,1.);
#2802=VECTOR('',#22199,1.);
#2803=VECTOR('',#22200,1.);
#2804=VECTOR('',#22201,1.);
#2805=VECTOR('',#22204,1.);
#2806=VECTOR('',#22205,1.);
#2807=VECTOR('',#22206,1.);
#2808=VECTOR('',#22209,1.);
#2809=VECTOR('',#22210,1.);
#2810=VECTOR('',#22211,1.);
#2811=VECTOR('',#22214,1.);
#2812=VECTOR('',#22215,1.);
#2813=VECTOR('',#22216,1.);
#2814=VECTOR('',#22217,1.);
#2815=VECTOR('',#22220,1.);
#2816=VECTOR('',#22221,1.);
#2817=VECTOR('',#22222,1.);
#2818=VECTOR('',#22229,1.);
#2819=VECTOR('',#22232,1.);
#2820=VECTOR('',#22233,1.);
#2821=VECTOR('',#22234,1.);
#2822=VECTOR('',#22235,1.);
#2823=VECTOR('',#22236,1.);
#2824=VECTOR('',#22237,1.);
#2825=VECTOR('',#22238,1.);
#2826=VECTOR('',#22239,0.999999999999999);
#2827=VECTOR('',#22240,1.);
#2828=VECTOR('',#22241,1.);
#2829=VECTOR('',#22246,1.);
#2830=VECTOR('',#22247,1.);
#2831=VECTOR('',#22248,1.);
#2832=VECTOR('',#22251,1.);
#2833=VECTOR('',#22258,1.);
#2834=VECTOR('',#22259,1.);
#2835=VECTOR('',#22260,1.);
#2836=VECTOR('',#22261,1.);
#2837=VECTOR('',#22262,1.);
#2838=VECTOR('',#22263,0.999999999999999);
#2839=VECTOR('',#22264,1.);
#2840=VECTOR('',#22265,1.);
#2841=VECTOR('',#22266,1.);
#2842=VECTOR('',#22267,1.);
#2843=VECTOR('',#22276,0.0005);
#2844=VECTOR('',#22469,0.0011);
#2845=VECTOR('',#22478,1.);
#2846=VECTOR('',#22481,1.);
#2847=VECTOR('',#22484,1.);
#2848=VECTOR('',#22485,1.);
#2849=VECTOR('',#22486,1.);
#2850=VECTOR('',#22491,1.);
#2851=VECTOR('',#22496,1.);
#2852=VECTOR('',#22497,1.);
#2853=VECTOR('',#22516,0.009);
#2854=VECTOR('',#22527,0.0055);
#2855=VECTOR('',#22596,0.002);
#2856=VECTOR('',#22605,0.001);
#2857=VECTOR('',#22610,0.001);
#2858=VECTOR('',#22613,1.);
#2859=VECTOR('',#22614,1.);
#2860=VECTOR('',#22615,1.);
#2861=VECTOR('',#22618,1.);
#2862=VECTOR('',#22619,1.);
#2863=VECTOR('',#22622,1.);
#2864=VECTOR('',#22623,1.);
#2865=VECTOR('',#22626,1.);
#2866=VECTOR('',#22627,1.);
#2867=VECTOR('',#22630,1.);
#2868=VECTOR('',#22631,1.);
#2869=VECTOR('',#22634,0.999999999999999);
#2870=VECTOR('',#22635,1.);
#2871=VECTOR('',#22638,1.);
#2872=VECTOR('',#22639,1.);
#2873=VECTOR('',#22642,1.);
#2874=VECTOR('',#22643,1.);
#2875=VECTOR('',#22646,1.);
#2876=VECTOR('',#22647,1.);
#2877=VECTOR('',#22650,1.);
#2878=VECTOR('',#22651,1.);
#2879=VECTOR('',#22654,1.);
#2880=VECTOR('',#22655,1.);
#2881=VECTOR('',#22658,1.);
#2882=VECTOR('',#22659,1.);
#2883=VECTOR('',#22662,1.);
#2884=VECTOR('',#22663,1.);
#2885=VECTOR('',#22666,1.);
#2886=VECTOR('',#22667,1.);
#2887=VECTOR('',#22670,1.);
#2888=VECTOR('',#22671,1.);
#2889=VECTOR('',#22674,1.);
#2890=VECTOR('',#22675,1.);
#2891=VECTOR('',#22678,1.);
#2892=VECTOR('',#22679,0.999999999999999);
#2893=VECTOR('',#22682,1.);
#2894=VECTOR('',#22683,1.);
#2895=VECTOR('',#22686,1.);
#2896=VECTOR('',#22687,1.);
#2897=VECTOR('',#22690,1.);
#2898=VECTOR('',#22701,1.);
#2899=VECTOR('',#22704,1.);
#2900=VECTOR('',#22747,0.009);
#2901=VECTOR('',#22758,0.0012);
#2902=VECTOR('',#22769,0.0005);
#2903=VECTOR('',#22780,0.0005);
#2904=VECTOR('',#22829,0.01);
#2905=VECTOR('',#22832,0.01);
#2906=VECTOR('',#22837,1.);
#2907=VECTOR('',#22838,1.);
#2908=VECTOR('',#22839,1.);
#2909=VECTOR('',#22840,1.);
#2910=VECTOR('',#22843,1.);
#2911=VECTOR('',#22844,1.);
#2912=VECTOR('',#22845,1.);
#2913=VECTOR('',#22846,1.);
#2914=VECTOR('',#22851,1.);
#2915=VECTOR('',#22856,1.);
#2916=VECTOR('',#22857,1.);
#2917=VECTOR('',#22858,1.);
#2918=VECTOR('',#22861,1.);
#2919=VECTOR('',#22862,1.);
#2920=VECTOR('',#22863,1.);
#2921=VECTOR('',#22864,1.);
#2922=VECTOR('',#22867,0.01);
#2923=VECTOR('',#22870,0.01);
#2924=VECTOR('',#22887,1.);
#2925=VECTOR('',#22888,1.);
#2926=VECTOR('',#22891,1.);
#2927=VECTOR('',#22892,1.);
#2928=VECTOR('',#22897,1.);
#2929=VECTOR('',#22898,1.);
#2930=VECTOR('',#22905,1.);
#2931=VECTOR('',#22906,1.);
#2932=VECTOR('',#22917,0.001);
#2933=VECTOR('',#23046,1.);
#2934=VECTOR('',#23049,1.);
#2935=VECTOR('',#23058,0.001);
#2936=VECTOR('',#23065,1.);
#2937=VECTOR('',#23068,1.);
#2938=VECTOR('',#23071,1.);
#2939=VECTOR('',#23074,1.);
#2940=VECTOR('',#23109,1.);
#2941=VECTOR('',#23112,1.);
#2942=VECTOR('',#23117,1.);
#2943=VECTOR('',#23120,1.);
#2944=VECTOR('',#23129,0.005);
#2945=VECTOR('',#23138,1.);
#2946=VECTOR('',#23141,1.);
#2947=VECTOR('',#23146,1.);
#2948=VECTOR('',#23147,1.);
#2949=VECTOR('',#23148,1.);
#2950=VECTOR('',#23151,1.);
#2951=VECTOR('',#23154,1.);
#2952=VECTOR('',#23159,1.);
#2953=VECTOR('',#23160,1.);
#2954=VECTOR('',#23161,1.);
#2955=VECTOR('',#23170,1.);
#2956=VECTOR('',#23173,1.);
#2957=VECTOR('',#23174,1.);
#2958=VECTOR('',#23177,1.);
#2959=VECTOR('',#23180,1.);
#2960=VECTOR('',#23183,1.);
#2961=VECTOR('',#23192,1.);
#2962=VECTOR('',#23195,1.);
#2963=VECTOR('',#23198,1.);
#2964=VECTOR('',#23201,1.);
#2965=VECTOR('',#23208,1.);
#2966=VECTOR('',#23211,1.);
#2967=VECTOR('',#23256,0.009);
#2968=VECTOR('',#23263,1.);
#2969=VECTOR('',#23264,0.01);
#2970=VECTOR('',#23265,1.);
#2971=VECTOR('',#23266,1.);
#2972=VECTOR('',#23267,1.);
#2973=VECTOR('',#23272,1.);
#2974=VECTOR('',#23273,0.01);
#2975=VECTOR('',#23274,1.);
#2976=VECTOR('',#23277,1.);
#2977=VECTOR('',#23278,1.);
#2978=VECTOR('',#23279,0.01);
#2979=VECTOR('',#23280,0.01);
#2980=VECTOR('',#23299,1.);
#2981=VECTOR('',#23302,1.);
#2982=VECTOR('',#23305,1.);
#2983=VECTOR('',#23312,1.);
#2984=VECTOR('',#23315,1.);
#2985=VECTOR('',#23316,1.);
#2986=VECTOR('',#23319,1.);
#2987=VECTOR('',#23320,1.);
#2988=VECTOR('',#23329,1.);
#2989=VECTOR('',#23332,1.);
#2990=VECTOR('',#23337,1.);
#2991=VECTOR('',#23338,1.);
#2992=VECTOR('',#23339,1.);
#2993=VECTOR('',#23342,1.);
#2994=VECTOR('',#23343,1.);
#2995=VECTOR('',#23344,1.);
#2996=VECTOR('',#23663,0.0005);
#2997=VECTOR('',#23666,0.0005);
#2998=VECTOR('',#23669,0.0005);
#2999=VECTOR('',#23672,0.0005);
#3000=VECTOR('',#23693,0.0005);
#3001=CYLINDRICAL_SURFACE('',#18023,0.012);
#3002=CYLINDRICAL_SURFACE('',#18025,0.012);
#3003=CYLINDRICAL_SURFACE('',#18027,0.012);
#3004=CYLINDRICAL_SURFACE('',#18029,0.012);
#3005=CYLINDRICAL_SURFACE('',#18031,0.012);
#3006=CYLINDRICAL_SURFACE('',#18033,0.012);
#3007=CYLINDRICAL_SURFACE('',#18035,0.012);
#3008=CYLINDRICAL_SURFACE('',#18037,0.012);
#3009=CYLINDRICAL_SURFACE('',#18039,0.012);
#3010=CYLINDRICAL_SURFACE('',#18041,0.012);
#3011=CYLINDRICAL_SURFACE('',#18043,0.012);
#3012=CYLINDRICAL_SURFACE('',#18045,0.012);
#3013=CYLINDRICAL_SURFACE('',#18047,0.012);
#3014=CYLINDRICAL_SURFACE('',#18049,0.012);
#3015=CYLINDRICAL_SURFACE('',#18051,0.012);
#3016=CYLINDRICAL_SURFACE('',#18053,0.012);
#3017=CYLINDRICAL_SURFACE('',#18055,0.012);
#3018=CYLINDRICAL_SURFACE('',#18057,0.012);
#3019=CYLINDRICAL_SURFACE('',#18059,0.012);
#3020=CYLINDRICAL_SURFACE('',#18061,0.012);
#3021=CYLINDRICAL_SURFACE('',#18063,0.012);
#3022=CYLINDRICAL_SURFACE('',#18065,0.012);
#3023=CYLINDRICAL_SURFACE('',#18067,0.012);
#3024=CYLINDRICAL_SURFACE('',#18069,0.012);
#3025=CYLINDRICAL_SURFACE('',#18071,0.012);
#3026=CYLINDRICAL_SURFACE('',#18073,0.012);
#3027=CYLINDRICAL_SURFACE('',#18075,0.012);
#3028=CYLINDRICAL_SURFACE('',#18077,0.012);
#3029=CYLINDRICAL_SURFACE('',#18079,0.012);
#3030=CYLINDRICAL_SURFACE('',#18081,0.012);
#3031=CYLINDRICAL_SURFACE('',#18083,0.012);
#3032=CYLINDRICAL_SURFACE('',#18085,0.012);
#3033=CYLINDRICAL_SURFACE('',#18087,0.012);
#3034=CYLINDRICAL_SURFACE('',#18089,0.012);
#3035=CYLINDRICAL_SURFACE('',#18091,0.012);
#3036=CYLINDRICAL_SURFACE('',#18093,0.012);
#3037=CYLINDRICAL_SURFACE('',#18095,0.012);
#3038=CYLINDRICAL_SURFACE('',#18097,0.012);
#3039=CYLINDRICAL_SURFACE('',#18099,0.012);
#3040=CYLINDRICAL_SURFACE('',#18101,0.012);
#3041=CYLINDRICAL_SURFACE('',#18103,0.012);
#3042=CYLINDRICAL_SURFACE('',#18105,0.012);
#3043=CYLINDRICAL_SURFACE('',#18107,0.012);
#3044=CYLINDRICAL_SURFACE('',#18109,0.012);
#3045=CYLINDRICAL_SURFACE('',#18111,0.012);
#3046=CYLINDRICAL_SURFACE('',#18254,0.012);
#3047=CYLINDRICAL_SURFACE('',#18255,0.0046);
#3048=CYLINDRICAL_SURFACE('',#18256,0.0046);
#3049=CYLINDRICAL_SURFACE('',#18257,0.010874);
#3050=CYLINDRICAL_SURFACE('',#18258,0.0046);
#3051=CYLINDRICAL_SURFACE('',#18259,0.0046);
#3052=CYLINDRICAL_SURFACE('',#18260,0.010874);
#3053=CYLINDRICAL_SURFACE('',#18261,0.0046);
#3054=CYLINDRICAL_SURFACE('',#18262,0.0046);
#3055=CYLINDRICAL_SURFACE('',#18263,0.010874);
#3056=CYLINDRICAL_SURFACE('',#18264,0.0046);
#3057=CYLINDRICAL_SURFACE('',#18265,0.0046);
#3058=CYLINDRICAL_SURFACE('',#18266,0.010874);
#3059=CYLINDRICAL_SURFACE('',#18267,0.0046);
#3060=CYLINDRICAL_SURFACE('',#18268,0.0046);
#3061=CYLINDRICAL_SURFACE('',#18269,0.010874);
#3062=CYLINDRICAL_SURFACE('',#18270,0.0046);
#3063=CYLINDRICAL_SURFACE('',#18271,0.0046);
#3064=CYLINDRICAL_SURFACE('',#18272,0.010874);
#3065=CYLINDRICAL_SURFACE('',#18273,0.0046);
#3066=CYLINDRICAL_SURFACE('',#18274,0.0046);
#3067=CYLINDRICAL_SURFACE('',#18275,0.010874);
#3068=CYLINDRICAL_SURFACE('',#18276,0.0046);
#3069=CYLINDRICAL_SURFACE('',#18277,0.0046);
#3070=CYLINDRICAL_SURFACE('',#18278,0.010874);
#3071=CYLINDRICAL_SURFACE('',#18279,0.0046);
#3072=CYLINDRICAL_SURFACE('',#18280,0.0046);
#3073=CYLINDRICAL_SURFACE('',#18281,0.010874);
#3074=CYLINDRICAL_SURFACE('',#18282,0.0046);
#3075=CYLINDRICAL_SURFACE('',#18283,0.0046);
#3076=CYLINDRICAL_SURFACE('',#18284,0.010874);
#3077=CYLINDRICAL_SURFACE('',#18285,0.0046);
#3078=CYLINDRICAL_SURFACE('',#18286,0.0046);
#3079=CYLINDRICAL_SURFACE('',#18287,0.010874);
#3080=CYLINDRICAL_SURFACE('',#18288,0.0046);
#3081=CYLINDRICAL_SURFACE('',#18289,0.0046);
#3082=CYLINDRICAL_SURFACE('',#18290,0.010874);
#3083=CYLINDRICAL_SURFACE('',#18291,0.0046);
#3084=CYLINDRICAL_SURFACE('',#18292,0.0046);
#3085=CYLINDRICAL_SURFACE('',#18293,0.010874);
#3086=CYLINDRICAL_SURFACE('',#18294,0.0046);
#3087=CYLINDRICAL_SURFACE('',#18295,0.0046);
#3088=CYLINDRICAL_SURFACE('',#18296,0.010874);
#3089=CYLINDRICAL_SURFACE('',#18297,0.0046);
#3090=CYLINDRICAL_SURFACE('',#18298,0.0046);
#3091=CYLINDRICAL_SURFACE('',#18299,0.010874);
#3092=CYLINDRICAL_SURFACE('',#18300,0.0046);
#3093=CYLINDRICAL_SURFACE('',#18301,0.0046);
#3094=CYLINDRICAL_SURFACE('',#18302,0.010874);
#3095=CYLINDRICAL_SURFACE('',#18303,0.0046);
#3096=CYLINDRICAL_SURFACE('',#18304,0.0046);
#3097=CYLINDRICAL_SURFACE('',#18305,0.010874);
#3098=CYLINDRICAL_SURFACE('',#18306,0.0046);
#3099=CYLINDRICAL_SURFACE('',#18307,0.0046);
#3100=CYLINDRICAL_SURFACE('',#18308,0.010874);
#3101=CYLINDRICAL_SURFACE('',#18309,0.0046);
#3102=CYLINDRICAL_SURFACE('',#18310,0.0046);
#3103=CYLINDRICAL_SURFACE('',#18311,0.010874);
#3104=CYLINDRICAL_SURFACE('',#18312,0.0046);
#3105=CYLINDRICAL_SURFACE('',#18313,0.0046);
#3106=CYLINDRICAL_SURFACE('',#18314,0.010874);
#3107=CYLINDRICAL_SURFACE('',#18315,0.0046);
#3108=CYLINDRICAL_SURFACE('',#18316,0.0046);
#3109=CYLINDRICAL_SURFACE('',#18317,0.010874);
#3110=CYLINDRICAL_SURFACE('',#18318,0.0046);
#3111=CYLINDRICAL_SURFACE('',#18319,0.0046);
#3112=CYLINDRICAL_SURFACE('',#18320,0.010874);
#3113=CYLINDRICAL_SURFACE('',#18321,0.0046);
#3114=CYLINDRICAL_SURFACE('',#18322,0.0046);
#3115=CYLINDRICAL_SURFACE('',#18323,0.010874);
#3116=CYLINDRICAL_SURFACE('',#18324,0.0046);
#3117=CYLINDRICAL_SURFACE('',#18325,0.0046);
#3118=CYLINDRICAL_SURFACE('',#18326,0.010874);
#3119=CYLINDRICAL_SURFACE('',#18327,0.0046);
#3120=CYLINDRICAL_SURFACE('',#18328,0.0046);
#3121=CYLINDRICAL_SURFACE('',#18329,0.010874);
#3122=CYLINDRICAL_SURFACE('',#18330,0.0046);
#3123=CYLINDRICAL_SURFACE('',#18331,0.0046);
#3124=CYLINDRICAL_SURFACE('',#18332,0.010874);
#3125=CYLINDRICAL_SURFACE('',#18333,0.0046);
#3126=CYLINDRICAL_SURFACE('',#18334,0.0046);
#3127=CYLINDRICAL_SURFACE('',#18335,0.010874);
#3128=CYLINDRICAL_SURFACE('',#18336,0.0046);
#3129=CYLINDRICAL_SURFACE('',#18337,0.0046);
#3130=CYLINDRICAL_SURFACE('',#18338,0.010874);
#3131=CYLINDRICAL_SURFACE('',#18339,0.0046);
#3132=CYLINDRICAL_SURFACE('',#18340,0.0046);
#3133=CYLINDRICAL_SURFACE('',#18341,0.010874);
#3134=CYLINDRICAL_SURFACE('',#18342,0.0046);
#3135=CYLINDRICAL_SURFACE('',#18343,0.0046);
#3136=CYLINDRICAL_SURFACE('',#18344,0.010874);
#3137=CYLINDRICAL_SURFACE('',#18345,0.0046);
#3138=CYLINDRICAL_SURFACE('',#18346,0.0046);
#3139=CYLINDRICAL_SURFACE('',#18347,0.010874);
#3140=CYLINDRICAL_SURFACE('',#18348,0.0046);
#3141=CYLINDRICAL_SURFACE('',#18349,0.0046);
#3142=CYLINDRICAL_SURFACE('',#18350,0.010874);
#3143=CYLINDRICAL_SURFACE('',#18351,0.0046);
#3144=CYLINDRICAL_SURFACE('',#18352,0.0046);
#3145=CYLINDRICAL_SURFACE('',#18353,0.010874);
#3146=CYLINDRICAL_SURFACE('',#18354,0.0046);
#3147=CYLINDRICAL_SURFACE('',#18355,0.0046);
#3148=CYLINDRICAL_SURFACE('',#18356,0.010874);
#3149=CYLINDRICAL_SURFACE('',#18357,0.0046);
#3150=CYLINDRICAL_SURFACE('',#18358,0.0046);
#3151=CYLINDRICAL_SURFACE('',#18359,0.010874);
#3152=CYLINDRICAL_SURFACE('',#18360,0.0046);
#3153=CYLINDRICAL_SURFACE('',#18361,0.0046);
#3154=CYLINDRICAL_SURFACE('',#18362,0.010874);
#3155=CYLINDRICAL_SURFACE('',#18363,0.0046);
#3156=CYLINDRICAL_SURFACE('',#18364,0.0046);
#3157=CYLINDRICAL_SURFACE('',#18365,0.010874);
#3158=CYLINDRICAL_SURFACE('',#18366,0.0046);
#3159=CYLINDRICAL_SURFACE('',#18367,0.0046);
#3160=CYLINDRICAL_SURFACE('',#18368,0.010874);
#3161=CYLINDRICAL_SURFACE('',#18369,0.0046);
#3162=CYLINDRICAL_SURFACE('',#18370,0.0046);
#3163=CYLINDRICAL_SURFACE('',#18371,0.010874);
#3164=CYLINDRICAL_SURFACE('',#18372,0.0046);
#3165=CYLINDRICAL_SURFACE('',#18373,0.0046);
#3166=CYLINDRICAL_SURFACE('',#18374,0.010874);
#3167=CYLINDRICAL_SURFACE('',#18375,0.0046);
#3168=CYLINDRICAL_SURFACE('',#18376,0.0046);
#3169=CYLINDRICAL_SURFACE('',#18377,0.010874);
#3170=CYLINDRICAL_SURFACE('',#18378,0.0046);
#3171=CYLINDRICAL_SURFACE('',#18379,0.0046);
#3172=CYLINDRICAL_SURFACE('',#18380,0.010874);
#3173=CYLINDRICAL_SURFACE('',#18381,0.0046);
#3174=CYLINDRICAL_SURFACE('',#18382,0.0046);
#3175=CYLINDRICAL_SURFACE('',#18383,0.010874);
#3176=CYLINDRICAL_SURFACE('',#18384,0.0046);
#3177=CYLINDRICAL_SURFACE('',#18385,0.0046);
#3178=CYLINDRICAL_SURFACE('',#18386,0.010874);
#3179=CYLINDRICAL_SURFACE('',#18387,0.0046);
#3180=CYLINDRICAL_SURFACE('',#18388,0.0046);
#3181=CYLINDRICAL_SURFACE('',#18389,0.010874);
#3182=CYLINDRICAL_SURFACE('',#18390,0.0046);
#3183=CYLINDRICAL_SURFACE('',#18391,0.0046);
#3184=CYLINDRICAL_SURFACE('',#18392,0.010874);
#3185=CYLINDRICAL_SURFACE('',#18393,0.009);
#3186=CYLINDRICAL_SURFACE('',#18395,0.005);
#3187=CYLINDRICAL_SURFACE('',#18400,0.0074756477610481);
#3188=CYLINDRICAL_SURFACE('',#18404,0.00932888901198444);
#3189=CYLINDRICAL_SURFACE('',#18409,0.00932888901198444);
#3190=CYLINDRICAL_SURFACE('',#18418,0.00898940279602035);
#3191=CYLINDRICAL_SURFACE('',#18422,0.00912888901198444);
#3192=CYLINDRICAL_SURFACE('',#18426,0.00932888901198444);
#3193=CYLINDRICAL_SURFACE('',#18430,0.00932888901198444);
#3194=CYLINDRICAL_SURFACE('',#18434,0.00898940279602035);
#3195=CYLINDRICAL_SURFACE('',#18438,0.00912888901198443);
#3196=CYLINDRICAL_SURFACE('',#18442,0.00932888901198444);
#3197=CYLINDRICAL_SURFACE('',#18446,0.0091288890119844);
#3198=CYLINDRICAL_SURFACE('',#18450,0.00932888901198444);
#3199=CYLINDRICAL_SURFACE('',#18454,0.00912888901198441);
#3200=CYLINDRICAL_SURFACE('',#18458,0.00932888901198444);
#3201=CYLINDRICAL_SURFACE('',#18462,0.00912888901198442);
#3202=CYLINDRICAL_SURFACE('',#18466,0.00932888901198444);
#3203=CYLINDRICAL_SURFACE('',#18475,0.0019998995087818);
#3204=CYLINDRICAL_SURFACE('',#18478,0.00199989950878194);
#3205=CYLINDRICAL_SURFACE('',#18525,0.00899250965190647);
#3206=CYLINDRICAL_SURFACE('',#18538,0.00899245661942092);
#3207=CYLINDRICAL_SURFACE('',#18543,0.0208790072664728);
#3208=CYLINDRICAL_SURFACE('',#18544,0.0055);
#3209=CYLINDRICAL_SURFACE('',#18545,0.0055);
#3210=CYLINDRICAL_SURFACE('',#18546,0.0208790057965016);
#3211=CYLINDRICAL_SURFACE('',#18549,0.004);
#3212=CYLINDRICAL_SURFACE('',#18550,0.004);
#3213=CYLINDRICAL_SURFACE('',#18552,0.00816904972011834);
#3214=CYLINDRICAL_SURFACE('',#18554,0.00816904972011834);
#3215=CYLINDRICAL_SURFACE('',#18555,0.00816904972011834);
#3216=CYLINDRICAL_SURFACE('',#18557,0.00816904972011834);
#3217=CYLINDRICAL_SURFACE('',#18581,9.9978220630668E-5);
#3218=CYLINDRICAL_SURFACE('',#18585,9.99782191435892E-5);
#3219=CYLINDRICAL_SURFACE('',#18600,9.9975692043519E-5);
#3220=CYLINDRICAL_SURFACE('',#18603,9.99782206312813E-5);
#3221=CYLINDRICAL_SURFACE('',#18619,0.00922904672092924);
#3222=CYLINDRICAL_SURFACE('',#18620,0.00919655447393812);
#3223=CYLINDRICAL_SURFACE('',#18621,0.00916484752937528);
#3224=CYLINDRICAL_SURFACE('',#18622,0.00913387652341414);
#3225=CYLINDRICAL_SURFACE('',#18623,0.00940354056819424);
#3226=CYLINDRICAL_SURFACE('',#18624,0.0090741001070128);
#3227=CYLINDRICAL_SURFACE('',#18625,0.00893498310288807);
#3228=CYLINDRICAL_SURFACE('',#18626,0.00910365113802367);
#3229=CYLINDRICAL_SURFACE('',#18627,0.00926228971845552);
#3230=CYLINDRICAL_SURFACE('',#18628,0.00929634095813992);
#3231=CYLINDRICAL_SURFACE('',#18629,0.00933121777652104);
#3232=CYLINDRICAL_SURFACE('',#18630,0.00936694531422377);
#3233=CYLINDRICAL_SURFACE('',#18631,0.00896125355933549);
#3234=CYLINDRICAL_SURFACE('',#18632,0.00898813022568495);
#3235=CYLINDRICAL_SURFACE('',#18633,0.0090162483098341);
#3236=CYLINDRICAL_SURFACE('',#18634,0.00904504186665572);
#3237=CYLINDRICAL_SURFACE('',#18635,0.00944176434989097);
#3238=CYLINDRICAL_SURFACE('',#18638,0.00922903063599022);
#3239=CYLINDRICAL_SURFACE('',#18639,0.0091965290470675);
#3240=CYLINDRICAL_SURFACE('',#18640,0.00916482066045435);
#3241=CYLINDRICAL_SURFACE('',#18641,0.00913384823750702);
#3242=CYLINDRICAL_SURFACE('',#18642,0.00940351008025872);
#3243=CYLINDRICAL_SURFACE('',#18643,0.00907404122166741);
#3244=CYLINDRICAL_SURFACE('',#18644,0.00893489737206019);
#3245=CYLINDRICAL_SURFACE('',#18645,0.00910361854634517);
#3246=CYLINDRICAL_SURFACE('',#18646,0.00926227916230088);
#3247=CYLINDRICAL_SURFACE('',#18647,0.0092963345462741);
#3248=CYLINDRICAL_SURFACE('',#18648,0.0093312128177526);
#3249=CYLINDRICAL_SURFACE('',#18649,0.00936693006801195);
#3250=CYLINDRICAL_SURFACE('',#18650,0.00896117725022564);
#3251=CYLINDRICAL_SURFACE('',#18651,0.00898806494315033);
#3252=CYLINDRICAL_SURFACE('',#18652,0.00901619755067071);
#3253=CYLINDRICAL_SURFACE('',#18653,0.00904499652239313);
#3254=CYLINDRICAL_SURFACE('',#18654,0.00944177138396684);
#3255=CYLINDRICAL_SURFACE('',#18657,9.99999926721475E-5);
#3256=CYLINDRICAL_SURFACE('',#18658,9.9999993193412E-5);
#3257=CYLINDRICAL_SURFACE('',#18660,9.99999931392734E-5);
#3258=CYLINDRICAL_SURFACE('',#18661,9.99999934745441E-5);
#3259=CYLINDRICAL_SURFACE('',#18662,9.9999993342419E-5);
#3260=CYLINDRICAL_SURFACE('',#18663,9.99999935401327E-5);
#3261=CYLINDRICAL_SURFACE('',#18664,9.99999931014713E-5);
#3262=CYLINDRICAL_SURFACE('',#18665,9.99999936857353E-5);
#3263=CYLINDRICAL_SURFACE('',#18666,9.99999927304824E-5);
#3264=CYLINDRICAL_SURFACE('',#18667,9.99999928406026E-5);
#3265=CYLINDRICAL_SURFACE('',#18668,9.99999939684521E-5);
#3266=CYLINDRICAL_SURFACE('',#18669,9.99999946770892E-5);
#3267=CYLINDRICAL_SURFACE('',#18670,9.99999905417014E-5);
#3268=CYLINDRICAL_SURFACE('',#18671,9.99999885290244E-5);
#3269=CYLINDRICAL_SURFACE('',#18672,9.99999926628113E-5);
#3270=CYLINDRICAL_SURFACE('',#18673,9.99999939595615E-5);
#3271=CYLINDRICAL_SURFACE('',#18674,9.99999928350082E-5);
#3272=CYLINDRICAL_SURFACE('',#18675,9.99999930681036E-5);
#3273=CYLINDRICAL_SURFACE('',#18676,9.99999927905074E-5);
#3274=CYLINDRICAL_SURFACE('',#18677,9.99999924750999E-5);
#3275=CYLINDRICAL_SURFACE('',#18678,9.99999926945566E-5);
#3276=CYLINDRICAL_SURFACE('',#18679,9.9999992897476E-5);
#3277=CYLINDRICAL_SURFACE('',#18680,9.99999930879845E-5);
#3278=CYLINDRICAL_SURFACE('',#18681,9.99999916320171E-5);
#3279=CYLINDRICAL_SURFACE('',#18682,9.9999990509756E-5);
#3280=CYLINDRICAL_SURFACE('',#18683,9.99999909505769E-5);
#3281=CYLINDRICAL_SURFACE('',#18685,9.99996240727958E-5);
#3282=CYLINDRICAL_SURFACE('',#18686,9.99996321868604E-5);
#3283=CYLINDRICAL_SURFACE('',#18691,9.9999992669382E-5);
#3284=CYLINDRICAL_SURFACE('',#18692,9.99999931979935E-5);
#3285=CYLINDRICAL_SURFACE('',#18693,9.99999931392223E-5);
#3286=CYLINDRICAL_SURFACE('',#18694,9.99999934779342E-5);
#3287=CYLINDRICAL_SURFACE('',#18695,9.9999993345512E-5);
#3288=CYLINDRICAL_SURFACE('',#18696,9.99999935437013E-5);
#3289=CYLINDRICAL_SURFACE('',#18697,9.99999931072116E-5);
#3290=CYLINDRICAL_SURFACE('',#18698,9.99999936854522E-5);
#3291=CYLINDRICAL_SURFACE('',#18699,9.99999927924378E-5);
#3292=CYLINDRICAL_SURFACE('',#18700,9.99999928656628E-5);
#3293=CYLINDRICAL_SURFACE('',#18701,9.99999939755481E-5);
#3294=CYLINDRICAL_SURFACE('',#18702,9.9999994677093E-5);
#3295=CYLINDRICAL_SURFACE('',#18703,9.99999905763174E-5);
#3296=CYLINDRICAL_SURFACE('',#18704,9.9999988507358E-5);
#3297=CYLINDRICAL_SURFACE('',#18705,9.99999926697609E-5);
#3298=CYLINDRICAL_SURFACE('',#18706,9.99999939599216E-5);
#3299=CYLINDRICAL_SURFACE('',#18707,9.99999928286534E-5);
#3300=CYLINDRICAL_SURFACE('',#18708,9.99999930733179E-5);
#3301=CYLINDRICAL_SURFACE('',#18709,9.99999927766249E-5);
#3302=CYLINDRICAL_SURFACE('',#18710,9.99999924822146E-5);
#3303=CYLINDRICAL_SURFACE('',#18711,9.9999992646252E-5);
#3304=CYLINDRICAL_SURFACE('',#18712,9.99999929064612E-5);
#3305=CYLINDRICAL_SURFACE('',#18713,9.99999929016321E-5);
#3306=CYLINDRICAL_SURFACE('',#18714,9.99999916467037E-5);
#3307=CYLINDRICAL_SURFACE('',#18715,9.99999905246489E-5);
#3308=CYLINDRICAL_SURFACE('',#18716,9.99999909501884E-5);
#3309=CYLINDRICAL_SURFACE('',#18718,9.99996239781536E-5);
#3310=CYLINDRICAL_SURFACE('',#18719,9.99996322518559E-5);
#3311=CYLINDRICAL_SURFACE('',#18726,9.99999890432553E-5);
#3312=CYLINDRICAL_SURFACE('',#18732,9.99999916933113E-5);
#3313=CYLINDRICAL_SURFACE('',#18737,9.99999916975992E-5);
#3314=CYLINDRICAL_SURFACE('',#18743,9.99999890830763E-5);
#3315=CYLINDRICAL_SURFACE('',#18760,0.0055);
#3316=CYLINDRICAL_SURFACE('',#18774,0.017);
#3317=CYLINDRICAL_SURFACE('',#18775,0.017);
#3318=CYLINDRICAL_SURFACE('',#18776,0.017);
#3319=CYLINDRICAL_SURFACE('',#18777,0.017);
#3320=CYLINDRICAL_SURFACE('',#18778,0.0005);
#3321=CYLINDRICAL_SURFACE('',#18779,0.0005);
#3322=CYLINDRICAL_SURFACE('',#18780,0.0005);
#3323=CYLINDRICAL_SURFACE('',#18781,0.0005);
#3324=CYLINDRICAL_SURFACE('',#18782,0.00278445714771807);
#3325=CYLINDRICAL_SURFACE('',#18790,0.00116635989804114);
#3326=CYLINDRICAL_SURFACE('',#18795,0.00184479343283513);
#3327=CYLINDRICAL_SURFACE('',#18796,0.00134583534834952);
#3328=CYLINDRICAL_SURFACE('',#18803,0.00125);
#3329=CYLINDRICAL_SURFACE('',#18832,0.0015);
#3330=CYLINDRICAL_SURFACE('',#18840,0.0005);
#3331=CYLINDRICAL_SURFACE('',#18844,0.0001);
#3332=CYLINDRICAL_SURFACE('',#18847,0.0001);
#3333=CYLINDRICAL_SURFACE('',#18849,0.0001);
#3334=CYLINDRICAL_SURFACE('',#18852,0.0001);
#3335=CYLINDRICAL_SURFACE('',#18854,0.0001);
#3336=CYLINDRICAL_SURFACE('',#18856,0.0001);
#3337=CYLINDRICAL_SURFACE('',#18858,0.0001);
#3338=CYLINDRICAL_SURFACE('',#18860,0.0001);
#3339=CYLINDRICAL_SURFACE('',#18862,0.0001);
#3340=CYLINDRICAL_SURFACE('',#18864,0.0001);
#3341=CYLINDRICAL_SURFACE('',#18866,0.0001);
#3342=CYLINDRICAL_SURFACE('',#18868,0.0001);
#3343=CYLINDRICAL_SURFACE('',#18870,0.0001);
#3344=CYLINDRICAL_SURFACE('',#18872,0.0001);
#3345=CYLINDRICAL_SURFACE('',#18874,0.0001);
#3346=CYLINDRICAL_SURFACE('',#18876,0.0001);
#3347=CYLINDRICAL_SURFACE('',#18878,0.0001);
#3348=CYLINDRICAL_SURFACE('',#18880,0.0001);
#3349=CYLINDRICAL_SURFACE('',#18882,0.0001);
#3350=CYLINDRICAL_SURFACE('',#18884,0.0001);
#3351=CYLINDRICAL_SURFACE('',#18886,0.0001);
#3352=CYLINDRICAL_SURFACE('',#18888,0.0001);
#3353=CYLINDRICAL_SURFACE('',#18890,0.0001);
#3354=CYLINDRICAL_SURFACE('',#18893,0.0001);
#3355=CYLINDRICAL_SURFACE('',#18895,0.0001);
#3356=CYLINDRICAL_SURFACE('',#18897,0.0001);
#3357=CYLINDRICAL_SURFACE('',#18903,0.0001);
#3358=CYLINDRICAL_SURFACE('',#18905,0.0001);
#3359=CYLINDRICAL_SURFACE('',#18911,0.0001);
#3360=CYLINDRICAL_SURFACE('',#18917,0.0001);
#3361=CYLINDRICAL_SURFACE('',#18923,0.0015);
#3362=CYLINDRICAL_SURFACE('',#18952,0.0005);
#3363=CYLINDRICAL_SURFACE('',#18956,0.0001);
#3364=CYLINDRICAL_SURFACE('',#18959,0.0001);
#3365=CYLINDRICAL_SURFACE('',#18961,0.0001);
#3366=CYLINDRICAL_SURFACE('',#18964,0.0001);
#3367=CYLINDRICAL_SURFACE('',#18966,0.0001);
#3368=CYLINDRICAL_SURFACE('',#18968,0.0001);
#3369=CYLINDRICAL_SURFACE('',#18970,0.0001);
#3370=CYLINDRICAL_SURFACE('',#18972,0.0001);
#3371=CYLINDRICAL_SURFACE('',#18974,0.0001);
#3372=CYLINDRICAL_SURFACE('',#18976,0.0001);
#3373=CYLINDRICAL_SURFACE('',#18978,0.0001);
#3374=CYLINDRICAL_SURFACE('',#18980,0.0001);
#3375=CYLINDRICAL_SURFACE('',#18982,0.0001);
#3376=CYLINDRICAL_SURFACE('',#18984,0.0001);
#3377=CYLINDRICAL_SURFACE('',#18986,0.0001);
#3378=CYLINDRICAL_SURFACE('',#18988,0.0001);
#3379=CYLINDRICAL_SURFACE('',#18990,0.0001);
#3380=CYLINDRICAL_SURFACE('',#18992,0.0001);
#3381=CYLINDRICAL_SURFACE('',#18994,0.0001);
#3382=CYLINDRICAL_SURFACE('',#18997,0.0001);
#3383=CYLINDRICAL_SURFACE('',#18999,0.0001);
#3384=CYLINDRICAL_SURFACE('',#19001,0.0001);
#3385=CYLINDRICAL_SURFACE('',#19007,0.0001);
#3386=CYLINDRICAL_SURFACE('',#19009,0.0001);
#3387=CYLINDRICAL_SURFACE('',#19011,0.0001);
#3388=CYLINDRICAL_SURFACE('',#19013,0.0001);
#3389=CYLINDRICAL_SURFACE('',#19016,0.0001);
#3390=CYLINDRICAL_SURFACE('',#19018,0.0001);
#3391=CYLINDRICAL_SURFACE('',#19020,0.0001);
#3392=CYLINDRICAL_SURFACE('',#19031,0.0001);
#3393=CYLINDRICAL_SURFACE('',#19037,0.0001);
#3394=CYLINDRICAL_SURFACE('',#19043,0.0001);
#3395=CYLINDRICAL_SURFACE('',#19049,0.0011);
#3396=CYLINDRICAL_SURFACE('',#19053,0.0005);
#3397=CYLINDRICAL_SURFACE('',#19057,0.00125);
#3398=CYLINDRICAL_SURFACE('',#19067,0.009);
#3399=CYLINDRICAL_SURFACE('',#19074,0.0055);
#3400=CYLINDRICAL_SURFACE('',#19108,0.002);
#3401=CYLINDRICAL_SURFACE('',#19111,0.001);
#3402=CYLINDRICAL_SURFACE('',#19139,0.0135);
#3403=CYLINDRICAL_SURFACE('',#19142,0.0135);
#3404=CYLINDRICAL_SURFACE('',#19159,0.009);
#3405=CYLINDRICAL_SURFACE('',#19164,0.0012);
#3406=CYLINDRICAL_SURFACE('',#19169,0.0005);
#3407=CYLINDRICAL_SURFACE('',#19174,0.0005);
#3408=CYLINDRICAL_SURFACE('',#19200,0.00240582032312608);
#3409=CYLINDRICAL_SURFACE('',#19205,0.00265162305984738);
#3410=CYLINDRICAL_SURFACE('',#19210,0.00240582032360216);
#3411=CYLINDRICAL_SURFACE('',#19213,0.00170789487802692);
#3412=CYLINDRICAL_SURFACE('',#19228,0.001);
#3413=CYLINDRICAL_SURFACE('',#19233,0.0001);
#3414=CYLINDRICAL_SURFACE('',#19241,0.0001);
#3415=CYLINDRICAL_SURFACE('',#19244,0.0001);
#3416=CYLINDRICAL_SURFACE('',#19246,0.0001);
#3417=CYLINDRICAL_SURFACE('',#19248,0.0001);
#3418=CYLINDRICAL_SURFACE('',#19260,0.0001);
#3419=CYLINDRICAL_SURFACE('',#19264,0.0001);
#3420=CYLINDRICAL_SURFACE('',#19266,0.0001);
#3421=CYLINDRICAL_SURFACE('',#19278,0.0001);
#3422=CYLINDRICAL_SURFACE('',#19280,0.0001);
#3423=CYLINDRICAL_SURFACE('',#19282,0.0001);
#3424=CYLINDRICAL_SURFACE('',#19288,0.0001);
#3425=CYLINDRICAL_SURFACE('',#19294,0.0125);
#3426=CYLINDRICAL_SURFACE('',#19298,0.001);
#3427=CYLINDRICAL_SURFACE('',#19301,0.0132323601801219);
#3428=CYLINDRICAL_SURFACE('',#19304,0.0132323601801219);
#3429=CYLINDRICAL_SURFACE('',#19322,0.0125);
#3430=CYLINDRICAL_SURFACE('',#19324,0.0125);
#3431=CYLINDRICAL_SURFACE('',#19327,0.005);
#3432=CYLINDRICAL_SURFACE('',#19334,0.0165);
#3433=CYLINDRICAL_SURFACE('',#19338,0.0165);
#3434=CYLINDRICAL_SURFACE('',#19342,0.0165);
#3435=CYLINDRICAL_SURFACE('',#19359,0.0135);
#3436=CYLINDRICAL_SURFACE('',#19362,0.0135);
#3437=CYLINDRICAL_SURFACE('',#19380,0.009);
#3438=CYLINDRICAL_SURFACE('',#19396,0.0132323601801219);
#3439=CYLINDRICAL_SURFACE('',#19399,0.0015);
#3440=CYLINDRICAL_SURFACE('',#19401,0.0015);
#3441=CYLINDRICAL_SURFACE('',#19408,0.0025);
#3442=CYLINDRICAL_SURFACE('',#19427,0.0002);
#3443=CYLINDRICAL_SURFACE('',#19433,0.0002);
#3444=CYLINDRICAL_SURFACE('',#19446,0.0002);
#3445=CYLINDRICAL_SURFACE('',#19447,0.0002);
#3446=CYLINDRICAL_SURFACE('',#19459,0.0002);
#3447=CYLINDRICAL_SURFACE('',#19463,0.0002);
#3448=CYLINDRICAL_SURFACE('',#19465,0.0002);
#3449=CYLINDRICAL_SURFACE('',#19467,0.0002);
#3450=CYLINDRICAL_SURFACE('',#19477,0.0002);
#3451=CYLINDRICAL_SURFACE('',#19481,0.0002);
#3452=CYLINDRICAL_SURFACE('',#19483,0.0002);
#3453=CYLINDRICAL_SURFACE('',#19491,0.0002);
#3454=CYLINDRICAL_SURFACE('',#19493,0.0002);
#3455=CYLINDRICAL_SURFACE('',#19495,0.0002);
#3456=CYLINDRICAL_SURFACE('',#19497,0.0002);
#3457=CYLINDRICAL_SURFACE('',#19502,0.0002);
#3458=CYLINDRICAL_SURFACE('',#19509,0.0002);
#3459=CYLINDRICAL_SURFACE('',#19516,0.0002);
#3460=CYLINDRICAL_SURFACE('',#19521,0.0002);
#3461=CYLINDRICAL_SURFACE('',#19523,0.0002);
#3462=CYLINDRICAL_SURFACE('',#19541,0.0002);
#3463=CYLINDRICAL_SURFACE('',#19544,0.0002);
#3464=CYLINDRICAL_SURFACE('',#19551,0.00199545322288878);
#3465=CYLINDRICAL_SURFACE('',#19553,0.0017588879999111);
#3466=CYLINDRICAL_SURFACE('',#19557,0.000202286544194825);
#3467=CYLINDRICAL_SURFACE('',#19558,0.000203651032597172);
#3468=CYLINDRICAL_SURFACE('',#19562,0.0019892004500739);
#3469=CYLINDRICAL_SURFACE('',#19564,0.00197736746715445);
#3470=CYLINDRICAL_SURFACE('',#19566,0.00199576483991537);
#3471=CYLINDRICAL_SURFACE('',#19570,0.000200921696200641);
#3472=CYLINDRICAL_SURFACE('',#19571,0.0005);
#3473=CYLINDRICAL_SURFACE('',#19572,0.0005);
#3474=CYLINDRICAL_SURFACE('',#19573,0.0005);
#3475=CYLINDRICAL_SURFACE('',#19574,0.0005);
#3476=CYLINDRICAL_SURFACE('',#19583,0.0005);
#3477=FACE_BOUND('',#4551,.T.);
#3478=FACE_BOUND('',#4598,.T.);
#3479=FACE_BOUND('',#4746,.T.);
#3480=FACE_BOUND('',#4748,.T.);
#3481=FACE_BOUND('',#4764,.T.);
#3482=FACE_BOUND('',#4796,.T.);
#3483=FACE_BOUND('',#4797,.T.);
#3484=FACE_BOUND('',#4801,.T.);
#3485=FACE_BOUND('',#4802,.T.);
#3486=FACE_BOUND('',#4803,.T.);
#3487=FACE_BOUND('',#4804,.T.);
#3488=FACE_BOUND('',#4805,.T.);
#3489=FACE_BOUND('',#4806,.T.);
#3490=FACE_BOUND('',#4807,.T.);
#3491=FACE_BOUND('',#4808,.T.);
#3492=FACE_BOUND('',#4809,.T.);
#3493=FACE_BOUND('',#4810,.T.);
#3494=FACE_BOUND('',#4811,.T.);
#3495=FACE_BOUND('',#4812,.T.);
#3496=FACE_BOUND('',#4813,.T.);
#3497=FACE_BOUND('',#4814,.T.);
#3498=FACE_BOUND('',#4815,.T.);
#3499=FACE_BOUND('',#4816,.T.);
#3500=FACE_BOUND('',#4817,.T.);
#3501=FACE_BOUND('',#5171,.T.);
#3502=FACE_BOUND('',#5175,.T.);
#3503=FACE_BOUND('',#5178,.T.);
#3504=FACE_BOUND('',#5187,.T.);
#3505=FACE_BOUND('',#5194,.T.);
#3506=FACE_BOUND('',#5205,.T.);
#3507=FACE_BOUND('',#5207,.T.);
#3508=FACE_BOUND('',#5278,.T.);
#3509=FACE_BOUND('',#5280,.T.);
#3510=FACE_BOUND('',#5333,.T.);
#3511=FACE_BOUND('',#5336,.T.);
#3512=FACE_BOUND('',#5339,.T.);
#3513=FACE_BOUND('',#5345,.T.);
#3514=FACE_BOUND('',#5375,.T.);
#3515=FACE_BOUND('',#5376,.T.);
#3516=FACE_BOUND('',#5377,.T.);
#3517=FACE_BOUND('',#5378,.T.);
#3518=FACE_BOUND('',#5380,.T.);
#3519=FACE_BOUND('',#5381,.T.);
#3520=FACE_BOUND('',#5382,.T.);
#3521=FACE_BOUND('',#5383,.T.);
#3522=FACE_BOUND('',#5409,.T.);
#3523=FACE_BOUND('',#5411,.T.);
#3524=FACE_BOUND('',#5453,.T.);
#3525=FACE_BOUND('',#5454,.T.);
#3526=FACE_BOUND('',#5455,.T.);
#3527=FACE_BOUND('',#5456,.T.);
#3528=FACE_BOUND('',#5457,.T.);
#3529=FACE_BOUND('',#5461,.T.);
#3530=FACE_BOUND('',#5462,.T.);
#3531=FACE_BOUND('',#5463,.T.);
#3532=FACE_BOUND('',#5464,.T.);
#3533=FACE_BOUND('',#5465,.T.);
#3534=FACE_BOUND('',#5472,.T.);
#3535=FACE_BOUND('',#5473,.T.);
#3536=FACE_BOUND('',#5474,.T.);
#3537=FACE_BOUND('',#5476,.T.);
#3538=FACE_BOUND('',#5480,.T.);
#3539=FACE_BOUND('',#5482,.T.);
#3540=FACE_BOUND('',#5501,.T.);
#3541=FACE_BOUND('',#5502,.T.);
#3542=FACE_BOUND('',#5503,.T.);
#3543=FACE_BOUND('',#5622,.T.);
#3544=FACE_OUTER_BOUND('',#4550,.T.);
#3545=FACE_OUTER_BOUND('',#4552,.T.);
#3546=FACE_OUTER_BOUND('',#4553,.T.);
#3547=FACE_OUTER_BOUND('',#4554,.T.);
#3548=FACE_OUTER_BOUND('',#4555,.T.);
#3549=FACE_OUTER_BOUND('',#4556,.T.);
#3550=FACE_OUTER_BOUND('',#4557,.T.);
#3551=FACE_OUTER_BOUND('',#4558,.T.);
#3552=FACE_OUTER_BOUND('',#4559,.T.);
#3553=FACE_OUTER_BOUND('',#4560,.T.);
#3554=FACE_OUTER_BOUND('',#4561,.T.);
#3555=FACE_OUTER_BOUND('',#4562,.T.);
#3556=FACE_OUTER_BOUND('',#4563,.T.);
#3557=FACE_OUTER_BOUND('',#4564,.T.);
#3558=FACE_OUTER_BOUND('',#4565,.T.);
#3559=FACE_OUTER_BOUND('',#4566,.T.);
#3560=FACE_OUTER_BOUND('',#4567,.T.);
#3561=FACE_OUTER_BOUND('',#4568,.T.);
#3562=FACE_OUTER_BOUND('',#4569,.T.);
#3563=FACE_OUTER_BOUND('',#4570,.T.);
#3564=FACE_OUTER_BOUND('',#4571,.T.);
#3565=FACE_OUTER_BOUND('',#4572,.T.);
#3566=FACE_OUTER_BOUND('',#4573,.T.);
#3567=FACE_OUTER_BOUND('',#4574,.T.);
#3568=FACE_OUTER_BOUND('',#4575,.T.);
#3569=FACE_OUTER_BOUND('',#4576,.T.);
#3570=FACE_OUTER_BOUND('',#4577,.T.);
#3571=FACE_OUTER_BOUND('',#4578,.T.);
#3572=FACE_OUTER_BOUND('',#4579,.T.);
#3573=FACE_OUTER_BOUND('',#4580,.T.);
#3574=FACE_OUTER_BOUND('',#4581,.T.);
#3575=FACE_OUTER_BOUND('',#4582,.T.);
#3576=FACE_OUTER_BOUND('',#4583,.T.);
#3577=FACE_OUTER_BOUND('',#4584,.T.);
#3578=FACE_OUTER_BOUND('',#4585,.T.);
#3579=FACE_OUTER_BOUND('',#4586,.T.);
#3580=FACE_OUTER_BOUND('',#4587,.T.);
#3581=FACE_OUTER_BOUND('',#4588,.T.);
#3582=FACE_OUTER_BOUND('',#4589,.T.);
#3583=FACE_OUTER_BOUND('',#4590,.T.);
#3584=FACE_OUTER_BOUND('',#4591,.T.);
#3585=FACE_OUTER_BOUND('',#4592,.T.);
#3586=FACE_OUTER_BOUND('',#4593,.T.);
#3587=FACE_OUTER_BOUND('',#4594,.T.);
#3588=FACE_OUTER_BOUND('',#4595,.T.);
#3589=FACE_OUTER_BOUND('',#4596,.T.);
#3590=FACE_OUTER_BOUND('',#4597,.T.);
#3591=FACE_OUTER_BOUND('',#4599,.T.);
#3592=FACE_OUTER_BOUND('',#4600,.T.);
#3593=FACE_OUTER_BOUND('',#4601,.T.);
#3594=FACE_OUTER_BOUND('',#4602,.T.);
#3595=FACE_OUTER_BOUND('',#4603,.T.);
#3596=FACE_OUTER_BOUND('',#4604,.T.);
#3597=FACE_OUTER_BOUND('',#4605,.T.);
#3598=FACE_OUTER_BOUND('',#4606,.T.);
#3599=FACE_OUTER_BOUND('',#4607,.T.);
#3600=FACE_OUTER_BOUND('',#4608,.T.);
#3601=FACE_OUTER_BOUND('',#4609,.T.);
#3602=FACE_OUTER_BOUND('',#4610,.T.);
#3603=FACE_OUTER_BOUND('',#4611,.T.);
#3604=FACE_OUTER_BOUND('',#4612,.T.);
#3605=FACE_OUTER_BOUND('',#4613,.T.);
#3606=FACE_OUTER_BOUND('',#4614,.T.);
#3607=FACE_OUTER_BOUND('',#4615,.T.);
#3608=FACE_OUTER_BOUND('',#4616,.T.);
#3609=FACE_OUTER_BOUND('',#4617,.T.);
#3610=FACE_OUTER_BOUND('',#4618,.T.);
#3611=FACE_OUTER_BOUND('',#4619,.T.);
#3612=FACE_OUTER_BOUND('',#4620,.T.);
#3613=FACE_OUTER_BOUND('',#4621,.T.);
#3614=FACE_OUTER_BOUND('',#4622,.T.);
#3615=FACE_OUTER_BOUND('',#4623,.T.);
#3616=FACE_OUTER_BOUND('',#4624,.T.);
#3617=FACE_OUTER_BOUND('',#4625,.T.);
#3618=FACE_OUTER_BOUND('',#4626,.T.);
#3619=FACE_OUTER_BOUND('',#4627,.T.);
#3620=FACE_OUTER_BOUND('',#4628,.T.);
#3621=FACE_OUTER_BOUND('',#4629,.T.);
#3622=FACE_OUTER_BOUND('',#4630,.T.);
#3623=FACE_OUTER_BOUND('',#4631,.T.);
#3624=FACE_OUTER_BOUND('',#4632,.T.);
#3625=FACE_OUTER_BOUND('',#4633,.T.);
#3626=FACE_OUTER_BOUND('',#4634,.T.);
#3627=FACE_OUTER_BOUND('',#4635,.T.);
#3628=FACE_OUTER_BOUND('',#4636,.T.);
#3629=FACE_OUTER_BOUND('',#4637,.T.);
#3630=FACE_OUTER_BOUND('',#4638,.T.);
#3631=FACE_OUTER_BOUND('',#4639,.T.);
#3632=FACE_OUTER_BOUND('',#4640,.T.);
#3633=FACE_OUTER_BOUND('',#4641,.T.);
#3634=FACE_OUTER_BOUND('',#4642,.T.);
#3635=FACE_OUTER_BOUND('',#4643,.T.);
#3636=FACE_OUTER_BOUND('',#4644,.T.);
#3637=FACE_OUTER_BOUND('',#4645,.T.);
#3638=FACE_OUTER_BOUND('',#4646,.T.);
#3639=FACE_OUTER_BOUND('',#4647,.T.);
#3640=FACE_OUTER_BOUND('',#4648,.T.);
#3641=FACE_OUTER_BOUND('',#4649,.T.);
#3642=FACE_OUTER_BOUND('',#4650,.T.);
#3643=FACE_OUTER_BOUND('',#4651,.T.);
#3644=FACE_OUTER_BOUND('',#4652,.T.);
#3645=FACE_OUTER_BOUND('',#4653,.T.);
#3646=FACE_OUTER_BOUND('',#4654,.T.);
#3647=FACE_OUTER_BOUND('',#4655,.T.);
#3648=FACE_OUTER_BOUND('',#4656,.T.);
#3649=FACE_OUTER_BOUND('',#4657,.T.);
#3650=FACE_OUTER_BOUND('',#4658,.T.);
#3651=FACE_OUTER_BOUND('',#4659,.T.);
#3652=FACE_OUTER_BOUND('',#4660,.T.);
#3653=FACE_OUTER_BOUND('',#4661,.T.);
#3654=FACE_OUTER_BOUND('',#4662,.T.);
#3655=FACE_OUTER_BOUND('',#4663,.T.);
#3656=FACE_OUTER_BOUND('',#4664,.T.);
#3657=FACE_OUTER_BOUND('',#4665,.T.);
#3658=FACE_OUTER_BOUND('',#4666,.T.);
#3659=FACE_OUTER_BOUND('',#4667,.T.);
#3660=FACE_OUTER_BOUND('',#4668,.T.);
#3661=FACE_OUTER_BOUND('',#4669,.T.);
#3662=FACE_OUTER_BOUND('',#4670,.T.);
#3663=FACE_OUTER_BOUND('',#4671,.T.);
#3664=FACE_OUTER_BOUND('',#4672,.T.);
#3665=FACE_OUTER_BOUND('',#4673,.T.);
#3666=FACE_OUTER_BOUND('',#4674,.T.);
#3667=FACE_OUTER_BOUND('',#4675,.T.);
#3668=FACE_OUTER_BOUND('',#4676,.T.);
#3669=FACE_OUTER_BOUND('',#4677,.T.);
#3670=FACE_OUTER_BOUND('',#4678,.T.);
#3671=FACE_OUTER_BOUND('',#4679,.T.);
#3672=FACE_OUTER_BOUND('',#4680,.T.);
#3673=FACE_OUTER_BOUND('',#4681,.T.);
#3674=FACE_OUTER_BOUND('',#4682,.T.);
#3675=FACE_OUTER_BOUND('',#4683,.T.);
#3676=FACE_OUTER_BOUND('',#4684,.T.);
#3677=FACE_OUTER_BOUND('',#4685,.T.);
#3678=FACE_OUTER_BOUND('',#4686,.T.);
#3679=FACE_OUTER_BOUND('',#4687,.T.);
#3680=FACE_OUTER_BOUND('',#4688,.T.);
#3681=FACE_OUTER_BOUND('',#4689,.T.);
#3682=FACE_OUTER_BOUND('',#4690,.T.);
#3683=FACE_OUTER_BOUND('',#4691,.T.);
#3684=FACE_OUTER_BOUND('',#4692,.T.);
#3685=FACE_OUTER_BOUND('',#4693,.T.);
#3686=FACE_OUTER_BOUND('',#4694,.T.);
#3687=FACE_OUTER_BOUND('',#4695,.T.);
#3688=FACE_OUTER_BOUND('',#4696,.T.);
#3689=FACE_OUTER_BOUND('',#4697,.T.);
#3690=FACE_OUTER_BOUND('',#4698,.T.);
#3691=FACE_OUTER_BOUND('',#4699,.T.);
#3692=FACE_OUTER_BOUND('',#4700,.T.);
#3693=FACE_OUTER_BOUND('',#4701,.T.);
#3694=FACE_OUTER_BOUND('',#4702,.T.);
#3695=FACE_OUTER_BOUND('',#4703,.T.);
#3696=FACE_OUTER_BOUND('',#4704,.T.);
#3697=FACE_OUTER_BOUND('',#4705,.T.);
#3698=FACE_OUTER_BOUND('',#4706,.T.);
#3699=FACE_OUTER_BOUND('',#4707,.T.);
#3700=FACE_OUTER_BOUND('',#4708,.T.);
#3701=FACE_OUTER_BOUND('',#4709,.T.);
#3702=FACE_OUTER_BOUND('',#4710,.T.);
#3703=FACE_OUTER_BOUND('',#4711,.T.);
#3704=FACE_OUTER_BOUND('',#4712,.T.);
#3705=FACE_OUTER_BOUND('',#4713,.T.);
#3706=FACE_OUTER_BOUND('',#4714,.T.);
#3707=FACE_OUTER_BOUND('',#4715,.T.);
#3708=FACE_OUTER_BOUND('',#4716,.T.);
#3709=FACE_OUTER_BOUND('',#4717,.T.);
#3710=FACE_OUTER_BOUND('',#4718,.T.);
#3711=FACE_OUTER_BOUND('',#4719,.T.);
#3712=FACE_OUTER_BOUND('',#4720,.T.);
#3713=FACE_OUTER_BOUND('',#4721,.T.);
#3714=FACE_OUTER_BOUND('',#4722,.T.);
#3715=FACE_OUTER_BOUND('',#4723,.T.);
#3716=FACE_OUTER_BOUND('',#4724,.T.);
#3717=FACE_OUTER_BOUND('',#4725,.T.);
#3718=FACE_OUTER_BOUND('',#4726,.T.);
#3719=FACE_OUTER_BOUND('',#4727,.T.);
#3720=FACE_OUTER_BOUND('',#4728,.T.);
#3721=FACE_OUTER_BOUND('',#4729,.T.);
#3722=FACE_OUTER_BOUND('',#4730,.T.);
#3723=FACE_OUTER_BOUND('',#4731,.T.);
#3724=FACE_OUTER_BOUND('',#4732,.T.);
#3725=FACE_OUTER_BOUND('',#4733,.T.);
#3726=FACE_OUTER_BOUND('',#4734,.T.);
#3727=FACE_OUTER_BOUND('',#4735,.T.);
#3728=FACE_OUTER_BOUND('',#4736,.T.);
#3729=FACE_OUTER_BOUND('',#4737,.T.);
#3730=FACE_OUTER_BOUND('',#4738,.T.);
#3731=FACE_OUTER_BOUND('',#4739,.T.);
#3732=FACE_OUTER_BOUND('',#4740,.T.);
#3733=FACE_OUTER_BOUND('',#4741,.T.);
#3734=FACE_OUTER_BOUND('',#4742,.T.);
#3735=FACE_OUTER_BOUND('',#4743,.T.);
#3736=FACE_OUTER_BOUND('',#4744,.T.);
#3737=FACE_OUTER_BOUND('',#4745,.T.);
#3738=FACE_OUTER_BOUND('',#4747,.T.);
#3739=FACE_OUTER_BOUND('',#4749,.T.);
#3740=FACE_OUTER_BOUND('',#4750,.T.);
#3741=FACE_OUTER_BOUND('',#4751,.T.);
#3742=FACE_OUTER_BOUND('',#4752,.T.);
#3743=FACE_OUTER_BOUND('',#4753,.T.);
#3744=FACE_OUTER_BOUND('',#4754,.T.);
#3745=FACE_OUTER_BOUND('',#4755,.T.);
#3746=FACE_OUTER_BOUND('',#4756,.T.);
#3747=FACE_OUTER_BOUND('',#4757,.T.);
#3748=FACE_OUTER_BOUND('',#4758,.T.);
#3749=FACE_OUTER_BOUND('',#4759,.T.);
#3750=FACE_OUTER_BOUND('',#4760,.T.);
#3751=FACE_OUTER_BOUND('',#4761,.T.);
#3752=FACE_OUTER_BOUND('',#4762,.T.);
#3753=FACE_OUTER_BOUND('',#4763,.T.);
#3754=FACE_OUTER_BOUND('',#4765,.T.);
#3755=FACE_OUTER_BOUND('',#4766,.T.);
#3756=FACE_OUTER_BOUND('',#4767,.T.);
#3757=FACE_OUTER_BOUND('',#4768,.T.);
#3758=FACE_OUTER_BOUND('',#4769,.T.);
#3759=FACE_OUTER_BOUND('',#4770,.T.);
#3760=FACE_OUTER_BOUND('',#4771,.T.);
#3761=FACE_OUTER_BOUND('',#4772,.T.);
#3762=FACE_OUTER_BOUND('',#4773,.T.);
#3763=FACE_OUTER_BOUND('',#4774,.T.);
#3764=FACE_OUTER_BOUND('',#4775,.T.);
#3765=FACE_OUTER_BOUND('',#4776,.T.);
#3766=FACE_OUTER_BOUND('',#4777,.T.);
#3767=FACE_OUTER_BOUND('',#4778,.T.);
#3768=FACE_OUTER_BOUND('',#4779,.T.);
#3769=FACE_OUTER_BOUND('',#4780,.T.);
#3770=FACE_OUTER_BOUND('',#4781,.T.);
#3771=FACE_OUTER_BOUND('',#4782,.T.);
#3772=FACE_OUTER_BOUND('',#4783,.T.);
#3773=FACE_OUTER_BOUND('',#4784,.T.);
#3774=FACE_OUTER_BOUND('',#4785,.T.);
#3775=FACE_OUTER_BOUND('',#4786,.T.);
#3776=FACE_OUTER_BOUND('',#4787,.T.);
#3777=FACE_OUTER_BOUND('',#4788,.T.);
#3778=FACE_OUTER_BOUND('',#4789,.T.);
#3779=FACE_OUTER_BOUND('',#4790,.T.);
#3780=FACE_OUTER_BOUND('',#4791,.T.);
#3781=FACE_OUTER_BOUND('',#4792,.T.);
#3782=FACE_OUTER_BOUND('',#4793,.T.);
#3783=FACE_OUTER_BOUND('',#4794,.T.);
#3784=FACE_OUTER_BOUND('',#4795,.T.);
#3785=FACE_OUTER_BOUND('',#4798,.T.);
#3786=FACE_OUTER_BOUND('',#4799,.T.);
#3787=FACE_OUTER_BOUND('',#4800,.T.);
#3788=FACE_OUTER_BOUND('',#4818,.T.);
#3789=FACE_OUTER_BOUND('',#4819,.T.);
#3790=FACE_OUTER_BOUND('',#4820,.T.);
#3791=FACE_OUTER_BOUND('',#4821,.T.);
#3792=FACE_OUTER_BOUND('',#4822,.T.);
#3793=FACE_OUTER_BOUND('',#4823,.T.);
#3794=FACE_OUTER_BOUND('',#4824,.T.);
#3795=FACE_OUTER_BOUND('',#4825,.T.);
#3796=FACE_OUTER_BOUND('',#4826,.T.);
#3797=FACE_OUTER_BOUND('',#4827,.T.);
#3798=FACE_OUTER_BOUND('',#4828,.T.);
#3799=FACE_OUTER_BOUND('',#4829,.T.);
#3800=FACE_OUTER_BOUND('',#4830,.T.);
#3801=FACE_OUTER_BOUND('',#4831,.T.);
#3802=FACE_OUTER_BOUND('',#4832,.T.);
#3803=FACE_OUTER_BOUND('',#4833,.T.);
#3804=FACE_OUTER_BOUND('',#4834,.T.);
#3805=FACE_OUTER_BOUND('',#4835,.T.);
#3806=FACE_OUTER_BOUND('',#4836,.T.);
#3807=FACE_OUTER_BOUND('',#4837,.T.);
#3808=FACE_OUTER_BOUND('',#4838,.T.);
#3809=FACE_OUTER_BOUND('',#4839,.T.);
#3810=FACE_OUTER_BOUND('',#4840,.T.);
#3811=FACE_OUTER_BOUND('',#4841,.T.);
#3812=FACE_OUTER_BOUND('',#4842,.T.);
#3813=FACE_OUTER_BOUND('',#4843,.T.);
#3814=FACE_OUTER_BOUND('',#4844,.T.);
#3815=FACE_OUTER_BOUND('',#4845,.T.);
#3816=FACE_OUTER_BOUND('',#4846,.T.);
#3817=FACE_OUTER_BOUND('',#4847,.T.);
#3818=FACE_OUTER_BOUND('',#4848,.T.);
#3819=FACE_OUTER_BOUND('',#4849,.T.);
#3820=FACE_OUTER_BOUND('',#4850,.T.);
#3821=FACE_OUTER_BOUND('',#4851,.T.);
#3822=FACE_OUTER_BOUND('',#4852,.T.);
#3823=FACE_OUTER_BOUND('',#4853,.T.);
#3824=FACE_OUTER_BOUND('',#4854,.T.);
#3825=FACE_OUTER_BOUND('',#4855,.T.);
#3826=FACE_OUTER_BOUND('',#4856,.T.);
#3827=FACE_OUTER_BOUND('',#4857,.T.);
#3828=FACE_OUTER_BOUND('',#4858,.T.);
#3829=FACE_OUTER_BOUND('',#4859,.T.);
#3830=FACE_OUTER_BOUND('',#4860,.T.);
#3831=FACE_OUTER_BOUND('',#4861,.T.);
#3832=FACE_OUTER_BOUND('',#4862,.T.);
#3833=FACE_OUTER_BOUND('',#4863,.T.);
#3834=FACE_OUTER_BOUND('',#4864,.T.);
#3835=FACE_OUTER_BOUND('',#4865,.T.);
#3836=FACE_OUTER_BOUND('',#4866,.T.);
#3837=FACE_OUTER_BOUND('',#4867,.T.);
#3838=FACE_OUTER_BOUND('',#4868,.T.);
#3839=FACE_OUTER_BOUND('',#4869,.T.);
#3840=FACE_OUTER_BOUND('',#4870,.T.);
#3841=FACE_OUTER_BOUND('',#4871,.T.);
#3842=FACE_OUTER_BOUND('',#4872,.T.);
#3843=FACE_OUTER_BOUND('',#4873,.T.);
#3844=FACE_OUTER_BOUND('',#4874,.T.);
#3845=FACE_OUTER_BOUND('',#4875,.T.);
#3846=FACE_OUTER_BOUND('',#4876,.T.);
#3847=FACE_OUTER_BOUND('',#4877,.T.);
#3848=FACE_OUTER_BOUND('',#4878,.T.);
#3849=FACE_OUTER_BOUND('',#4879,.T.);
#3850=FACE_OUTER_BOUND('',#4880,.T.);
#3851=FACE_OUTER_BOUND('',#4881,.T.);
#3852=FACE_OUTER_BOUND('',#4882,.T.);
#3853=FACE_OUTER_BOUND('',#4883,.T.);
#3854=FACE_OUTER_BOUND('',#4884,.T.);
#3855=FACE_OUTER_BOUND('',#4885,.T.);
#3856=FACE_OUTER_BOUND('',#4886,.T.);
#3857=FACE_OUTER_BOUND('',#4887,.T.);
#3858=FACE_OUTER_BOUND('',#4888,.T.);
#3859=FACE_OUTER_BOUND('',#4889,.T.);
#3860=FACE_OUTER_BOUND('',#4890,.T.);
#3861=FACE_OUTER_BOUND('',#4891,.T.);
#3862=FACE_OUTER_BOUND('',#4892,.T.);
#3863=FACE_OUTER_BOUND('',#4893,.T.);
#3864=FACE_OUTER_BOUND('',#4894,.T.);
#3865=FACE_OUTER_BOUND('',#4895,.T.);
#3866=FACE_OUTER_BOUND('',#4896,.T.);
#3867=FACE_OUTER_BOUND('',#4897,.T.);
#3868=FACE_OUTER_BOUND('',#4898,.T.);
#3869=FACE_OUTER_BOUND('',#4899,.T.);
#3870=FACE_OUTER_BOUND('',#4900,.T.);
#3871=FACE_OUTER_BOUND('',#4901,.T.);
#3872=FACE_OUTER_BOUND('',#4902,.T.);
#3873=FACE_OUTER_BOUND('',#4903,.T.);
#3874=FACE_OUTER_BOUND('',#4904,.T.);
#3875=FACE_OUTER_BOUND('',#4905,.T.);
#3876=FACE_OUTER_BOUND('',#4906,.T.);
#3877=FACE_OUTER_BOUND('',#4907,.T.);
#3878=FACE_OUTER_BOUND('',#4908,.T.);
#3879=FACE_OUTER_BOUND('',#4909,.T.);
#3880=FACE_OUTER_BOUND('',#4910,.T.);
#3881=FACE_OUTER_BOUND('',#4911,.T.);
#3882=FACE_OUTER_BOUND('',#4912,.T.);
#3883=FACE_OUTER_BOUND('',#4913,.T.);
#3884=FACE_OUTER_BOUND('',#4914,.T.);
#3885=FACE_OUTER_BOUND('',#4915,.T.);
#3886=FACE_OUTER_BOUND('',#4916,.T.);
#3887=FACE_OUTER_BOUND('',#4917,.T.);
#3888=FACE_OUTER_BOUND('',#4918,.T.);
#3889=FACE_OUTER_BOUND('',#4919,.T.);
#3890=FACE_OUTER_BOUND('',#4920,.T.);
#3891=FACE_OUTER_BOUND('',#4921,.T.);
#3892=FACE_OUTER_BOUND('',#4922,.T.);
#3893=FACE_OUTER_BOUND('',#4923,.T.);
#3894=FACE_OUTER_BOUND('',#4924,.T.);
#3895=FACE_OUTER_BOUND('',#4925,.T.);
#3896=FACE_OUTER_BOUND('',#4926,.T.);
#3897=FACE_OUTER_BOUND('',#4927,.T.);
#3898=FACE_OUTER_BOUND('',#4928,.T.);
#3899=FACE_OUTER_BOUND('',#4929,.T.);
#3900=FACE_OUTER_BOUND('',#4930,.T.);
#3901=FACE_OUTER_BOUND('',#4931,.T.);
#3902=FACE_OUTER_BOUND('',#4932,.T.);
#3903=FACE_OUTER_BOUND('',#4933,.T.);
#3904=FACE_OUTER_BOUND('',#4934,.T.);
#3905=FACE_OUTER_BOUND('',#4935,.T.);
#3906=FACE_OUTER_BOUND('',#4936,.T.);
#3907=FACE_OUTER_BOUND('',#4937,.T.);
#3908=FACE_OUTER_BOUND('',#4938,.T.);
#3909=FACE_OUTER_BOUND('',#4939,.T.);
#3910=FACE_OUTER_BOUND('',#4940,.T.);
#3911=FACE_OUTER_BOUND('',#4941,.T.);
#3912=FACE_OUTER_BOUND('',#4942,.T.);
#3913=FACE_OUTER_BOUND('',#4943,.T.);
#3914=FACE_OUTER_BOUND('',#4944,.T.);
#3915=FACE_OUTER_BOUND('',#4945,.T.);
#3916=FACE_OUTER_BOUND('',#4946,.T.);
#3917=FACE_OUTER_BOUND('',#4947,.T.);
#3918=FACE_OUTER_BOUND('',#4948,.T.);
#3919=FACE_OUTER_BOUND('',#4949,.T.);
#3920=FACE_OUTER_BOUND('',#4950,.T.);
#3921=FACE_OUTER_BOUND('',#4951,.T.);
#3922=FACE_OUTER_BOUND('',#4952,.T.);
#3923=FACE_OUTER_BOUND('',#4953,.T.);
#3924=FACE_OUTER_BOUND('',#4954,.T.);
#3925=FACE_OUTER_BOUND('',#4955,.T.);
#3926=FACE_OUTER_BOUND('',#4956,.T.);
#3927=FACE_OUTER_BOUND('',#4957,.T.);
#3928=FACE_OUTER_BOUND('',#4958,.T.);
#3929=FACE_OUTER_BOUND('',#4959,.T.);
#3930=FACE_OUTER_BOUND('',#4960,.T.);
#3931=FACE_OUTER_BOUND('',#4961,.T.);
#3932=FACE_OUTER_BOUND('',#4962,.T.);
#3933=FACE_OUTER_BOUND('',#4963,.T.);
#3934=FACE_OUTER_BOUND('',#4964,.T.);
#3935=FACE_OUTER_BOUND('',#4965,.T.);
#3936=FACE_OUTER_BOUND('',#4966,.T.);
#3937=FACE_OUTER_BOUND('',#4967,.T.);
#3938=FACE_OUTER_BOUND('',#4968,.T.);
#3939=FACE_OUTER_BOUND('',#4969,.T.);
#3940=FACE_OUTER_BOUND('',#4970,.T.);
#3941=FACE_OUTER_BOUND('',#4971,.T.);
#3942=FACE_OUTER_BOUND('',#4972,.T.);
#3943=FACE_OUTER_BOUND('',#4973,.T.);
#3944=FACE_OUTER_BOUND('',#4974,.T.);
#3945=FACE_OUTER_BOUND('',#4975,.T.);
#3946=FACE_OUTER_BOUND('',#4976,.T.);
#3947=FACE_OUTER_BOUND('',#4977,.T.);
#3948=FACE_OUTER_BOUND('',#4978,.T.);
#3949=FACE_OUTER_BOUND('',#4979,.T.);
#3950=FACE_OUTER_BOUND('',#4980,.T.);
#3951=FACE_OUTER_BOUND('',#4981,.T.);
#3952=FACE_OUTER_BOUND('',#4982,.T.);
#3953=FACE_OUTER_BOUND('',#4983,.T.);
#3954=FACE_OUTER_BOUND('',#4984,.T.);
#3955=FACE_OUTER_BOUND('',#4985,.T.);
#3956=FACE_OUTER_BOUND('',#4986,.T.);
#3957=FACE_OUTER_BOUND('',#4987,.T.);
#3958=FACE_OUTER_BOUND('',#4988,.T.);
#3959=FACE_OUTER_BOUND('',#4989,.T.);
#3960=FACE_OUTER_BOUND('',#4990,.T.);
#3961=FACE_OUTER_BOUND('',#4991,.T.);
#3962=FACE_OUTER_BOUND('',#4992,.T.);
#3963=FACE_OUTER_BOUND('',#4993,.T.);
#3964=FACE_OUTER_BOUND('',#4994,.T.);
#3965=FACE_OUTER_BOUND('',#4995,.T.);
#3966=FACE_OUTER_BOUND('',#4996,.T.);
#3967=FACE_OUTER_BOUND('',#4997,.T.);
#3968=FACE_OUTER_BOUND('',#4998,.T.);
#3969=FACE_OUTER_BOUND('',#4999,.T.);
#3970=FACE_OUTER_BOUND('',#5000,.T.);
#3971=FACE_OUTER_BOUND('',#5001,.T.);
#3972=FACE_OUTER_BOUND('',#5002,.T.);
#3973=FACE_OUTER_BOUND('',#5003,.T.);
#3974=FACE_OUTER_BOUND('',#5004,.T.);
#3975=FACE_OUTER_BOUND('',#5005,.T.);
#3976=FACE_OUTER_BOUND('',#5006,.T.);
#3977=FACE_OUTER_BOUND('',#5007,.T.);
#3978=FACE_OUTER_BOUND('',#5008,.T.);
#3979=FACE_OUTER_BOUND('',#5009,.T.);
#3980=FACE_OUTER_BOUND('',#5010,.T.);
#3981=FACE_OUTER_BOUND('',#5011,.T.);
#3982=FACE_OUTER_BOUND('',#5012,.T.);
#3983=FACE_OUTER_BOUND('',#5013,.T.);
#3984=FACE_OUTER_BOUND('',#5014,.T.);
#3985=FACE_OUTER_BOUND('',#5015,.T.);
#3986=FACE_OUTER_BOUND('',#5016,.T.);
#3987=FACE_OUTER_BOUND('',#5017,.T.);
#3988=FACE_OUTER_BOUND('',#5018,.T.);
#3989=FACE_OUTER_BOUND('',#5019,.T.);
#3990=FACE_OUTER_BOUND('',#5020,.T.);
#3991=FACE_OUTER_BOUND('',#5021,.T.);
#3992=FACE_OUTER_BOUND('',#5022,.T.);
#3993=FACE_OUTER_BOUND('',#5023,.T.);
#3994=FACE_OUTER_BOUND('',#5024,.T.);
#3995=FACE_OUTER_BOUND('',#5025,.T.);
#3996=FACE_OUTER_BOUND('',#5026,.T.);
#3997=FACE_OUTER_BOUND('',#5027,.T.);
#3998=FACE_OUTER_BOUND('',#5028,.T.);
#3999=FACE_OUTER_BOUND('',#5029,.T.);
#4000=FACE_OUTER_BOUND('',#5030,.T.);
#4001=FACE_OUTER_BOUND('',#5031,.T.);
#4002=FACE_OUTER_BOUND('',#5032,.T.);
#4003=FACE_OUTER_BOUND('',#5033,.T.);
#4004=FACE_OUTER_BOUND('',#5034,.T.);
#4005=FACE_OUTER_BOUND('',#5035,.T.);
#4006=FACE_OUTER_BOUND('',#5036,.T.);
#4007=FACE_OUTER_BOUND('',#5037,.T.);
#4008=FACE_OUTER_BOUND('',#5038,.T.);
#4009=FACE_OUTER_BOUND('',#5039,.T.);
#4010=FACE_OUTER_BOUND('',#5040,.T.);
#4011=FACE_OUTER_BOUND('',#5041,.T.);
#4012=FACE_OUTER_BOUND('',#5042,.T.);
#4013=FACE_OUTER_BOUND('',#5043,.T.);
#4014=FACE_OUTER_BOUND('',#5044,.T.);
#4015=FACE_OUTER_BOUND('',#5045,.T.);
#4016=FACE_OUTER_BOUND('',#5046,.T.);
#4017=FACE_OUTER_BOUND('',#5047,.T.);
#4018=FACE_OUTER_BOUND('',#5048,.T.);
#4019=FACE_OUTER_BOUND('',#5049,.T.);
#4020=FACE_OUTER_BOUND('',#5050,.T.);
#4021=FACE_OUTER_BOUND('',#5051,.T.);
#4022=FACE_OUTER_BOUND('',#5052,.T.);
#4023=FACE_OUTER_BOUND('',#5053,.T.);
#4024=FACE_OUTER_BOUND('',#5054,.T.);
#4025=FACE_OUTER_BOUND('',#5055,.T.);
#4026=FACE_OUTER_BOUND('',#5056,.T.);
#4027=FACE_OUTER_BOUND('',#5057,.T.);
#4028=FACE_OUTER_BOUND('',#5058,.T.);
#4029=FACE_OUTER_BOUND('',#5059,.T.);
#4030=FACE_OUTER_BOUND('',#5060,.T.);
#4031=FACE_OUTER_BOUND('',#5061,.T.);
#4032=FACE_OUTER_BOUND('',#5062,.T.);
#4033=FACE_OUTER_BOUND('',#5063,.T.);
#4034=FACE_OUTER_BOUND('',#5064,.T.);
#4035=FACE_OUTER_BOUND('',#5065,.T.);
#4036=FACE_OUTER_BOUND('',#5066,.T.);
#4037=FACE_OUTER_BOUND('',#5067,.T.);
#4038=FACE_OUTER_BOUND('',#5068,.T.);
#4039=FACE_OUTER_BOUND('',#5069,.T.);
#4040=FACE_OUTER_BOUND('',#5070,.T.);
#4041=FACE_OUTER_BOUND('',#5071,.T.);
#4042=FACE_OUTER_BOUND('',#5072,.T.);
#4043=FACE_OUTER_BOUND('',#5073,.T.);
#4044=FACE_OUTER_BOUND('',#5074,.T.);
#4045=FACE_OUTER_BOUND('',#5075,.T.);
#4046=FACE_OUTER_BOUND('',#5076,.T.);
#4047=FACE_OUTER_BOUND('',#5077,.T.);
#4048=FACE_OUTER_BOUND('',#5078,.T.);
#4049=FACE_OUTER_BOUND('',#5079,.T.);
#4050=FACE_OUTER_BOUND('',#5080,.T.);
#4051=FACE_OUTER_BOUND('',#5081,.T.);
#4052=FACE_OUTER_BOUND('',#5082,.T.);
#4053=FACE_OUTER_BOUND('',#5083,.T.);
#4054=FACE_OUTER_BOUND('',#5084,.T.);
#4055=FACE_OUTER_BOUND('',#5085,.T.);
#4056=FACE_OUTER_BOUND('',#5086,.T.);
#4057=FACE_OUTER_BOUND('',#5087,.T.);
#4058=FACE_OUTER_BOUND('',#5088,.T.);
#4059=FACE_OUTER_BOUND('',#5089,.T.);
#4060=FACE_OUTER_BOUND('',#5090,.T.);
#4061=FACE_OUTER_BOUND('',#5091,.T.);
#4062=FACE_OUTER_BOUND('',#5092,.T.);
#4063=FACE_OUTER_BOUND('',#5093,.T.);
#4064=FACE_OUTER_BOUND('',#5094,.T.);
#4065=FACE_OUTER_BOUND('',#5095,.T.);
#4066=FACE_OUTER_BOUND('',#5096,.T.);
#4067=FACE_OUTER_BOUND('',#5097,.T.);
#4068=FACE_OUTER_BOUND('',#5098,.T.);
#4069=FACE_OUTER_BOUND('',#5099,.T.);
#4070=FACE_OUTER_BOUND('',#5100,.T.);
#4071=FACE_OUTER_BOUND('',#5101,.T.);
#4072=FACE_OUTER_BOUND('',#5102,.T.);
#4073=FACE_OUTER_BOUND('',#5103,.T.);
#4074=FACE_OUTER_BOUND('',#5104,.T.);
#4075=FACE_OUTER_BOUND('',#5105,.T.);
#4076=FACE_OUTER_BOUND('',#5106,.T.);
#4077=FACE_OUTER_BOUND('',#5107,.T.);
#4078=FACE_OUTER_BOUND('',#5108,.T.);
#4079=FACE_OUTER_BOUND('',#5109,.T.);
#4080=FACE_OUTER_BOUND('',#5110,.T.);
#4081=FACE_OUTER_BOUND('',#5111,.T.);
#4082=FACE_OUTER_BOUND('',#5112,.T.);
#4083=FACE_OUTER_BOUND('',#5113,.T.);
#4084=FACE_OUTER_BOUND('',#5114,.T.);
#4085=FACE_OUTER_BOUND('',#5115,.T.);
#4086=FACE_OUTER_BOUND('',#5116,.T.);
#4087=FACE_OUTER_BOUND('',#5117,.T.);
#4088=FACE_OUTER_BOUND('',#5118,.T.);
#4089=FACE_OUTER_BOUND('',#5119,.T.);
#4090=FACE_OUTER_BOUND('',#5120,.T.);
#4091=FACE_OUTER_BOUND('',#5121,.T.);
#4092=FACE_OUTER_BOUND('',#5122,.T.);
#4093=FACE_OUTER_BOUND('',#5123,.T.);
#4094=FACE_OUTER_BOUND('',#5124,.T.);
#4095=FACE_OUTER_BOUND('',#5125,.T.);
#4096=FACE_OUTER_BOUND('',#5126,.T.);
#4097=FACE_OUTER_BOUND('',#5127,.T.);
#4098=FACE_OUTER_BOUND('',#5128,.T.);
#4099=FACE_OUTER_BOUND('',#5129,.T.);
#4100=FACE_OUTER_BOUND('',#5130,.T.);
#4101=FACE_OUTER_BOUND('',#5131,.T.);
#4102=FACE_OUTER_BOUND('',#5132,.T.);
#4103=FACE_OUTER_BOUND('',#5133,.T.);
#4104=FACE_OUTER_BOUND('',#5134,.T.);
#4105=FACE_OUTER_BOUND('',#5135,.T.);
#4106=FACE_OUTER_BOUND('',#5136,.T.);
#4107=FACE_OUTER_BOUND('',#5137,.T.);
#4108=FACE_OUTER_BOUND('',#5138,.T.);
#4109=FACE_OUTER_BOUND('',#5139,.T.);
#4110=FACE_OUTER_BOUND('',#5140,.T.);
#4111=FACE_OUTER_BOUND('',#5141,.T.);
#4112=FACE_OUTER_BOUND('',#5142,.T.);
#4113=FACE_OUTER_BOUND('',#5143,.T.);
#4114=FACE_OUTER_BOUND('',#5144,.T.);
#4115=FACE_OUTER_BOUND('',#5145,.T.);
#4116=FACE_OUTER_BOUND('',#5146,.T.);
#4117=FACE_OUTER_BOUND('',#5147,.T.);
#4118=FACE_OUTER_BOUND('',#5148,.T.);
#4119=FACE_OUTER_BOUND('',#5149,.T.);
#4120=FACE_OUTER_BOUND('',#5150,.T.);
#4121=FACE_OUTER_BOUND('',#5151,.T.);
#4122=FACE_OUTER_BOUND('',#5152,.T.);
#4123=FACE_OUTER_BOUND('',#5153,.T.);
#4124=FACE_OUTER_BOUND('',#5154,.T.);
#4125=FACE_OUTER_BOUND('',#5155,.T.);
#4126=FACE_OUTER_BOUND('',#5156,.T.);
#4127=FACE_OUTER_BOUND('',#5157,.T.);
#4128=FACE_OUTER_BOUND('',#5158,.T.);
#4129=FACE_OUTER_BOUND('',#5159,.T.);
#4130=FACE_OUTER_BOUND('',#5160,.T.);
#4131=FACE_OUTER_BOUND('',#5161,.T.);
#4132=FACE_OUTER_BOUND('',#5162,.T.);
#4133=FACE_OUTER_BOUND('',#5163,.T.);
#4134=FACE_OUTER_BOUND('',#5164,.T.);
#4135=FACE_OUTER_BOUND('',#5165,.T.);
#4136=FACE_OUTER_BOUND('',#5166,.T.);
#4137=FACE_OUTER_BOUND('',#5167,.T.);
#4138=FACE_OUTER_BOUND('',#5168,.T.);
#4139=FACE_OUTER_BOUND('',#5169,.T.);
#4140=FACE_OUTER_BOUND('',#5170,.T.);
#4141=FACE_OUTER_BOUND('',#5172,.T.);
#4142=FACE_OUTER_BOUND('',#5173,.T.);
#4143=FACE_OUTER_BOUND('',#5174,.T.);
#4144=FACE_OUTER_BOUND('',#5176,.T.);
#4145=FACE_OUTER_BOUND('',#5177,.T.);
#4146=FACE_OUTER_BOUND('',#5179,.T.);
#4147=FACE_OUTER_BOUND('',#5180,.T.);
#4148=FACE_OUTER_BOUND('',#5181,.T.);
#4149=FACE_OUTER_BOUND('',#5182,.T.);
#4150=FACE_OUTER_BOUND('',#5183,.T.);
#4151=FACE_OUTER_BOUND('',#5184,.T.);
#4152=FACE_OUTER_BOUND('',#5185,.T.);
#4153=FACE_OUTER_BOUND('',#5186,.T.);
#4154=FACE_OUTER_BOUND('',#5188,.T.);
#4155=FACE_OUTER_BOUND('',#5189,.T.);
#4156=FACE_OUTER_BOUND('',#5190,.T.);
#4157=FACE_OUTER_BOUND('',#5191,.T.);
#4158=FACE_OUTER_BOUND('',#5192,.T.);
#4159=FACE_OUTER_BOUND('',#5193,.T.);
#4160=FACE_OUTER_BOUND('',#5195,.T.);
#4161=FACE_OUTER_BOUND('',#5196,.T.);
#4162=FACE_OUTER_BOUND('',#5197,.T.);
#4163=FACE_OUTER_BOUND('',#5198,.T.);
#4164=FACE_OUTER_BOUND('',#5199,.T.);
#4165=FACE_OUTER_BOUND('',#5200,.T.);
#4166=FACE_OUTER_BOUND('',#5201,.T.);
#4167=FACE_OUTER_BOUND('',#5202,.T.);
#4168=FACE_OUTER_BOUND('',#5203,.T.);
#4169=FACE_OUTER_BOUND('',#5204,.T.);
#4170=FACE_OUTER_BOUND('',#5206,.T.);
#4171=FACE_OUTER_BOUND('',#5208,.T.);
#4172=FACE_OUTER_BOUND('',#5209,.T.);
#4173=FACE_OUTER_BOUND('',#5210,.T.);
#4174=FACE_OUTER_BOUND('',#5211,.T.);
#4175=FACE_OUTER_BOUND('',#5212,.T.);
#4176=FACE_OUTER_BOUND('',#5213,.T.);
#4177=FACE_OUTER_BOUND('',#5214,.T.);
#4178=FACE_OUTER_BOUND('',#5215,.T.);
#4179=FACE_OUTER_BOUND('',#5216,.T.);
#4180=FACE_OUTER_BOUND('',#5217,.T.);
#4181=FACE_OUTER_BOUND('',#5218,.T.);
#4182=FACE_OUTER_BOUND('',#5219,.T.);
#4183=FACE_OUTER_BOUND('',#5220,.T.);
#4184=FACE_OUTER_BOUND('',#5221,.T.);
#4185=FACE_OUTER_BOUND('',#5222,.T.);
#4186=FACE_OUTER_BOUND('',#5223,.T.);
#4187=FACE_OUTER_BOUND('',#5224,.T.);
#4188=FACE_OUTER_BOUND('',#5225,.T.);
#4189=FACE_OUTER_BOUND('',#5226,.T.);
#4190=FACE_OUTER_BOUND('',#5227,.T.);
#4191=FACE_OUTER_BOUND('',#5228,.T.);
#4192=FACE_OUTER_BOUND('',#5229,.T.);
#4193=FACE_OUTER_BOUND('',#5230,.T.);
#4194=FACE_OUTER_BOUND('',#5231,.T.);
#4195=FACE_OUTER_BOUND('',#5232,.T.);
#4196=FACE_OUTER_BOUND('',#5233,.T.);
#4197=FACE_OUTER_BOUND('',#5234,.T.);
#4198=FACE_OUTER_BOUND('',#5235,.T.);
#4199=FACE_OUTER_BOUND('',#5236,.T.);
#4200=FACE_OUTER_BOUND('',#5237,.T.);
#4201=FACE_OUTER_BOUND('',#5238,.T.);
#4202=FACE_OUTER_BOUND('',#5239,.T.);
#4203=FACE_OUTER_BOUND('',#5240,.T.);
#4204=FACE_OUTER_BOUND('',#5241,.T.);
#4205=FACE_OUTER_BOUND('',#5242,.T.);
#4206=FACE_OUTER_BOUND('',#5243,.T.);
#4207=FACE_OUTER_BOUND('',#5244,.T.);
#4208=FACE_OUTER_BOUND('',#5245,.T.);
#4209=FACE_OUTER_BOUND('',#5246,.T.);
#4210=FACE_OUTER_BOUND('',#5247,.T.);
#4211=FACE_OUTER_BOUND('',#5248,.T.);
#4212=FACE_OUTER_BOUND('',#5249,.T.);
#4213=FACE_OUTER_BOUND('',#5250,.T.);
#4214=FACE_OUTER_BOUND('',#5251,.T.);
#4215=FACE_OUTER_BOUND('',#5252,.T.);
#4216=FACE_OUTER_BOUND('',#5253,.T.);
#4217=FACE_OUTER_BOUND('',#5254,.T.);
#4218=FACE_OUTER_BOUND('',#5255,.T.);
#4219=FACE_OUTER_BOUND('',#5256,.T.);
#4220=FACE_OUTER_BOUND('',#5257,.T.);
#4221=FACE_OUTER_BOUND('',#5258,.T.);
#4222=FACE_OUTER_BOUND('',#5259,.T.);
#4223=FACE_OUTER_BOUND('',#5260,.T.);
#4224=FACE_OUTER_BOUND('',#5261,.T.);
#4225=FACE_OUTER_BOUND('',#5262,.T.);
#4226=FACE_OUTER_BOUND('',#5263,.T.);
#4227=FACE_OUTER_BOUND('',#5264,.T.);
#4228=FACE_OUTER_BOUND('',#5265,.T.);
#4229=FACE_OUTER_BOUND('',#5266,.T.);
#4230=FACE_OUTER_BOUND('',#5267,.T.);
#4231=FACE_OUTER_BOUND('',#5268,.T.);
#4232=FACE_OUTER_BOUND('',#5269,.T.);
#4233=FACE_OUTER_BOUND('',#5270,.T.);
#4234=FACE_OUTER_BOUND('',#5271,.T.);
#4235=FACE_OUTER_BOUND('',#5272,.T.);
#4236=FACE_OUTER_BOUND('',#5273,.T.);
#4237=FACE_OUTER_BOUND('',#5274,.T.);
#4238=FACE_OUTER_BOUND('',#5275,.T.);
#4239=FACE_OUTER_BOUND('',#5276,.T.);
#4240=FACE_OUTER_BOUND('',#5277,.T.);
#4241=FACE_OUTER_BOUND('',#5279,.T.);
#4242=FACE_OUTER_BOUND('',#5281,.T.);
#4243=FACE_OUTER_BOUND('',#5282,.T.);
#4244=FACE_OUTER_BOUND('',#5283,.T.);
#4245=FACE_OUTER_BOUND('',#5284,.T.);
#4246=FACE_OUTER_BOUND('',#5285,.T.);
#4247=FACE_OUTER_BOUND('',#5286,.T.);
#4248=FACE_OUTER_BOUND('',#5287,.T.);
#4249=FACE_OUTER_BOUND('',#5288,.T.);
#4250=FACE_OUTER_BOUND('',#5289,.T.);
#4251=FACE_OUTER_BOUND('',#5290,.T.);
#4252=FACE_OUTER_BOUND('',#5291,.T.);
#4253=FACE_OUTER_BOUND('',#5292,.T.);
#4254=FACE_OUTER_BOUND('',#5293,.T.);
#4255=FACE_OUTER_BOUND('',#5294,.T.);
#4256=FACE_OUTER_BOUND('',#5295,.T.);
#4257=FACE_OUTER_BOUND('',#5296,.T.);
#4258=FACE_OUTER_BOUND('',#5297,.T.);
#4259=FACE_OUTER_BOUND('',#5298,.T.);
#4260=FACE_OUTER_BOUND('',#5299,.T.);
#4261=FACE_OUTER_BOUND('',#5300,.T.);
#4262=FACE_OUTER_BOUND('',#5301,.T.);
#4263=FACE_OUTER_BOUND('',#5302,.T.);
#4264=FACE_OUTER_BOUND('',#5303,.T.);
#4265=FACE_OUTER_BOUND('',#5304,.T.);
#4266=FACE_OUTER_BOUND('',#5305,.T.);
#4267=FACE_OUTER_BOUND('',#5306,.T.);
#4268=FACE_OUTER_BOUND('',#5307,.T.);
#4269=FACE_OUTER_BOUND('',#5308,.T.);
#4270=FACE_OUTER_BOUND('',#5309,.T.);
#4271=FACE_OUTER_BOUND('',#5310,.T.);
#4272=FACE_OUTER_BOUND('',#5311,.T.);
#4273=FACE_OUTER_BOUND('',#5312,.T.);
#4274=FACE_OUTER_BOUND('',#5313,.T.);
#4275=FACE_OUTER_BOUND('',#5314,.T.);
#4276=FACE_OUTER_BOUND('',#5315,.T.);
#4277=FACE_OUTER_BOUND('',#5316,.T.);
#4278=FACE_OUTER_BOUND('',#5317,.T.);
#4279=FACE_OUTER_BOUND('',#5318,.T.);
#4280=FACE_OUTER_BOUND('',#5319,.T.);
#4281=FACE_OUTER_BOUND('',#5320,.T.);
#4282=FACE_OUTER_BOUND('',#5321,.T.);
#4283=FACE_OUTER_BOUND('',#5322,.T.);
#4284=FACE_OUTER_BOUND('',#5323,.T.);
#4285=FACE_OUTER_BOUND('',#5324,.T.);
#4286=FACE_OUTER_BOUND('',#5325,.T.);
#4287=FACE_OUTER_BOUND('',#5326,.T.);
#4288=FACE_OUTER_BOUND('',#5327,.T.);
#4289=FACE_OUTER_BOUND('',#5328,.T.);
#4290=FACE_OUTER_BOUND('',#5329,.T.);
#4291=FACE_OUTER_BOUND('',#5330,.T.);
#4292=FACE_OUTER_BOUND('',#5331,.T.);
#4293=FACE_OUTER_BOUND('',#5332,.T.);
#4294=FACE_OUTER_BOUND('',#5334,.T.);
#4295=FACE_OUTER_BOUND('',#5335,.T.);
#4296=FACE_OUTER_BOUND('',#5337,.T.);
#4297=FACE_OUTER_BOUND('',#5338,.T.);
#4298=FACE_OUTER_BOUND('',#5340,.T.);
#4299=FACE_OUTER_BOUND('',#5341,.T.);
#4300=FACE_OUTER_BOUND('',#5342,.T.);
#4301=FACE_OUTER_BOUND('',#5343,.T.);
#4302=FACE_OUTER_BOUND('',#5344,.T.);
#4303=FACE_OUTER_BOUND('',#5346,.T.);
#4304=FACE_OUTER_BOUND('',#5347,.T.);
#4305=FACE_OUTER_BOUND('',#5348,.T.);
#4306=FACE_OUTER_BOUND('',#5349,.T.);
#4307=FACE_OUTER_BOUND('',#5350,.T.);
#4308=FACE_OUTER_BOUND('',#5351,.T.);
#4309=FACE_OUTER_BOUND('',#5352,.T.);
#4310=FACE_OUTER_BOUND('',#5353,.T.);
#4311=FACE_OUTER_BOUND('',#5354,.T.);
#4312=FACE_OUTER_BOUND('',#5355,.T.);
#4313=FACE_OUTER_BOUND('',#5356,.T.);
#4314=FACE_OUTER_BOUND('',#5357,.T.);
#4315=FACE_OUTER_BOUND('',#5358,.T.);
#4316=FACE_OUTER_BOUND('',#5359,.T.);
#4317=FACE_OUTER_BOUND('',#5360,.T.);
#4318=FACE_OUTER_BOUND('',#5361,.T.);
#4319=FACE_OUTER_BOUND('',#5362,.T.);
#4320=FACE_OUTER_BOUND('',#5363,.T.);
#4321=FACE_OUTER_BOUND('',#5364,.T.);
#4322=FACE_OUTER_BOUND('',#5365,.T.);
#4323=FACE_OUTER_BOUND('',#5366,.T.);
#4324=FACE_OUTER_BOUND('',#5367,.T.);
#4325=FACE_OUTER_BOUND('',#5368,.T.);
#4326=FACE_OUTER_BOUND('',#5369,.T.);
#4327=FACE_OUTER_BOUND('',#5370,.T.);
#4328=FACE_OUTER_BOUND('',#5371,.T.);
#4329=FACE_OUTER_BOUND('',#5372,.T.);
#4330=FACE_OUTER_BOUND('',#5373,.T.);
#4331=FACE_OUTER_BOUND('',#5374,.T.);
#4332=FACE_OUTER_BOUND('',#5379,.T.);
#4333=FACE_OUTER_BOUND('',#5384,.T.);
#4334=FACE_OUTER_BOUND('',#5385,.T.);
#4335=FACE_OUTER_BOUND('',#5386,.T.);
#4336=FACE_OUTER_BOUND('',#5387,.T.);
#4337=FACE_OUTER_BOUND('',#5388,.T.);
#4338=FACE_OUTER_BOUND('',#5389,.T.);
#4339=FACE_OUTER_BOUND('',#5390,.T.);
#4340=FACE_OUTER_BOUND('',#5391,.T.);
#4341=FACE_OUTER_BOUND('',#5392,.T.);
#4342=FACE_OUTER_BOUND('',#5393,.T.);
#4343=FACE_OUTER_BOUND('',#5394,.T.);
#4344=FACE_OUTER_BOUND('',#5395,.T.);
#4345=FACE_OUTER_BOUND('',#5396,.T.);
#4346=FACE_OUTER_BOUND('',#5397,.T.);
#4347=FACE_OUTER_BOUND('',#5398,.T.);
#4348=FACE_OUTER_BOUND('',#5399,.T.);
#4349=FACE_OUTER_BOUND('',#5400,.T.);
#4350=FACE_OUTER_BOUND('',#5401,.T.);
#4351=FACE_OUTER_BOUND('',#5402,.T.);
#4352=FACE_OUTER_BOUND('',#5403,.T.);
#4353=FACE_OUTER_BOUND('',#5404,.T.);
#4354=FACE_OUTER_BOUND('',#5405,.T.);
#4355=FACE_OUTER_BOUND('',#5406,.T.);
#4356=FACE_OUTER_BOUND('',#5407,.T.);
#4357=FACE_OUTER_BOUND('',#5408,.T.);
#4358=FACE_OUTER_BOUND('',#5410,.T.);
#4359=FACE_OUTER_BOUND('',#5412,.T.);
#4360=FACE_OUTER_BOUND('',#5413,.T.);
#4361=FACE_OUTER_BOUND('',#5414,.T.);
#4362=FACE_OUTER_BOUND('',#5415,.T.);
#4363=FACE_OUTER_BOUND('',#5416,.T.);
#4364=FACE_OUTER_BOUND('',#5417,.T.);
#4365=FACE_OUTER_BOUND('',#5418,.T.);
#4366=FACE_OUTER_BOUND('',#5419,.T.);
#4367=FACE_OUTER_BOUND('',#5420,.T.);
#4368=FACE_OUTER_BOUND('',#5421,.T.);
#4369=FACE_OUTER_BOUND('',#5422,.T.);
#4370=FACE_OUTER_BOUND('',#5423,.T.);
#4371=FACE_OUTER_BOUND('',#5424,.T.);
#4372=FACE_OUTER_BOUND('',#5425,.T.);
#4373=FACE_OUTER_BOUND('',#5426,.T.);
#4374=FACE_OUTER_BOUND('',#5427,.T.);
#4375=FACE_OUTER_BOUND('',#5428,.T.);
#4376=FACE_OUTER_BOUND('',#5429,.T.);
#4377=FACE_OUTER_BOUND('',#5430,.T.);
#4378=FACE_OUTER_BOUND('',#5431,.T.);
#4379=FACE_OUTER_BOUND('',#5432,.T.);
#4380=FACE_OUTER_BOUND('',#5433,.T.);
#4381=FACE_OUTER_BOUND('',#5434,.T.);
#4382=FACE_OUTER_BOUND('',#5435,.T.);
#4383=FACE_OUTER_BOUND('',#5436,.T.);
#4384=FACE_OUTER_BOUND('',#5437,.T.);
#4385=FACE_OUTER_BOUND('',#5438,.T.);
#4386=FACE_OUTER_BOUND('',#5439,.T.);
#4387=FACE_OUTER_BOUND('',#5440,.T.);
#4388=FACE_OUTER_BOUND('',#5441,.T.);
#4389=FACE_OUTER_BOUND('',#5442,.T.);
#4390=FACE_OUTER_BOUND('',#5443,.T.);
#4391=FACE_OUTER_BOUND('',#5444,.T.);
#4392=FACE_OUTER_BOUND('',#5445,.T.);
#4393=FACE_OUTER_BOUND('',#5446,.T.);
#4394=FACE_OUTER_BOUND('',#5447,.T.);
#4395=FACE_OUTER_BOUND('',#5448,.T.);
#4396=FACE_OUTER_BOUND('',#5449,.T.);
#4397=FACE_OUTER_BOUND('',#5450,.T.);
#4398=FACE_OUTER_BOUND('',#5451,.T.);
#4399=FACE_OUTER_BOUND('',#5452,.T.);
#4400=FACE_OUTER_BOUND('',#5458,.T.);
#4401=FACE_OUTER_BOUND('',#5459,.T.);
#4402=FACE_OUTER_BOUND('',#5460,.T.);
#4403=FACE_OUTER_BOUND('',#5466,.T.);
#4404=FACE_OUTER_BOUND('',#5467,.T.);
#4405=FACE_OUTER_BOUND('',#5468,.T.);
#4406=FACE_OUTER_BOUND('',#5469,.T.);
#4407=FACE_OUTER_BOUND('',#5470,.T.);
#4408=FACE_OUTER_BOUND('',#5471,.T.);
#4409=FACE_OUTER_BOUND('',#5475,.T.);
#4410=FACE_OUTER_BOUND('',#5477,.T.);
#4411=FACE_OUTER_BOUND('',#5478,.T.);
#4412=FACE_OUTER_BOUND('',#5479,.T.);
#4413=FACE_OUTER_BOUND('',#5481,.T.);
#4414=FACE_OUTER_BOUND('',#5483,.T.);
#4415=FACE_OUTER_BOUND('',#5484,.T.);
#4416=FACE_OUTER_BOUND('',#5485,.T.);
#4417=FACE_OUTER_BOUND('',#5486,.T.);
#4418=FACE_OUTER_BOUND('',#5487,.T.);
#4419=FACE_OUTER_BOUND('',#5488,.T.);
#4420=FACE_OUTER_BOUND('',#5489,.T.);
#4421=FACE_OUTER_BOUND('',#5490,.T.);
#4422=FACE_OUTER_BOUND('',#5491,.T.);
#4423=FACE_OUTER_BOUND('',#5492,.T.);
#4424=FACE_OUTER_BOUND('',#5493,.T.);
#4425=FACE_OUTER_BOUND('',#5494,.T.);
#4426=FACE_OUTER_BOUND('',#5495,.T.);
#4427=FACE_OUTER_BOUND('',#5496,.T.);
#4428=FACE_OUTER_BOUND('',#5497,.T.);
#4429=FACE_OUTER_BOUND('',#5498,.T.);
#4430=FACE_OUTER_BOUND('',#5499,.T.);
#4431=FACE_OUTER_BOUND('',#5500,.T.);
#4432=FACE_OUTER_BOUND('',#5504,.T.);
#4433=FACE_OUTER_BOUND('',#5505,.T.);
#4434=FACE_OUTER_BOUND('',#5506,.T.);
#4435=FACE_OUTER_BOUND('',#5507,.T.);
#4436=FACE_OUTER_BOUND('',#5508,.T.);
#4437=FACE_OUTER_BOUND('',#5509,.T.);
#4438=FACE_OUTER_BOUND('',#5510,.T.);
#4439=FACE_OUTER_BOUND('',#5511,.T.);
#4440=FACE_OUTER_BOUND('',#5512,.T.);
#4441=FACE_OUTER_BOUND('',#5513,.T.);
#4442=FACE_OUTER_BOUND('',#5514,.T.);
#4443=FACE_OUTER_BOUND('',#5515,.T.);
#4444=FACE_OUTER_BOUND('',#5516,.T.);
#4445=FACE_OUTER_BOUND('',#5517,.T.);
#4446=FACE_OUTER_BOUND('',#5518,.T.);
#4447=FACE_OUTER_BOUND('',#5519,.T.);
#4448=FACE_OUTER_BOUND('',#5520,.T.);
#4449=FACE_OUTER_BOUND('',#5521,.T.);
#4450=FACE_OUTER_BOUND('',#5522,.T.);
#4451=FACE_OUTER_BOUND('',#5523,.T.);
#4452=FACE_OUTER_BOUND('',#5524,.T.);
#4453=FACE_OUTER_BOUND('',#5525,.T.);
#4454=FACE_OUTER_BOUND('',#5526,.T.);
#4455=FACE_OUTER_BOUND('',#5527,.T.);
#4456=FACE_OUTER_BOUND('',#5528,.T.);
#4457=FACE_OUTER_BOUND('',#5529,.T.);
#4458=FACE_OUTER_BOUND('',#5530,.T.);
#4459=FACE_OUTER_BOUND('',#5531,.T.);
#4460=FACE_OUTER_BOUND('',#5532,.T.);
#4461=FACE_OUTER_BOUND('',#5533,.T.);
#4462=FACE_OUTER_BOUND('',#5534,.T.);
#4463=FACE_OUTER_BOUND('',#5535,.T.);
#4464=FACE_OUTER_BOUND('',#5536,.T.);
#4465=FACE_OUTER_BOUND('',#5537,.T.);
#4466=FACE_OUTER_BOUND('',#5538,.T.);
#4467=FACE_OUTER_BOUND('',#5539,.T.);
#4468=FACE_OUTER_BOUND('',#5540,.T.);
#4469=FACE_OUTER_BOUND('',#5541,.T.);
#4470=FACE_OUTER_BOUND('',#5542,.T.);
#4471=FACE_OUTER_BOUND('',#5543,.T.);
#4472=FACE_OUTER_BOUND('',#5544,.T.);
#4473=FACE_OUTER_BOUND('',#5545,.T.);
#4474=FACE_OUTER_BOUND('',#5546,.T.);
#4475=FACE_OUTER_BOUND('',#5547,.T.);
#4476=FACE_OUTER_BOUND('',#5548,.T.);
#4477=FACE_OUTER_BOUND('',#5549,.T.);
#4478=FACE_OUTER_BOUND('',#5550,.T.);
#4479=FACE_OUTER_BOUND('',#5551,.T.);
#4480=FACE_OUTER_BOUND('',#5552,.T.);
#4481=FACE_OUTER_BOUND('',#5553,.T.);
#4482=FACE_OUTER_BOUND('',#5554,.T.);
#4483=FACE_OUTER_BOUND('',#5555,.T.);
#4484=FACE_OUTER_BOUND('',#5556,.T.);
#4485=FACE_OUTER_BOUND('',#5557,.T.);
#4486=FACE_OUTER_BOUND('',#5558,.T.);
#4487=FACE_OUTER_BOUND('',#5559,.T.);
#4488=FACE_OUTER_BOUND('',#5560,.T.);
#4489=FACE_OUTER_BOUND('',#5561,.T.);
#4490=FACE_OUTER_BOUND('',#5562,.T.);
#4491=FACE_OUTER_BOUND('',#5563,.T.);
#4492=FACE_OUTER_BOUND('',#5564,.T.);
#4493=FACE_OUTER_BOUND('',#5565,.T.);
#4494=FACE_OUTER_BOUND('',#5566,.T.);
#4495=FACE_OUTER_BOUND('',#5567,.T.);
#4496=FACE_OUTER_BOUND('',#5568,.T.);
#4497=FACE_OUTER_BOUND('',#5569,.T.);
#4498=FACE_OUTER_BOUND('',#5570,.T.);
#4499=FACE_OUTER_BOUND('',#5571,.T.);
#4500=FACE_OUTER_BOUND('',#5572,.T.);
#4501=FACE_OUTER_BOUND('',#5573,.T.);
#4502=FACE_OUTER_BOUND('',#5574,.T.);
#4503=FACE_OUTER_BOUND('',#5575,.T.);
#4504=FACE_OUTER_BOUND('',#5576,.T.);
#4505=FACE_OUTER_BOUND('',#5577,.T.);
#4506=FACE_OUTER_BOUND('',#5578,.T.);
#4507=FACE_OUTER_BOUND('',#5579,.T.);
#4508=FACE_OUTER_BOUND('',#5580,.T.);
#4509=FACE_OUTER_BOUND('',#5581,.T.);
#4510=FACE_OUTER_BOUND('',#5582,.T.);
#4511=FACE_OUTER_BOUND('',#5583,.T.);
#4512=FACE_OUTER_BOUND('',#5584,.T.);
#4513=FACE_OUTER_BOUND('',#5585,.T.);
#4514=FACE_OUTER_BOUND('',#5586,.T.);
#4515=FACE_OUTER_BOUND('',#5587,.T.);
#4516=FACE_OUTER_BOUND('',#5588,.T.);
#4517=FACE_OUTER_BOUND('',#5589,.T.);
#4518=FACE_OUTER_BOUND('',#5590,.T.);
#4519=FACE_OUTER_BOUND('',#5591,.T.);
#4520=FACE_OUTER_BOUND('',#5592,.T.);
#4521=FACE_OUTER_BOUND('',#5593,.T.);
#4522=FACE_OUTER_BOUND('',#5594,.T.);
#4523=FACE_OUTER_BOUND('',#5595,.T.);
#4524=FACE_OUTER_BOUND('',#5596,.T.);
#4525=FACE_OUTER_BOUND('',#5597,.T.);
#4526=FACE_OUTER_BOUND('',#5598,.T.);
#4527=FACE_OUTER_BOUND('',#5599,.T.);
#4528=FACE_OUTER_BOUND('',#5600,.T.);
#4529=FACE_OUTER_BOUND('',#5601,.T.);
#4530=FACE_OUTER_BOUND('',#5602,.T.);
#4531=FACE_OUTER_BOUND('',#5603,.T.);
#4532=FACE_OUTER_BOUND('',#5604,.T.);
#4533=FACE_OUTER_BOUND('',#5605,.T.);
#4534=FACE_OUTER_BOUND('',#5606,.T.);
#4535=FACE_OUTER_BOUND('',#5607,.T.);
#4536=FACE_OUTER_BOUND('',#5608,.T.);
#4537=FACE_OUTER_BOUND('',#5609,.T.);
#4538=FACE_OUTER_BOUND('',#5610,.T.);
#4539=FACE_OUTER_BOUND('',#5611,.T.);
#4540=FACE_OUTER_BOUND('',#5612,.T.);
#4541=FACE_OUTER_BOUND('',#5613,.T.);
#4542=FACE_OUTER_BOUND('',#5614,.T.);
#4543=FACE_OUTER_BOUND('',#5615,.T.);
#4544=FACE_OUTER_BOUND('',#5616,.T.);
#4545=FACE_OUTER_BOUND('',#5617,.T.);
#4546=FACE_OUTER_BOUND('',#5618,.T.);
#4547=FACE_OUTER_BOUND('',#5619,.T.);
#4548=FACE_OUTER_BOUND('',#5620,.T.);
#4549=FACE_OUTER_BOUND('',#5621,.T.);
#4550=EDGE_LOOP('',(#11069,#11070,#11071,#11072,#11073,#11074,#11075,#11076,
#11077,#11078,#11079,#11080,#11081,#11082,#11083,#11084,#11085,#11086,#11087,
#11088,#11089,#11090,#11091,#11092,#11093,#11094,#11095,#11096,#11097,#11098,
#11099,#11100,#11101,#11102,#11103,#11104,#11105,#11106,#11107,#11108,#11109,
#11110,#11111,#11112,#11113,#11114,#11115,#11116,#11117,#11118,#11119,#11120,
#11121,#11122,#11123,#11124,#11125,#11126,#11127,#11128,#11129,#11130,#11131,
#11132,#11133,#11134,#11135,#11136,#11137,#11138,#11139,#11140,#11141,#11142,
#11143,#11144,#11145,#11146,#11147,#11148,#11149,#11150,#11151,#11152,#11153,
#11154,#11155,#11156,#11157,#11158,#11159,#11160,#11161,#11162,#11163,#11164,
#11165,#11166,#11167,#11168,#11169,#11170,#11171,#11172,#11173,#11174,#11175,
#11176,#11177,#11178,#11179,#11180,#11181,#11182,#11183,#11184,#11185,#11186,
#11187,#11188,#11189,#11190,#11191,#11192,#11193,#11194,#11195,#11196,#11197,
#11198,#11199,#11200,#11201,#11202,#11203,#11204,#11205,#11206,#11207,#11208,
#11209,#11210,#11211,#11212,#11213,#11214,#11215,#11216,#11217,#11218,#11219,
#11220,#11221,#11222,#11223,#11224,#11225,#11226,#11227,#11228,#11229,#11230,
#11231,#11232,#11233,#11234,#11235,#11236,#11237,#11238,#11239,#11240,#11241,
#11242,#11243,#11244,#11245,#11246,#11247,#11248,#11249,#11250,#11251,#11252));
#4551=EDGE_LOOP('',(#11253));
#4552=EDGE_LOOP('',(#11254,#11255,#11256,#11257));
#4553=EDGE_LOOP('',(#11258,#11259,#11260,#11261));
#4554=EDGE_LOOP('',(#11262,#11263,#11264,#11265));
#4555=EDGE_LOOP('',(#11266,#11267,#11268,#11269));
#4556=EDGE_LOOP('',(#11270,#11271,#11272,#11273));
#4557=EDGE_LOOP('',(#11274,#11275,#11276,#11277));
#4558=EDGE_LOOP('',(#11278,#11279,#11280,#11281));
#4559=EDGE_LOOP('',(#11282,#11283,#11284,#11285));
#4560=EDGE_LOOP('',(#11286,#11287,#11288,#11289));
#4561=EDGE_LOOP('',(#11290,#11291,#11292,#11293));
#4562=EDGE_LOOP('',(#11294,#11295,#11296,#11297));
#4563=EDGE_LOOP('',(#11298,#11299,#11300,#11301));
#4564=EDGE_LOOP('',(#11302,#11303,#11304,#11305));
#4565=EDGE_LOOP('',(#11306,#11307,#11308,#11309));
#4566=EDGE_LOOP('',(#11310,#11311,#11312,#11313));
#4567=EDGE_LOOP('',(#11314,#11315,#11316,#11317));
#4568=EDGE_LOOP('',(#11318,#11319,#11320,#11321));
#4569=EDGE_LOOP('',(#11322,#11323,#11324,#11325));
#4570=EDGE_LOOP('',(#11326,#11327,#11328,#11329));
#4571=EDGE_LOOP('',(#11330,#11331,#11332,#11333));
#4572=EDGE_LOOP('',(#11334,#11335,#11336,#11337));
#4573=EDGE_LOOP('',(#11338,#11339,#11340,#11341));
#4574=EDGE_LOOP('',(#11342,#11343,#11344,#11345));
#4575=EDGE_LOOP('',(#11346,#11347,#11348,#11349));
#4576=EDGE_LOOP('',(#11350,#11351,#11352,#11353));
#4577=EDGE_LOOP('',(#11354,#11355,#11356,#11357));
#4578=EDGE_LOOP('',(#11358,#11359,#11360,#11361));
#4579=EDGE_LOOP('',(#11362,#11363,#11364,#11365));
#4580=EDGE_LOOP('',(#11366,#11367,#11368,#11369));
#4581=EDGE_LOOP('',(#11370,#11371,#11372,#11373));
#4582=EDGE_LOOP('',(#11374,#11375,#11376,#11377));
#4583=EDGE_LOOP('',(#11378,#11379,#11380,#11381));
#4584=EDGE_LOOP('',(#11382,#11383,#11384,#11385));
#4585=EDGE_LOOP('',(#11386,#11387,#11388,#11389));
#4586=EDGE_LOOP('',(#11390,#11391,#11392,#11393));
#4587=EDGE_LOOP('',(#11394,#11395,#11396,#11397));
#4588=EDGE_LOOP('',(#11398,#11399,#11400,#11401));
#4589=EDGE_LOOP('',(#11402,#11403,#11404,#11405));
#4590=EDGE_LOOP('',(#11406,#11407,#11408,#11409));
#4591=EDGE_LOOP('',(#11410,#11411,#11412,#11413));
#4592=EDGE_LOOP('',(#11414,#11415,#11416,#11417));
#4593=EDGE_LOOP('',(#11418,#11419,#11420,#11421));
#4594=EDGE_LOOP('',(#11422,#11423,#11424,#11425));
#4595=EDGE_LOOP('',(#11426,#11427,#11428,#11429));
#4596=EDGE_LOOP('',(#11430,#11431,#11432,#11433));
#4597=EDGE_LOOP('',(#11434,#11435,#11436,#11437,#11438,#11439,#11440,#11441,
#11442,#11443,#11444,#11445,#11446,#11447,#11448,#11449,#11450,#11451,#11452,
#11453,#11454,#11455,#11456,#11457,#11458,#11459,#11460,#11461,#11462,#11463,
#11464,#11465,#11466,#11467,#11468,#11469,#11470,#11471,#11472,#11473,#11474,
#11475,#11476,#11477,#11478,#11479,#11480,#11481,#11482,#11483,#11484,#11485,
#11486,#11487,#11488,#11489,#11490,#11491,#11492,#11493,#11494,#11495,#11496,
#11497,#11498,#11499,#11500,#11501,#11502,#11503,#11504,#11505,#11506,#11507,
#11508,#11509,#11510,#11511,#11512,#11513,#11514,#11515,#11516,#11517,#11518,
#11519,#11520,#11521,#11522,#11523,#11524,#11525,#11526,#11527,#11528,#11529,
#11530,#11531,#11532,#11533,#11534,#11535,#11536,#11537,#11538,#11539,#11540,
#11541,#11542,#11543,#11544,#11545,#11546,#11547,#11548,#11549,#11550,#11551,
#11552,#11553,#11554,#11555,#11556,#11557,#11558,#11559,#11560,#11561,#11562,
#11563,#11564,#11565,#11566,#11567,#11568,#11569,#11570,#11571,#11572,#11573,
#11574,#11575,#11576,#11577,#11578,#11579,#11580,#11581,#11582,#11583,#11584,
#11585,#11586,#11587,#11588,#11589,#11590,#11591,#11592,#11593,#11594,#11595,
#11596,#11597,#11598,#11599,#11600,#11601,#11602,#11603,#11604,#11605,#11606,
#11607,#11608,#11609,#11610,#11611,#11612,#11613,#11614,#11615,#11616,#11617));
#4598=EDGE_LOOP('',(#11618));
#4599=EDGE_LOOP('',(#11619,#11620,#11621,#11622));
#4600=EDGE_LOOP('',(#11623,#11624,#11625,#11626));
#4601=EDGE_LOOP('',(#11627,#11628,#11629,#11630));
#4602=EDGE_LOOP('',(#11631,#11632,#11633,#11634));
#4603=EDGE_LOOP('',(#11635,#11636,#11637,#11638));
#4604=EDGE_LOOP('',(#11639,#11640,#11641,#11642));
#4605=EDGE_LOOP('',(#11643,#11644,#11645,#11646));
#4606=EDGE_LOOP('',(#11647,#11648,#11649,#11650));
#4607=EDGE_LOOP('',(#11651,#11652,#11653,#11654));
#4608=EDGE_LOOP('',(#11655,#11656,#11657,#11658));
#4609=EDGE_LOOP('',(#11659,#11660,#11661,#11662));
#4610=EDGE_LOOP('',(#11663,#11664,#11665,#11666));
#4611=EDGE_LOOP('',(#11667,#11668,#11669,#11670));
#4612=EDGE_LOOP('',(#11671,#11672,#11673,#11674));
#4613=EDGE_LOOP('',(#11675,#11676,#11677,#11678));
#4614=EDGE_LOOP('',(#11679,#11680,#11681,#11682));
#4615=EDGE_LOOP('',(#11683,#11684,#11685,#11686));
#4616=EDGE_LOOP('',(#11687,#11688,#11689,#11690));
#4617=EDGE_LOOP('',(#11691,#11692,#11693,#11694));
#4618=EDGE_LOOP('',(#11695,#11696,#11697,#11698));
#4619=EDGE_LOOP('',(#11699,#11700,#11701,#11702));
#4620=EDGE_LOOP('',(#11703,#11704,#11705,#11706));
#4621=EDGE_LOOP('',(#11707,#11708,#11709,#11710));
#4622=EDGE_LOOP('',(#11711,#11712,#11713,#11714));
#4623=EDGE_LOOP('',(#11715,#11716,#11717,#11718));
#4624=EDGE_LOOP('',(#11719,#11720,#11721,#11722));
#4625=EDGE_LOOP('',(#11723,#11724,#11725,#11726));
#4626=EDGE_LOOP('',(#11727,#11728,#11729,#11730));
#4627=EDGE_LOOP('',(#11731,#11732,#11733,#11734));
#4628=EDGE_LOOP('',(#11735,#11736,#11737,#11738));
#4629=EDGE_LOOP('',(#11739,#11740,#11741,#11742));
#4630=EDGE_LOOP('',(#11743,#11744,#11745,#11746));
#4631=EDGE_LOOP('',(#11747,#11748,#11749,#11750));
#4632=EDGE_LOOP('',(#11751,#11752,#11753,#11754));
#4633=EDGE_LOOP('',(#11755,#11756,#11757,#11758));
#4634=EDGE_LOOP('',(#11759,#11760,#11761,#11762));
#4635=EDGE_LOOP('',(#11763,#11764,#11765,#11766));
#4636=EDGE_LOOP('',(#11767,#11768,#11769,#11770));
#4637=EDGE_LOOP('',(#11771,#11772,#11773,#11774));
#4638=EDGE_LOOP('',(#11775,#11776,#11777,#11778));
#4639=EDGE_LOOP('',(#11779,#11780,#11781,#11782));
#4640=EDGE_LOOP('',(#11783,#11784,#11785,#11786));
#4641=EDGE_LOOP('',(#11787,#11788,#11789,#11790));
#4642=EDGE_LOOP('',(#11791,#11792,#11793,#11794));
#4643=EDGE_LOOP('',(#11795,#11796,#11797,#11798));
#4644=EDGE_LOOP('',(#11799,#11800,#11801,#11802));
#4645=EDGE_LOOP('',(#11803,#11804,#11805,#11806));
#4646=EDGE_LOOP('',(#11807,#11808,#11809,#11810));
#4647=EDGE_LOOP('',(#11811,#11812,#11813,#11814));
#4648=EDGE_LOOP('',(#11815,#11816,#11817,#11818));
#4649=EDGE_LOOP('',(#11819,#11820,#11821,#11822));
#4650=EDGE_LOOP('',(#11823,#11824,#11825,#11826));
#4651=EDGE_LOOP('',(#11827,#11828,#11829,#11830));
#4652=EDGE_LOOP('',(#11831,#11832,#11833,#11834));
#4653=EDGE_LOOP('',(#11835,#11836,#11837,#11838));
#4654=EDGE_LOOP('',(#11839,#11840,#11841,#11842));
#4655=EDGE_LOOP('',(#11843,#11844,#11845,#11846));
#4656=EDGE_LOOP('',(#11847,#11848,#11849,#11850));
#4657=EDGE_LOOP('',(#11851,#11852,#11853,#11854));
#4658=EDGE_LOOP('',(#11855,#11856,#11857,#11858));
#4659=EDGE_LOOP('',(#11859,#11860,#11861,#11862));
#4660=EDGE_LOOP('',(#11863,#11864,#11865,#11866));
#4661=EDGE_LOOP('',(#11867,#11868,#11869,#11870));
#4662=EDGE_LOOP('',(#11871,#11872,#11873,#11874));
#4663=EDGE_LOOP('',(#11875,#11876,#11877,#11878));
#4664=EDGE_LOOP('',(#11879,#11880,#11881,#11882));
#4665=EDGE_LOOP('',(#11883,#11884,#11885,#11886));
#4666=EDGE_LOOP('',(#11887,#11888,#11889,#11890));
#4667=EDGE_LOOP('',(#11891,#11892,#11893,#11894));
#4668=EDGE_LOOP('',(#11895,#11896,#11897,#11898));
#4669=EDGE_LOOP('',(#11899,#11900,#11901,#11902));
#4670=EDGE_LOOP('',(#11903,#11904,#11905,#11906));
#4671=EDGE_LOOP('',(#11907,#11908,#11909,#11910));
#4672=EDGE_LOOP('',(#11911,#11912,#11913,#11914));
#4673=EDGE_LOOP('',(#11915,#11916,#11917,#11918));
#4674=EDGE_LOOP('',(#11919,#11920,#11921,#11922));
#4675=EDGE_LOOP('',(#11923,#11924,#11925,#11926));
#4676=EDGE_LOOP('',(#11927,#11928,#11929,#11930));
#4677=EDGE_LOOP('',(#11931,#11932,#11933,#11934));
#4678=EDGE_LOOP('',(#11935,#11936,#11937,#11938));
#4679=EDGE_LOOP('',(#11939,#11940,#11941,#11942));
#4680=EDGE_LOOP('',(#11943,#11944,#11945,#11946));
#4681=EDGE_LOOP('',(#11947,#11948,#11949,#11950));
#4682=EDGE_LOOP('',(#11951,#11952,#11953,#11954));
#4683=EDGE_LOOP('',(#11955,#11956,#11957,#11958));
#4684=EDGE_LOOP('',(#11959,#11960,#11961,#11962));
#4685=EDGE_LOOP('',(#11963,#11964,#11965,#11966));
#4686=EDGE_LOOP('',(#11967,#11968,#11969,#11970));
#4687=EDGE_LOOP('',(#11971,#11972,#11973,#11974));
#4688=EDGE_LOOP('',(#11975,#11976,#11977,#11978));
#4689=EDGE_LOOP('',(#11979,#11980,#11981,#11982));
#4690=EDGE_LOOP('',(#11983,#11984,#11985,#11986));
#4691=EDGE_LOOP('',(#11987,#11988,#11989,#11990));
#4692=EDGE_LOOP('',(#11991,#11992,#11993,#11994));
#4693=EDGE_LOOP('',(#11995,#11996,#11997,#11998));
#4694=EDGE_LOOP('',(#11999,#12000,#12001,#12002));
#4695=EDGE_LOOP('',(#12003,#12004,#12005,#12006));
#4696=EDGE_LOOP('',(#12007,#12008,#12009,#12010));
#4697=EDGE_LOOP('',(#12011,#12012,#12013,#12014));
#4698=EDGE_LOOP('',(#12015,#12016,#12017,#12018));
#4699=EDGE_LOOP('',(#12019,#12020,#12021,#12022));
#4700=EDGE_LOOP('',(#12023,#12024,#12025,#12026));
#4701=EDGE_LOOP('',(#12027,#12028,#12029,#12030));
#4702=EDGE_LOOP('',(#12031,#12032,#12033,#12034));
#4703=EDGE_LOOP('',(#12035,#12036,#12037,#12038));
#4704=EDGE_LOOP('',(#12039,#12040,#12041,#12042));
#4705=EDGE_LOOP('',(#12043,#12044,#12045,#12046));
#4706=EDGE_LOOP('',(#12047,#12048,#12049,#12050));
#4707=EDGE_LOOP('',(#12051,#12052,#12053,#12054));
#4708=EDGE_LOOP('',(#12055,#12056,#12057,#12058));
#4709=EDGE_LOOP('',(#12059,#12060,#12061,#12062));
#4710=EDGE_LOOP('',(#12063,#12064,#12065,#12066));
#4711=EDGE_LOOP('',(#12067,#12068,#12069,#12070));
#4712=EDGE_LOOP('',(#12071,#12072,#12073,#12074));
#4713=EDGE_LOOP('',(#12075,#12076,#12077,#12078));
#4714=EDGE_LOOP('',(#12079,#12080,#12081,#12082));
#4715=EDGE_LOOP('',(#12083,#12084,#12085,#12086));
#4716=EDGE_LOOP('',(#12087,#12088,#12089,#12090));
#4717=EDGE_LOOP('',(#12091,#12092,#12093,#12094));
#4718=EDGE_LOOP('',(#12095,#12096,#12097,#12098));
#4719=EDGE_LOOP('',(#12099,#12100,#12101,#12102));
#4720=EDGE_LOOP('',(#12103,#12104,#12105,#12106));
#4721=EDGE_LOOP('',(#12107,#12108,#12109,#12110));
#4722=EDGE_LOOP('',(#12111,#12112,#12113,#12114));
#4723=EDGE_LOOP('',(#12115,#12116,#12117,#12118));
#4724=EDGE_LOOP('',(#12119,#12120,#12121,#12122));
#4725=EDGE_LOOP('',(#12123,#12124,#12125,#12126));
#4726=EDGE_LOOP('',(#12127,#12128,#12129,#12130));
#4727=EDGE_LOOP('',(#12131,#12132,#12133,#12134));
#4728=EDGE_LOOP('',(#12135,#12136,#12137,#12138));
#4729=EDGE_LOOP('',(#12139,#12140,#12141,#12142));
#4730=EDGE_LOOP('',(#12143,#12144,#12145,#12146));
#4731=EDGE_LOOP('',(#12147,#12148,#12149,#12150));
#4732=EDGE_LOOP('',(#12151,#12152,#12153,#12154));
#4733=EDGE_LOOP('',(#12155,#12156,#12157,#12158));
#4734=EDGE_LOOP('',(#12159,#12160,#12161,#12162));
#4735=EDGE_LOOP('',(#12163,#12164,#12165,#12166));
#4736=EDGE_LOOP('',(#12167,#12168,#12169,#12170));
#4737=EDGE_LOOP('',(#12171,#12172,#12173,#12174));
#4738=EDGE_LOOP('',(#12175,#12176,#12177,#12178));
#4739=EDGE_LOOP('',(#12179,#12180,#12181,#12182,#12183));
#4740=EDGE_LOOP('',(#12184,#12185,#12186,#12187,#12188,#12189,#12190));
#4741=EDGE_LOOP('',(#12191,#12192,#12193,#12194,#12195,#12196));
#4742=EDGE_LOOP('',(#12197,#12198,#12199,#12200,#12201));
#4743=EDGE_LOOP('',(#12202,#12203,#12204,#12205,#12206,#12207));
#4744=EDGE_LOOP('',(#12208,#12209,#12210,#12211,#12212));
#4745=EDGE_LOOP('',(#12213));
#4746=EDGE_LOOP('',(#12214));
#4747=EDGE_LOOP('',(#12215));
#4748=EDGE_LOOP('',(#12216));
#4749=EDGE_LOOP('',(#12217,#12218,#12219,#12220,#12221));
#4750=EDGE_LOOP('',(#12222,#12223,#12224,#12225,#12226));
#4751=EDGE_LOOP('',(#12227,#12228,#12229,#12230,#12231));
#4752=EDGE_LOOP('',(#12232,#12233,#12234,#12235,#12236));
#4753=EDGE_LOOP('',(#12237,#12238,#12239,#12240,#12241));
#4754=EDGE_LOOP('',(#12242,#12243,#12244,#12245,#12246));
#4755=EDGE_LOOP('',(#12247,#12248,#12249,#12250,#12251));
#4756=EDGE_LOOP('',(#12252,#12253,#12254,#12255,#12256));
#4757=EDGE_LOOP('',(#12257,#12258,#12259,#12260,#12261));
#4758=EDGE_LOOP('',(#12262,#12263,#12264,#12265,#12266));
#4759=EDGE_LOOP('',(#12267,#12268,#12269,#12270,#12271));
#4760=EDGE_LOOP('',(#12272,#12273,#12274,#12275,#12276));
#4761=EDGE_LOOP('',(#12277,#12278,#12279,#12280,#12281));
#4762=EDGE_LOOP('',(#12282,#12283,#12284,#12285,#12286,#12287));
#4763=EDGE_LOOP('',(#12288,#12289,#12290));
#4764=EDGE_LOOP('',(#12291));
#4765=EDGE_LOOP('',(#12292));
#4766=EDGE_LOOP('',(#12293,#12294,#12295,#12296));
#4767=EDGE_LOOP('',(#12297,#12298,#12299,#12300));
#4768=EDGE_LOOP('',(#12301,#12302,#12303,#12304,#12305));
#4769=EDGE_LOOP('',(#12306,#12307,#12308,#12309));
#4770=EDGE_LOOP('',(#12310,#12311,#12312,#12313,#12314));
#4771=EDGE_LOOP('',(#12315,#12316,#12317,#12318,#12319));
#4772=EDGE_LOOP('',(#12320,#12321,#12322,#12323,#12324));
#4773=EDGE_LOOP('',(#12325,#12326,#12327,#12328,#12329));
#4774=EDGE_LOOP('',(#12330,#12331,#12332,#12333,#12334));
#4775=EDGE_LOOP('',(#12335,#12336,#12337,#12338,#12339,#12340));
#4776=EDGE_LOOP('',(#12341,#12342,#12343,#12344,#12345,#12346));
#4777=EDGE_LOOP('',(#12347,#12348,#12349,#12350));
#4778=EDGE_LOOP('',(#12351,#12352,#12353,#12354,#12355,#12356));
#4779=EDGE_LOOP('',(#12357,#12358,#12359,#12360));
#4780=EDGE_LOOP('',(#12361,#12362,#12363,#12364,#12365,#12366));
#4781=EDGE_LOOP('',(#12367,#12368,#12369,#12370));
#4782=EDGE_LOOP('',(#12371,#12372,#12373,#12374));
#4783=EDGE_LOOP('',(#12375,#12376,#12377,#12378,#12379,#12380));
#4784=EDGE_LOOP('',(#12381,#12382,#12383,#12384));
#4785=EDGE_LOOP('',(#12385,#12386,#12387,#12388,#12389,#12390));
#4786=EDGE_LOOP('',(#12391,#12392,#12393,#12394,#12395));
#4787=EDGE_LOOP('',(#12396,#12397,#12398,#12399));
#4788=EDGE_LOOP('',(#12400,#12401,#12402,#12403,#12404,#12405));
#4789=EDGE_LOOP('',(#12406,#12407,#12408,#12409));
#4790=EDGE_LOOP('',(#12410,#12411,#12412,#12413,#12414));
#4791=EDGE_LOOP('',(#12415,#12416));
#4792=EDGE_LOOP('',(#12417,#12418,#12419,#12420,#12421,#12422,#12423));
#4793=EDGE_LOOP('',(#12424,#12425,#12426,#12427,#12428,#12429,#12430,#12431,
#12432,#12433,#12434,#12435,#12436,#12437));
#4794=EDGE_LOOP('',(#12438,#12439,#12440,#12441,#12442,#12443,#12444,#12445,
#12446,#12447,#12448,#12449,#12450,#12451,#12452,#12453,#12454,#12455,#12456,
#12457,#12458,#12459,#12460,#12461,#12462,#12463,#12464,#12465,#12466,#12467,
#12468,#12469,#12470,#12471,#12472,#12473,#12474,#12475,#12476,#12477,#12478,
#12479,#12480,#12481,#12482,#12483,#12484,#12485,#12486,#12487,#12488,#12489,
#12490,#12491,#12492,#12493,#12494,#12495,#12496,#12497,#12498,#12499,#12500,
#12501,#12502,#12503,#12504,#12505,#12506,#12507,#12508,#12509,#12510,#12511,
#12512,#12513,#12514,#12515,#12516,#12517,#12518,#12519,#12520,#12521,#12522,
#12523,#12524,#12525,#12526,#12527,#12528,#12529,#12530,#12531,#12532,#12533,
#12534,#12535,#12536,#12537,#12538,#12539,#12540,#12541,#12542,#12543,#12544,
#12545,#12546,#12547,#12548,#12549,#12550,#12551,#12552,#12553,#12554,#12555,
#12556,#12557,#12558,#12559,#12560,#12561,#12562,#12563,#12564,#12565,#12566,
#12567,#12568,#12569,#12570,#12571,#12572,#12573,#12574,#12575,#12576));
#4795=EDGE_LOOP('',(#12577,#12578,#12579,#12580,#12581,#12582,#12583,#12584,
#12585,#12586,#12587,#12588,#12589,#12590,#12591,#12592,#12593,#12594,#12595,
#12596,#12597,#12598,#12599,#12600,#12601,#12602,#12603,#12604,#12605,#12606,
#12607,#12608,#12609,#12610,#12611,#12612,#12613));
#4796=EDGE_LOOP('',(#12614,#12615,#12616,#12617));
#4797=EDGE_LOOP('',(#12618,#12619,#12620,#12621));
#4798=EDGE_LOOP('',(#12622,#12623,#12624,#12625,#12626,#12627));
#4799=EDGE_LOOP('',(#12628,#12629,#12630,#12631));
#4800=EDGE_LOOP('',(#12632,#12633,#12634,#12635,#12636,#12637,#12638,#12639,
#12640,#12641,#12642,#12643,#12644,#12645,#12646,#12647,#12648,#12649,#12650,
#12651,#12652,#12653,#12654,#12655,#12656,#12657,#12658,#12659,#12660,#12661,
#12662,#12663,#12664,#12665,#12666,#12667,#12668,#12669,#12670,#12671,#12672,
#12673,#12674,#12675,#12676,#12677,#12678,#12679,#12680,#12681,#12682,#12683,
#12684,#12685,#12686,#12687,#12688,#12689,#12690,#12691,#12692,#12693,#12694,
#12695,#12696,#12697,#12698,#12699,#12700,#12701,#12702,#12703,#12704,#12705,
#12706,#12707,#12708,#12709,#12710,#12711,#12712,#12713,#12714,#12715,#12716,
#12717,#12718,#12719,#12720,#12721,#12722,#12723,#12724,#12725,#12726,#12727,
#12728,#12729,#12730,#12731,#12732,#12733,#12734,#12735,#12736,#12737,#12738,
#12739,#12740,#12741,#12742,#12743,#12744,#12745,#12746,#12747,#12748,#12749,
#12750,#12751,#12752,#12753,#12754,#12755,#12756,#12757,#12758,#12759,#12760,
#12761,#12762,#12763));
#4801=EDGE_LOOP('',(#12764,#12765,#12766,#12767,#12768,#12769));
#4802=EDGE_LOOP('',(#12770,#12771,#12772,#12773,#12774,#12775));
#4803=EDGE_LOOP('',(#12776,#12777,#12778,#12779,#12780,#12781));
#4804=EDGE_LOOP('',(#12782,#12783,#12784,#12785,#12786,#12787));
#4805=EDGE_LOOP('',(#12788,#12789,#12790,#12791,#12792,#12793));
#4806=EDGE_LOOP('',(#12794,#12795,#12796,#12797,#12798,#12799));
#4807=EDGE_LOOP('',(#12800,#12801,#12802,#12803,#12804,#12805,#12806,#12807,
#12808,#12809));
#4808=EDGE_LOOP('',(#12810,#12811,#12812,#12813,#12814,#12815));
#4809=EDGE_LOOP('',(#12816,#12817,#12818,#12819,#12820,#12821));
#4810=EDGE_LOOP('',(#12822,#12823,#12824,#12825,#12826,#12827));
#4811=EDGE_LOOP('',(#12828,#12829,#12830,#12831,#12832,#12833));
#4812=EDGE_LOOP('',(#12834,#12835,#12836,#12837,#12838,#12839));
#4813=EDGE_LOOP('',(#12840,#12841,#12842,#12843,#12844,#12845,#12846,#12847,
#12848,#12849));
#4814=EDGE_LOOP('',(#12850,#12851,#12852,#12853,#12854,#12855,#12856,#12857,
#12858,#12859));
#4815=EDGE_LOOP('',(#12860,#12861,#12862,#12863,#12864,#12865,#12866,#12867,
#12868,#12869,#12870,#12871));
#4816=EDGE_LOOP('',(#12872,#12873,#12874,#12875,#12876,#12877,#12878,#12879));
#4817=EDGE_LOOP('',(#12880,#12881,#12882,#12883,#12884,#12885,#12886,#12887,
#12888,#12889,#12890));
#4818=EDGE_LOOP('',(#12891,#12892,#12893,#12894));
#4819=EDGE_LOOP('',(#12895,#12896,#12897,#12898));
#4820=EDGE_LOOP('',(#12899,#12900,#12901,#12902));
#4821=EDGE_LOOP('',(#12903,#12904,#12905,#12906));
#4822=EDGE_LOOP('',(#12907,#12908,#12909,#12910,#12911));
#4823=EDGE_LOOP('',(#12912,#12913,#12914,#12915,#12916));
#4824=EDGE_LOOP('',(#12917,#12918,#12919,#12920,#12921));
#4825=EDGE_LOOP('',(#12922,#12923,#12924,#12925,#12926));
#4826=EDGE_LOOP('',(#12927,#12928,#12929,#12930));
#4827=EDGE_LOOP('',(#12931,#12932,#12933,#12934,#12935,#12936,#12937,#12938,
#12939,#12940,#12941,#12942,#12943,#12944,#12945,#12946,#12947));
#4828=EDGE_LOOP('',(#12948,#12949,#12950,#12951,#12952,#12953,#12954));
#4829=EDGE_LOOP('',(#12955,#12956,#12957,#12958,#12959,#12960));
#4830=EDGE_LOOP('',(#12961,#12962,#12963,#12964,#12965,#12966));
#4831=EDGE_LOOP('',(#12967,#12968,#12969,#12970,#12971,#12972,#12973));
#4832=EDGE_LOOP('',(#12974,#12975,#12976,#12977,#12978,#12979,#12980));
#4833=EDGE_LOOP('',(#12981,#12982,#12983,#12984,#12985,#12986,#12987,#12988,
#12989,#12990,#12991,#12992));
#4834=EDGE_LOOP('',(#12993,#12994,#12995,#12996,#12997,#12998,#12999,#13000,
#13001,#13002,#13003,#13004));
#4835=EDGE_LOOP('',(#13005,#13006,#13007,#13008,#13009,#13010,#13011));
#4836=EDGE_LOOP('',(#13012,#13013,#13014,#13015));
#4837=EDGE_LOOP('',(#13016,#13017,#13018,#13019));
#4838=EDGE_LOOP('',(#13020,#13021,#13022,#13023));
#4839=EDGE_LOOP('',(#13024,#13025,#13026,#13027));
#4840=EDGE_LOOP('',(#13028,#13029,#13030,#13031,#13032));
#4841=EDGE_LOOP('',(#13033,#13034,#13035,#13036));
#4842=EDGE_LOOP('',(#13037,#13038,#13039,#13040));
#4843=EDGE_LOOP('',(#13041,#13042,#13043,#13044,#13045,#13046,#13047));
#4844=EDGE_LOOP('',(#13048,#13049,#13050,#13051,#13052));
#4845=EDGE_LOOP('',(#13053,#13054,#13055,#13056));
#4846=EDGE_LOOP('',(#13057,#13058,#13059,#13060));
#4847=EDGE_LOOP('',(#13061,#13062,#13063,#13064,#13065));
#4848=EDGE_LOOP('',(#13066,#13067,#13068,#13069,#13070));
#4849=EDGE_LOOP('',(#13071,#13072,#13073,#13074));
#4850=EDGE_LOOP('',(#13075,#13076,#13077,#13078));
#4851=EDGE_LOOP('',(#13079,#13080,#13081,#13082,#13083,#13084));
#4852=EDGE_LOOP('',(#13085,#13086,#13087,#13088,#13089));
#4853=EDGE_LOOP('',(#13090,#13091,#13092,#13093,#13094,#13095,#13096,#13097));
#4854=EDGE_LOOP('',(#13098,#13099,#13100,#13101,#13102,#13103,#13104,#13105,
#13106));
#4855=EDGE_LOOP('',(#13107,#13108,#13109,#13110,#13111));
#4856=EDGE_LOOP('',(#13112,#13113,#13114));
#4857=EDGE_LOOP('',(#13115,#13116,#13117,#13118));
#4858=EDGE_LOOP('',(#13119,#13120,#13121,#13122,#13123));
#4859=EDGE_LOOP('',(#13124,#13125,#13126,#13127,#13128,#13129));
#4860=EDGE_LOOP('',(#13130,#13131,#13132,#13133,#13134));
#4861=EDGE_LOOP('',(#13135,#13136,#13137,#13138,#13139));
#4862=EDGE_LOOP('',(#13140,#13141,#13142,#13143));
#4863=EDGE_LOOP('',(#13144,#13145,#13146,#13147));
#4864=EDGE_LOOP('',(#13148,#13149,#13150,#13151));
#4865=EDGE_LOOP('',(#13152,#13153,#13154));
#4866=EDGE_LOOP('',(#13155,#13156,#13157,#13158));
#4867=EDGE_LOOP('',(#13159,#13160,#13161,#13162));
#4868=EDGE_LOOP('',(#13163,#13164,#13165));
#4869=EDGE_LOOP('',(#13166,#13167,#13168,#13169));
#4870=EDGE_LOOP('',(#13170,#13171,#13172));
#4871=EDGE_LOOP('',(#13173,#13174,#13175,#13176));
#4872=EDGE_LOOP('',(#13177,#13178,#13179,#13180));
#4873=EDGE_LOOP('',(#13181,#13182,#13183,#13184,#13185,#13186,#13187));
#4874=EDGE_LOOP('',(#13188,#13189,#13190,#13191,#13192));
#4875=EDGE_LOOP('',(#13193,#13194,#13195,#13196,#13197));
#4876=EDGE_LOOP('',(#13198,#13199,#13200));
#4877=EDGE_LOOP('',(#13201,#13202,#13203,#13204));
#4878=EDGE_LOOP('',(#13205,#13206,#13207));
#4879=EDGE_LOOP('',(#13208,#13209,#13210,#13211,#13212,#13213,#13214,#13215,
#13216,#13217));
#4880=EDGE_LOOP('',(#13218,#13219,#13220,#13221,#13222,#13223,#13224));
#4881=EDGE_LOOP('',(#13225,#13226,#13227,#13228,#13229,#13230,#13231));
#4882=EDGE_LOOP('',(#13232,#13233,#13234,#13235,#13236,#13237,#13238,#13239));
#4883=EDGE_LOOP('',(#13240,#13241,#13242,#13243));
#4884=EDGE_LOOP('',(#13244,#13245,#13246,#13247,#13248,#13249,#13250,#13251));
#4885=EDGE_LOOP('',(#13252,#13253,#13254,#13255,#13256,#13257));
#4886=EDGE_LOOP('',(#13258,#13259,#13260,#13261,#13262,#13263));
#4887=EDGE_LOOP('',(#13264,#13265,#13266,#13267,#13268,#13269));
#4888=EDGE_LOOP('',(#13270,#13271,#13272,#13273,#13274,#13275));
#4889=EDGE_LOOP('',(#13276,#13277,#13278,#13279,#13280,#13281));
#4890=EDGE_LOOP('',(#13282,#13283,#13284,#13285,#13286,#13287));
#4891=EDGE_LOOP('',(#13288,#13289,#13290,#13291,#13292,#13293));
#4892=EDGE_LOOP('',(#13294,#13295,#13296,#13297,#13298,#13299));
#4893=EDGE_LOOP('',(#13300,#13301,#13302,#13303,#13304,#13305));
#4894=EDGE_LOOP('',(#13306,#13307,#13308,#13309,#13310,#13311));
#4895=EDGE_LOOP('',(#13312,#13313,#13314,#13315,#13316,#13317));
#4896=EDGE_LOOP('',(#13318,#13319,#13320,#13321,#13322,#13323));
#4897=EDGE_LOOP('',(#13324,#13325,#13326,#13327,#13328,#13329));
#4898=EDGE_LOOP('',(#13330,#13331,#13332,#13333,#13334,#13335));
#4899=EDGE_LOOP('',(#13336,#13337,#13338,#13339,#13340,#13341));
#4900=EDGE_LOOP('',(#13342,#13343,#13344,#13345,#13346,#13347));
#4901=EDGE_LOOP('',(#13348,#13349,#13350,#13351,#13352,#13353));
#4902=EDGE_LOOP('',(#13354,#13355,#13356,#13357));
#4903=EDGE_LOOP('',(#13358,#13359,#13360,#13361));
#4904=EDGE_LOOP('',(#13362,#13363,#13364,#13365,#13366,#13367));
#4905=EDGE_LOOP('',(#13368,#13369,#13370,#13371,#13372,#13373));
#4906=EDGE_LOOP('',(#13374,#13375,#13376,#13377,#13378,#13379));
#4907=EDGE_LOOP('',(#13380,#13381,#13382,#13383,#13384,#13385));
#4908=EDGE_LOOP('',(#13386,#13387,#13388,#13389,#13390,#13391));
#4909=EDGE_LOOP('',(#13392,#13393,#13394,#13395,#13396,#13397));
#4910=EDGE_LOOP('',(#13398,#13399,#13400,#13401,#13402,#13403));
#4911=EDGE_LOOP('',(#13404,#13405,#13406,#13407,#13408,#13409));
#4912=EDGE_LOOP('',(#13410,#13411,#13412,#13413,#13414,#13415));
#4913=EDGE_LOOP('',(#13416,#13417,#13418,#13419,#13420,#13421));
#4914=EDGE_LOOP('',(#13422,#13423,#13424,#13425,#13426,#13427));
#4915=EDGE_LOOP('',(#13428,#13429,#13430,#13431,#13432,#13433));
#4916=EDGE_LOOP('',(#13434,#13435,#13436,#13437,#13438,#13439));
#4917=EDGE_LOOP('',(#13440,#13441,#13442,#13443,#13444,#13445));
#4918=EDGE_LOOP('',(#13446,#13447,#13448,#13449,#13450,#13451));
#4919=EDGE_LOOP('',(#13452,#13453,#13454,#13455,#13456,#13457));
#4920=EDGE_LOOP('',(#13458,#13459,#13460,#13461,#13462,#13463));
#4921=EDGE_LOOP('',(#13464,#13465,#13466,#13467));
#4922=EDGE_LOOP('',(#13468,#13469,#13470,#13471));
#4923=EDGE_LOOP('',(#13472,#13473,#13474,#13475));
#4924=EDGE_LOOP('',(#13476,#13477,#13478,#13479));
#4925=EDGE_LOOP('',(#13480,#13481,#13482,#13483));
#4926=EDGE_LOOP('',(#13484,#13485,#13486,#13487));
#4927=EDGE_LOOP('',(#13488,#13489,#13490,#13491));
#4928=EDGE_LOOP('',(#13492,#13493,#13494,#13495));
#4929=EDGE_LOOP('',(#13496,#13497,#13498,#13499));
#4930=EDGE_LOOP('',(#13500,#13501,#13502,#13503));
#4931=EDGE_LOOP('',(#13504,#13505,#13506,#13507));
#4932=EDGE_LOOP('',(#13508,#13509,#13510,#13511));
#4933=EDGE_LOOP('',(#13512,#13513,#13514,#13515));
#4934=EDGE_LOOP('',(#13516,#13517,#13518,#13519));
#4935=EDGE_LOOP('',(#13520,#13521,#13522,#13523));
#4936=EDGE_LOOP('',(#13524,#13525,#13526,#13527));
#4937=EDGE_LOOP('',(#13528,#13529,#13530,#13531));
#4938=EDGE_LOOP('',(#13532,#13533,#13534,#13535));
#4939=EDGE_LOOP('',(#13536,#13537,#13538,#13539));
#4940=EDGE_LOOP('',(#13540,#13541,#13542,#13543));
#4941=EDGE_LOOP('',(#13544,#13545,#13546,#13547));
#4942=EDGE_LOOP('',(#13548,#13549,#13550,#13551));
#4943=EDGE_LOOP('',(#13552,#13553,#13554,#13555));
#4944=EDGE_LOOP('',(#13556,#13557,#13558,#13559));
#4945=EDGE_LOOP('',(#13560,#13561,#13562,#13563));
#4946=EDGE_LOOP('',(#13564,#13565,#13566,#13567));
#4947=EDGE_LOOP('',(#13568,#13569,#13570,#13571));
#4948=EDGE_LOOP('',(#13572,#13573,#13574,#13575));
#4949=EDGE_LOOP('',(#13576,#13577,#13578,#13579));
#4950=EDGE_LOOP('',(#13580,#13581,#13582,#13583));
#4951=EDGE_LOOP('',(#13584,#13585,#13586,#13587));
#4952=EDGE_LOOP('',(#13588,#13589,#13590,#13591));
#4953=EDGE_LOOP('',(#13592,#13593,#13594,#13595));
#4954=EDGE_LOOP('',(#13596,#13597,#13598,#13599));
#4955=EDGE_LOOP('',(#13600,#13601,#13602,#13603));
#4956=EDGE_LOOP('',(#13604,#13605,#13606,#13607));
#4957=EDGE_LOOP('',(#13608,#13609,#13610,#13611));
#4958=EDGE_LOOP('',(#13612,#13613,#13614,#13615));
#4959=EDGE_LOOP('',(#13616,#13617,#13618,#13619,#13620));
#4960=EDGE_LOOP('',(#13621,#13622,#13623,#13624));
#4961=EDGE_LOOP('',(#13625,#13626,#13627,#13628,#13629));
#4962=EDGE_LOOP('',(#13630,#13631,#13632,#13633,#13634));
#4963=EDGE_LOOP('',(#13635,#13636,#13637,#13638));
#4964=EDGE_LOOP('',(#13639,#13640,#13641,#13642,#13643));
#4965=EDGE_LOOP('',(#13644,#13645,#13646,#13647));
#4966=EDGE_LOOP('',(#13648,#13649,#13650,#13651));
#4967=EDGE_LOOP('',(#13652,#13653,#13654,#13655));
#4968=EDGE_LOOP('',(#13656,#13657,#13658,#13659));
#4969=EDGE_LOOP('',(#13660,#13661,#13662,#13663));
#4970=EDGE_LOOP('',(#13664,#13665,#13666,#13667));
#4971=EDGE_LOOP('',(#13668,#13669,#13670,#13671));
#4972=EDGE_LOOP('',(#13672,#13673,#13674,#13675));
#4973=EDGE_LOOP('',(#13676,#13677,#13678,#13679));
#4974=EDGE_LOOP('',(#13680,#13681,#13682,#13683));
#4975=EDGE_LOOP('',(#13684,#13685,#13686,#13687));
#4976=EDGE_LOOP('',(#13688,#13689,#13690,#13691));
#4977=EDGE_LOOP('',(#13692,#13693,#13694,#13695));
#4978=EDGE_LOOP('',(#13696,#13697,#13698,#13699));
#4979=EDGE_LOOP('',(#13700,#13701,#13702,#13703));
#4980=EDGE_LOOP('',(#13704,#13705,#13706,#13707));
#4981=EDGE_LOOP('',(#13708,#13709,#13710,#13711));
#4982=EDGE_LOOP('',(#13712,#13713,#13714,#13715));
#4983=EDGE_LOOP('',(#13716,#13717,#13718,#13719));
#4984=EDGE_LOOP('',(#13720,#13721,#13722,#13723));
#4985=EDGE_LOOP('',(#13724,#13725,#13726,#13727));
#4986=EDGE_LOOP('',(#13728,#13729,#13730,#13731));
#4987=EDGE_LOOP('',(#13732,#13733,#13734,#13735));
#4988=EDGE_LOOP('',(#13736,#13737,#13738,#13739));
#4989=EDGE_LOOP('',(#13740,#13741,#13742,#13743));
#4990=EDGE_LOOP('',(#13744,#13745,#13746,#13747));
#4991=EDGE_LOOP('',(#13748,#13749,#13750,#13751));
#4992=EDGE_LOOP('',(#13752,#13753,#13754,#13755));
#4993=EDGE_LOOP('',(#13756,#13757,#13758,#13759));
#4994=EDGE_LOOP('',(#13760,#13761,#13762,#13763));
#4995=EDGE_LOOP('',(#13764,#13765,#13766,#13767,#13768));
#4996=EDGE_LOOP('',(#13769,#13770,#13771,#13772));
#4997=EDGE_LOOP('',(#13773,#13774,#13775,#13776,#13777));
#4998=EDGE_LOOP('',(#13778,#13779,#13780,#13781,#13782));
#4999=EDGE_LOOP('',(#13783,#13784,#13785,#13786));
#5000=EDGE_LOOP('',(#13787,#13788,#13789,#13790,#13791));
#5001=EDGE_LOOP('',(#13792,#13793,#13794,#13795,#13796));
#5002=EDGE_LOOP('',(#13797,#13798,#13799,#13800));
#5003=EDGE_LOOP('',(#13801,#13802,#13803,#13804,#13805));
#5004=EDGE_LOOP('',(#13806,#13807,#13808,#13809,#13810));
#5005=EDGE_LOOP('',(#13811,#13812,#13813,#13814));
#5006=EDGE_LOOP('',(#13815,#13816,#13817,#13818,#13819));
#5007=EDGE_LOOP('',(#13820,#13821,#13822,#13823));
#5008=EDGE_LOOP('',(#13824,#13825,#13826,#13827));
#5009=EDGE_LOOP('',(#13828,#13829,#13830,#13831,#13832,#13833,#13834));
#5010=EDGE_LOOP('',(#13835,#13836,#13837,#13838,#13839));
#5011=EDGE_LOOP('',(#13840,#13841,#13842,#13843,#13844));
#5012=EDGE_LOOP('',(#13845,#13846,#13847,#13848,#13849));
#5013=EDGE_LOOP('',(#13850,#13851,#13852,#13853,#13854));
#5014=EDGE_LOOP('',(#13855,#13856,#13857,#13858));
#5015=EDGE_LOOP('',(#13859,#13860,#13861,#13862,#13863));
#5016=EDGE_LOOP('',(#13864,#13865,#13866,#13867));
#5017=EDGE_LOOP('',(#13868,#13869,#13870,#13871));
#5018=EDGE_LOOP('',(#13872,#13873,#13874,#13875));
#5019=EDGE_LOOP('',(#13876,#13877,#13878,#13879,#13880));
#5020=EDGE_LOOP('',(#13881,#13882,#13883,#13884));
#5021=EDGE_LOOP('',(#13885,#13886,#13887,#13888));
#5022=EDGE_LOOP('',(#13889,#13890,#13891,#13892,#13893,#13894,#13895));
#5023=EDGE_LOOP('',(#13896,#13897,#13898,#13899));
#5024=EDGE_LOOP('',(#13900,#13901,#13902,#13903,#13904));
#5025=EDGE_LOOP('',(#13905,#13906,#13907,#13908,#13909));
#5026=EDGE_LOOP('',(#13910,#13911,#13912,#13913));
#5027=EDGE_LOOP('',(#13914,#13915,#13916,#13917));
#5028=EDGE_LOOP('',(#13918,#13919,#13920,#13921));
#5029=EDGE_LOOP('',(#13922,#13923,#13924,#13925,#13926));
#5030=EDGE_LOOP('',(#13927,#13928,#13929,#13930));
#5031=EDGE_LOOP('',(#13931,#13932,#13933,#13934,#13935));
#5032=EDGE_LOOP('',(#13936,#13937,#13938,#13939));
#5033=EDGE_LOOP('',(#13940,#13941,#13942,#13943));
#5034=EDGE_LOOP('',(#13944,#13945,#13946,#13947));
#5035=EDGE_LOOP('',(#13948,#13949,#13950,#13951,#13952));
#5036=EDGE_LOOP('',(#13953,#13954,#13955,#13956));
#5037=EDGE_LOOP('',(#13957,#13958,#13959,#13960,#13961));
#5038=EDGE_LOOP('',(#13962,#13963,#13964,#13965));
#5039=EDGE_LOOP('',(#13966,#13967,#13968,#13969));
#5040=EDGE_LOOP('',(#13970,#13971,#13972,#13973));
#5041=EDGE_LOOP('',(#13974,#13975,#13976,#13977,#13978));
#5042=EDGE_LOOP('',(#13979,#13980,#13981,#13982));
#5043=EDGE_LOOP('',(#13983,#13984,#13985,#13986,#13987));
#5044=EDGE_LOOP('',(#13988,#13989,#13990,#13991));
#5045=EDGE_LOOP('',(#13992,#13993,#13994,#13995));
#5046=EDGE_LOOP('',(#13996,#13997,#13998,#13999));
#5047=EDGE_LOOP('',(#14000,#14001,#14002,#14003,#14004));
#5048=EDGE_LOOP('',(#14005,#14006,#14007,#14008));
#5049=EDGE_LOOP('',(#14009,#14010,#14011,#14012,#14013));
#5050=EDGE_LOOP('',(#14014,#14015,#14016,#14017));
#5051=EDGE_LOOP('',(#14018,#14019,#14020,#14021));
#5052=EDGE_LOOP('',(#14022,#14023,#14024,#14025));
#5053=EDGE_LOOP('',(#14026,#14027,#14028,#14029,#14030));
#5054=EDGE_LOOP('',(#14031,#14032,#14033,#14034));
#5055=EDGE_LOOP('',(#14035,#14036,#14037,#14038,#14039));
#5056=EDGE_LOOP('',(#14040,#14041,#14042,#14043));
#5057=EDGE_LOOP('',(#14044,#14045,#14046,#14047));
#5058=EDGE_LOOP('',(#14048,#14049,#14050,#14051));
#5059=EDGE_LOOP('',(#14052,#14053,#14054,#14055,#14056));
#5060=EDGE_LOOP('',(#14057,#14058,#14059,#14060));
#5061=EDGE_LOOP('',(#14061,#14062,#14063,#14064,#14065,#14066));
#5062=EDGE_LOOP('',(#14067,#14068,#14069,#14070,#14071));
#5063=EDGE_LOOP('',(#14072,#14073,#14074,#14075));
#5064=EDGE_LOOP('',(#14076,#14077,#14078,#14079));
#5065=EDGE_LOOP('',(#14080,#14081,#14082,#14083,#14084,#14085));
#5066=EDGE_LOOP('',(#14086,#14087,#14088,#14089,#14090));
#5067=EDGE_LOOP('',(#14091,#14092,#14093,#14094,#14095));
#5068=EDGE_LOOP('',(#14096,#14097,#14098,#14099));
#5069=EDGE_LOOP('',(#14100,#14101,#14102,#14103));
#5070=EDGE_LOOP('',(#14104,#14105,#14106,#14107));
#5071=EDGE_LOOP('',(#14108,#14109,#14110,#14111,#14112));
#5072=EDGE_LOOP('',(#14113,#14114,#14115,#14116));
#5073=EDGE_LOOP('',(#14117,#14118,#14119,#14120,#14121));
#5074=EDGE_LOOP('',(#14122,#14123,#14124,#14125));
#5075=EDGE_LOOP('',(#14126,#14127,#14128,#14129));
#5076=EDGE_LOOP('',(#14130,#14131,#14132,#14133));
#5077=EDGE_LOOP('',(#14134,#14135,#14136,#14137,#14138));
#5078=EDGE_LOOP('',(#14139,#14140,#14141,#14142));
#5079=EDGE_LOOP('',(#14143,#14144,#14145,#14146,#14147));
#5080=EDGE_LOOP('',(#14148,#14149,#14150,#14151));
#5081=EDGE_LOOP('',(#14152,#14153,#14154,#14155));
#5082=EDGE_LOOP('',(#14156,#14157,#14158,#14159));
#5083=EDGE_LOOP('',(#14160,#14161,#14162,#14163,#14164));
#5084=EDGE_LOOP('',(#14165,#14166,#14167,#14168));
#5085=EDGE_LOOP('',(#14169,#14170,#14171,#14172,#14173));
#5086=EDGE_LOOP('',(#14174,#14175,#14176,#14177));
#5087=EDGE_LOOP('',(#14178,#14179,#14180,#14181));
#5088=EDGE_LOOP('',(#14182,#14183,#14184,#14185));
#5089=EDGE_LOOP('',(#14186,#14187,#14188,#14189,#14190));
#5090=EDGE_LOOP('',(#14191,#14192,#14193,#14194));
#5091=EDGE_LOOP('',(#14195,#14196,#14197,#14198,#14199));
#5092=EDGE_LOOP('',(#14200,#14201,#14202,#14203));
#5093=EDGE_LOOP('',(#14204,#14205,#14206,#14207));
#5094=EDGE_LOOP('',(#14208,#14209,#14210,#14211));
#5095=EDGE_LOOP('',(#14212,#14213,#14214,#14215,#14216));
#5096=EDGE_LOOP('',(#14217,#14218,#14219,#14220));
#5097=EDGE_LOOP('',(#14221,#14222,#14223,#14224,#14225,#14226));
#5098=EDGE_LOOP('',(#14227,#14228,#14229,#14230,#14231));
#5099=EDGE_LOOP('',(#14232,#14233,#14234,#14235));
#5100=EDGE_LOOP('',(#14236,#14237,#14238,#14239));
#5101=EDGE_LOOP('',(#14240,#14241,#14242,#14243,#14244,#14245));
#5102=EDGE_LOOP('',(#14246,#14247,#14248,#14249,#14250));
#5103=EDGE_LOOP('',(#14251,#14252,#14253,#14254,#14255,#14256));
#5104=EDGE_LOOP('',(#14257,#14258,#14259,#14260,#14261));
#5105=EDGE_LOOP('',(#14262,#14263,#14264,#14265));
#5106=EDGE_LOOP('',(#14266,#14267,#14268,#14269));
#5107=EDGE_LOOP('',(#14270,#14271,#14272,#14273,#14274,#14275));
#5108=EDGE_LOOP('',(#14276,#14277,#14278,#14279,#14280));
#5109=EDGE_LOOP('',(#14281,#14282,#14283,#14284,#14285,#14286));
#5110=EDGE_LOOP('',(#14287,#14288,#14289,#14290,#14291));
#5111=EDGE_LOOP('',(#14292,#14293,#14294,#14295,#14296));
#5112=EDGE_LOOP('',(#14297,#14298,#14299,#14300,#14301));
#5113=EDGE_LOOP('',(#14302,#14303,#14304,#14305,#14306));
#5114=EDGE_LOOP('',(#14307,#14308,#14309,#14310,#14311,#14312,#14313));
#5115=EDGE_LOOP('',(#14314,#14315,#14316,#14317,#14318));
#5116=EDGE_LOOP('',(#14319,#14320,#14321,#14322));
#5117=EDGE_LOOP('',(#14323,#14324,#14325,#14326));
#5118=EDGE_LOOP('',(#14327,#14328,#14329,#14330));
#5119=EDGE_LOOP('',(#14331,#14332,#14333,#14334,#14335,#14336));
#5120=EDGE_LOOP('',(#14337,#14338,#14339,#14340,#14341));
#5121=EDGE_LOOP('',(#14342,#14343,#14344,#14345,#14346));
#5122=EDGE_LOOP('',(#14347,#14348,#14349,#14350));
#5123=EDGE_LOOP('',(#14351,#14352,#14353,#14354));
#5124=EDGE_LOOP('',(#14355,#14356,#14357,#14358,#14359,#14360,#14361,#14362));
#5125=EDGE_LOOP('',(#14363,#14364,#14365,#14366,#14367));
#5126=EDGE_LOOP('',(#14368,#14369,#14370,#14371,#14372));
#5127=EDGE_LOOP('',(#14373,#14374,#14375,#14376,#14377));
#5128=EDGE_LOOP('',(#14378,#14379,#14380,#14381));
#5129=EDGE_LOOP('',(#14382,#14383,#14384,#14385,#14386));
#5130=EDGE_LOOP('',(#14387,#14388,#14389,#14390));
#5131=EDGE_LOOP('',(#14391,#14392,#14393,#14394,#14395));
#5132=EDGE_LOOP('',(#14396,#14397,#14398,#14399));
#5133=EDGE_LOOP('',(#14400,#14401,#14402,#14403,#14404));
#5134=EDGE_LOOP('',(#14405,#14406,#14407,#14408));
#5135=EDGE_LOOP('',(#14409,#14410,#14411,#14412));
#5136=EDGE_LOOP('',(#14413,#14414,#14415,#14416,#14417,#14418));
#5137=EDGE_LOOP('',(#14419,#14420,#14421,#14422));
#5138=EDGE_LOOP('',(#14423,#14424,#14425,#14426));
#5139=EDGE_LOOP('',(#14427,#14428,#14429,#14430));
#5140=EDGE_LOOP('',(#14431,#14432,#14433,#14434));
#5141=EDGE_LOOP('',(#14435,#14436,#14437,#14438));
#5142=EDGE_LOOP('',(#14439,#14440,#14441,#14442,#14443,#14444));
#5143=EDGE_LOOP('',(#14445,#14446,#14447,#14448));
#5144=EDGE_LOOP('',(#14449,#14450,#14451,#14452));
#5145=EDGE_LOOP('',(#14453,#14454,#14455,#14456));
#5146=EDGE_LOOP('',(#14457,#14458,#14459,#14460));
#5147=EDGE_LOOP('',(#14461,#14462,#14463,#14464,#14465));
#5148=EDGE_LOOP('',(#14466,#14467,#14468,#14469));
#5149=EDGE_LOOP('',(#14470,#14471,#14472,#14473,#14474));
#5150=EDGE_LOOP('',(#14475,#14476,#14477,#14478));
#5151=EDGE_LOOP('',(#14479,#14480,#14481,#14482,#14483,#14484));
#5152=EDGE_LOOP('',(#14485,#14486,#14487,#14488));
#5153=EDGE_LOOP('',(#14489,#14490,#14491,#14492,#14493));
#5154=EDGE_LOOP('',(#14494,#14495,#14496,#14497,#14498));
#5155=EDGE_LOOP('',(#14499,#14500,#14501,#14502));
#5156=EDGE_LOOP('',(#14503,#14504,#14505,#14506,#14507,#14508));
#5157=EDGE_LOOP('',(#14509,#14510,#14511,#14512));
#5158=EDGE_LOOP('',(#14513,#14514,#14515,#14516,#14517));
#5159=EDGE_LOOP('',(#14518,#14519,#14520,#14521));
#5160=EDGE_LOOP('',(#14522,#14523,#14524,#14525));
#5161=EDGE_LOOP('',(#14526,#14527,#14528,#14529));
#5162=EDGE_LOOP('',(#14530,#14531,#14532,#14533,#14534));
#5163=EDGE_LOOP('',(#14535,#14536,#14537,#14538,#14539,#14540));
#5164=EDGE_LOOP('',(#14541,#14542,#14543,#14544,#14545,#14546));
#5165=EDGE_LOOP('',(#14547,#14548,#14549,#14550,#14551,#14552));
#5166=EDGE_LOOP('',(#14553,#14554,#14555,#14556));
#5167=EDGE_LOOP('',(#14557,#14558,#14559,#14560,#14561));
#5168=EDGE_LOOP('',(#14562,#14563,#14564,#14565,#14566,#14567,#14568,#14569,
#14570));
#5169=EDGE_LOOP('',(#14571,#14572,#14573,#14574,#14575,#14576,#14577,#14578,
#14579,#14580,#14581,#14582,#14583,#14584,#14585));
#5170=EDGE_LOOP('',(#14586));
#5171=EDGE_LOOP('',(#14587,#14588,#14589,#14590,#14591,#14592,#14593,#14594));
#5172=EDGE_LOOP('',(#14595,#14596,#14597,#14598));
#5173=EDGE_LOOP('',(#14599));
#5174=EDGE_LOOP('',(#14600,#14601,#14602,#14603,#14604,#14605,#14606,#14607));
#5175=EDGE_LOOP('',(#14608));
#5176=EDGE_LOOP('',(#14609,#14610,#14611,#14612));
#5177=EDGE_LOOP('',(#14613,#14614,#14615,#14616));
#5178=EDGE_LOOP('',(#14617,#14618));
#5179=EDGE_LOOP('',(#14619,#14620,#14621,#14622));
#5180=EDGE_LOOP('',(#14623,#14624,#14625,#14626));
#5181=EDGE_LOOP('',(#14627,#14628,#14629,#14630));
#5182=EDGE_LOOP('',(#14631,#14632,#14633,#14634));
#5183=EDGE_LOOP('',(#14635,#14636,#14637,#14638));
#5184=EDGE_LOOP('',(#14639,#14640,#14641,#14642));
#5185=EDGE_LOOP('',(#14643,#14644,#14645,#14646,#14647));
#5186=EDGE_LOOP('',(#14648));
#5187=EDGE_LOOP('',(#14649));
#5188=EDGE_LOOP('',(#14650,#14651,#14652,#14653,#14654));
#5189=EDGE_LOOP('',(#14655,#14656,#14657,#14658));
#5190=EDGE_LOOP('',(#14659));
#5191=EDGE_LOOP('',(#14660,#14661,#14662,#14663,#14664,#14665,#14666,#14667,
#14668,#14669,#14670,#14671));
#5192=EDGE_LOOP('',(#14672,#14673,#14674,#14675,#14676,#14677,#14678,#14679,
#14680,#14681,#14682,#14683,#14684));
#5193=EDGE_LOOP('',(#14685,#14686,#14687));
#5194=EDGE_LOOP('',(#14688,#14689,#14690,#14691,#14692,#14693));
#5195=EDGE_LOOP('',(#14694));
#5196=EDGE_LOOP('',(#14695,#14696,#14697,#14698,#14699,#14700,#14701,#14702,
#14703,#14704));
#5197=EDGE_LOOP('',(#14705,#14706,#14707,#14708,#14709));
#5198=EDGE_LOOP('',(#14710,#14711,#14712,#14713));
#5199=EDGE_LOOP('',(#14714,#14715,#14716,#14717,#14718,#14719,#14720,#14721,
#14722,#14723));
#5200=EDGE_LOOP('',(#14724,#14725,#14726,#14727,#14728));
#5201=EDGE_LOOP('',(#14729,#14730,#14731,#14732));
#5202=EDGE_LOOP('',(#14733,#14734,#14735,#14736));
#5203=EDGE_LOOP('',(#14737,#14738,#14739,#14740));
#5204=EDGE_LOOP('',(#14741,#14742,#14743,#14744,#14745,#14746,#14747,#14748,
#14749,#14750,#14751,#14752,#14753,#14754,#14755,#14756,#14757));
#5205=EDGE_LOOP('',(#14758));
#5206=EDGE_LOOP('',(#14759,#14760,#14761,#14762,#14763,#14764,#14765,#14766,
#14767,#14768,#14769,#14770,#14771,#14772,#14773,#14774,#14775));
#5207=EDGE_LOOP('',(#14776));
#5208=EDGE_LOOP('',(#14777,#14778,#14779,#14780));
#5209=EDGE_LOOP('',(#14781,#14782,#14783,#14784));
#5210=EDGE_LOOP('',(#14785,#14786,#14787,#14788));
#5211=EDGE_LOOP('',(#14789,#14790,#14791,#14792));
#5212=EDGE_LOOP('',(#14793,#14794,#14795,#14796));
#5213=EDGE_LOOP('',(#14797,#14798,#14799,#14800));
#5214=EDGE_LOOP('',(#14801,#14802,#14803,#14804));
#5215=EDGE_LOOP('',(#14805,#14806,#14807,#14808));
#5216=EDGE_LOOP('',(#14809,#14810,#14811,#14812));
#5217=EDGE_LOOP('',(#14813,#14814,#14815,#14816));
#5218=EDGE_LOOP('',(#14817,#14818,#14819,#14820));
#5219=EDGE_LOOP('',(#14821,#14822,#14823,#14824));
#5220=EDGE_LOOP('',(#14825,#14826,#14827,#14828));
#5221=EDGE_LOOP('',(#14829,#14830,#14831,#14832));
#5222=EDGE_LOOP('',(#14833,#14834,#14835,#14836));
#5223=EDGE_LOOP('',(#14837,#14838,#14839,#14840,#14841));
#5224=EDGE_LOOP('',(#14842,#14843,#14844,#14845));
#5225=EDGE_LOOP('',(#14846,#14847,#14848,#14849));
#5226=EDGE_LOOP('',(#14850,#14851,#14852,#14853));
#5227=EDGE_LOOP('',(#14854,#14855,#14856,#14857));
#5228=EDGE_LOOP('',(#14858,#14859,#14860,#14861));
#5229=EDGE_LOOP('',(#14862,#14863,#14864,#14865));
#5230=EDGE_LOOP('',(#14866,#14867,#14868,#14869));
#5231=EDGE_LOOP('',(#14870,#14871,#14872,#14873));
#5232=EDGE_LOOP('',(#14874,#14875,#14876,#14877));
#5233=EDGE_LOOP('',(#14878,#14879,#14880,#14881));
#5234=EDGE_LOOP('',(#14882,#14883,#14884,#14885));
#5235=EDGE_LOOP('',(#14886,#14887,#14888,#14889));
#5236=EDGE_LOOP('',(#14890,#14891,#14892,#14893));
#5237=EDGE_LOOP('',(#14894,#14895,#14896,#14897));
#5238=EDGE_LOOP('',(#14898,#14899,#14900,#14901));
#5239=EDGE_LOOP('',(#14902,#14903,#14904,#14905));
#5240=EDGE_LOOP('',(#14906,#14907,#14908,#14909));
#5241=EDGE_LOOP('',(#14910,#14911,#14912,#14913));
#5242=EDGE_LOOP('',(#14914,#14915,#14916,#14917));
#5243=EDGE_LOOP('',(#14918,#14919,#14920,#14921));
#5244=EDGE_LOOP('',(#14922,#14923,#14924,#14925));
#5245=EDGE_LOOP('',(#14926,#14927,#14928,#14929));
#5246=EDGE_LOOP('',(#14930,#14931,#14932,#14933));
#5247=EDGE_LOOP('',(#14934,#14935,#14936,#14937));
#5248=EDGE_LOOP('',(#14938,#14939,#14940,#14941));
#5249=EDGE_LOOP('',(#14942,#14943,#14944,#14945));
#5250=EDGE_LOOP('',(#14946,#14947,#14948,#14949));
#5251=EDGE_LOOP('',(#14950,#14951,#14952,#14953));
#5252=EDGE_LOOP('',(#14954,#14955,#14956,#14957));
#5253=EDGE_LOOP('',(#14958,#14959,#14960,#14961));
#5254=EDGE_LOOP('',(#14962,#14963,#14964,#14965));
#5255=EDGE_LOOP('',(#14966,#14967,#14968,#14969));
#5256=EDGE_LOOP('',(#14970,#14971,#14972,#14973));
#5257=EDGE_LOOP('',(#14974,#14975,#14976,#14977));
#5258=EDGE_LOOP('',(#14978,#14979,#14980,#14981));
#5259=EDGE_LOOP('',(#14982,#14983,#14984,#14985));
#5260=EDGE_LOOP('',(#14986,#14987,#14988,#14989));
#5261=EDGE_LOOP('',(#14990,#14991,#14992,#14993,#14994));
#5262=EDGE_LOOP('',(#14995,#14996,#14997,#14998));
#5263=EDGE_LOOP('',(#14999,#15000,#15001,#15002));
#5264=EDGE_LOOP('',(#15003,#15004,#15005,#15006));
#5265=EDGE_LOOP('',(#15007,#15008,#15009,#15010));
#5266=EDGE_LOOP('',(#15011,#15012,#15013,#15014));
#5267=EDGE_LOOP('',(#15015,#15016,#15017,#15018));
#5268=EDGE_LOOP('',(#15019,#15020,#15021,#15022));
#5269=EDGE_LOOP('',(#15023,#15024,#15025,#15026));
#5270=EDGE_LOOP('',(#15027,#15028,#15029,#15030));
#5271=EDGE_LOOP('',(#15031,#15032,#15033,#15034));
#5272=EDGE_LOOP('',(#15035,#15036,#15037,#15038));
#5273=EDGE_LOOP('',(#15039,#15040,#15041,#15042));
#5274=EDGE_LOOP('',(#15043,#15044,#15045,#15046));
#5275=EDGE_LOOP('',(#15047,#15048,#15049,#15050));
#5276=EDGE_LOOP('',(#15051,#15052,#15053,#15054));
#5277=EDGE_LOOP('',(#15055,#15056,#15057,#15058,#15059,#15060,#15061,#15062,
#15063,#15064,#15065,#15066,#15067,#15068,#15069,#15070,#15071,#15072));
#5278=EDGE_LOOP('',(#15073));
#5279=EDGE_LOOP('',(#15074,#15075,#15076,#15077,#15078,#15079,#15080,#15081,
#15082,#15083,#15084,#15085,#15086,#15087,#15088,#15089,#15090,#15091));
#5280=EDGE_LOOP('',(#15092));
#5281=EDGE_LOOP('',(#15093,#15094,#15095,#15096,#15097));
#5282=EDGE_LOOP('',(#15098,#15099,#15100,#15101));
#5283=EDGE_LOOP('',(#15102,#15103,#15104,#15105));
#5284=EDGE_LOOP('',(#15106,#15107,#15108,#15109));
#5285=EDGE_LOOP('',(#15110,#15111,#15112,#15113));
#5286=EDGE_LOOP('',(#15114,#15115,#15116,#15117));
#5287=EDGE_LOOP('',(#15118,#15119,#15120,#15121));
#5288=EDGE_LOOP('',(#15122,#15123,#15124,#15125));
#5289=EDGE_LOOP('',(#15126,#15127,#15128,#15129));
#5290=EDGE_LOOP('',(#15130,#15131,#15132,#15133));
#5291=EDGE_LOOP('',(#15134,#15135,#15136,#15137));
#5292=EDGE_LOOP('',(#15138,#15139,#15140,#15141));
#5293=EDGE_LOOP('',(#15142,#15143,#15144,#15145));
#5294=EDGE_LOOP('',(#15146,#15147,#15148,#15149));
#5295=EDGE_LOOP('',(#15150,#15151,#15152,#15153));
#5296=EDGE_LOOP('',(#15154,#15155,#15156,#15157));
#5297=EDGE_LOOP('',(#15158,#15159,#15160,#15161));
#5298=EDGE_LOOP('',(#15162,#15163,#15164,#15165));
#5299=EDGE_LOOP('',(#15166,#15167,#15168,#15169));
#5300=EDGE_LOOP('',(#15170,#15171,#15172,#15173));
#5301=EDGE_LOOP('',(#15174,#15175,#15176,#15177));
#5302=EDGE_LOOP('',(#15178,#15179,#15180,#15181));
#5303=EDGE_LOOP('',(#15182,#15183,#15184,#15185));
#5304=EDGE_LOOP('',(#15186,#15187,#15188));
#5305=EDGE_LOOP('',(#15189,#15190,#15191));
#5306=EDGE_LOOP('',(#15192,#15193,#15194,#15195));
#5307=EDGE_LOOP('',(#15196,#15197,#15198,#15199));
#5308=EDGE_LOOP('',(#15200,#15201,#15202,#15203));
#5309=EDGE_LOOP('',(#15204,#15205,#15206,#15207));
#5310=EDGE_LOOP('',(#15208,#15209,#15210,#15211));
#5311=EDGE_LOOP('',(#15212,#15213,#15214,#15215));
#5312=EDGE_LOOP('',(#15216,#15217,#15218,#15219));
#5313=EDGE_LOOP('',(#15220,#15221,#15222,#15223));
#5314=EDGE_LOOP('',(#15224,#15225,#15226,#15227));
#5315=EDGE_LOOP('',(#15228,#15229,#15230,#15231));
#5316=EDGE_LOOP('',(#15232,#15233,#15234,#15235));
#5317=EDGE_LOOP('',(#15236,#15237,#15238,#15239));
#5318=EDGE_LOOP('',(#15240,#15241,#15242,#15243));
#5319=EDGE_LOOP('',(#15244,#15245,#15246,#15247));
#5320=EDGE_LOOP('',(#15248,#15249,#15250,#15251));
#5321=EDGE_LOOP('',(#15252,#15253,#15254,#15255));
#5322=EDGE_LOOP('',(#15256,#15257,#15258,#15259));
#5323=EDGE_LOOP('',(#15260,#15261,#15262,#15263));
#5324=EDGE_LOOP('',(#15264,#15265,#15266,#15267));
#5325=EDGE_LOOP('',(#15268,#15269,#15270,#15271,#15272));
#5326=EDGE_LOOP('',(#15273,#15274,#15275,#15276));
#5327=EDGE_LOOP('',(#15277));
#5328=EDGE_LOOP('',(#15278,#15279,#15280,#15281));
#5329=EDGE_LOOP('',(#15282,#15283,#15284,#15285));
#5330=EDGE_LOOP('',(#15286,#15287,#15288,#15289));
#5331=EDGE_LOOP('',(#15290,#15291,#15292,#15293));
#5332=EDGE_LOOP('',(#15294,#15295,#15296,#15297));
#5333=EDGE_LOOP('',(#15298));
#5334=EDGE_LOOP('',(#15299,#15300,#15301,#15302));
#5335=EDGE_LOOP('',(#15303));
#5336=EDGE_LOOP('',(#15304));
#5337=EDGE_LOOP('',(#15305,#15306,#15307,#15308,#15309));
#5338=EDGE_LOOP('',(#15310));
#5339=EDGE_LOOP('',(#15311));
#5340=EDGE_LOOP('',(#15312,#15313,#15314,#15315));
#5341=EDGE_LOOP('',(#15316,#15317,#15318,#15319));
#5342=EDGE_LOOP('',(#15320,#15321,#15322,#15323,#15324));
#5343=EDGE_LOOP('',(#15325,#15326,#15327,#15328,#15329,#15330,#15331,#15332,
#15333,#15334,#15335,#15336,#15337,#15338,#15339,#15340,#15341,#15342,#15343,
#15344,#15345,#15346,#15347,#15348,#15349));
#5344=EDGE_LOOP('',(#15350));
#5345=EDGE_LOOP('',(#15351));
#5346=EDGE_LOOP('',(#15352,#15353,#15354,#15355,#15356));
#5347=EDGE_LOOP('',(#15357));
#5348=EDGE_LOOP('',(#15358,#15359,#15360,#15361));
#5349=EDGE_LOOP('',(#15362,#15363,#15364,#15365));
#5350=EDGE_LOOP('',(#15366,#15367,#15368,#15369));
#5351=EDGE_LOOP('',(#15370,#15371,#15372,#15373));
#5352=EDGE_LOOP('',(#15374,#15375,#15376,#15377));
#5353=EDGE_LOOP('',(#15378,#15379,#15380,#15381));
#5354=EDGE_LOOP('',(#15382,#15383,#15384,#15385));
#5355=EDGE_LOOP('',(#15386,#15387,#15388,#15389));
#5356=EDGE_LOOP('',(#15390,#15391,#15392,#15393));
#5357=EDGE_LOOP('',(#15394,#15395,#15396,#15397));
#5358=EDGE_LOOP('',(#15398,#15399,#15400,#15401));
#5359=EDGE_LOOP('',(#15402,#15403,#15404,#15405));
#5360=EDGE_LOOP('',(#15406,#15407,#15408,#15409));
#5361=EDGE_LOOP('',(#15410,#15411,#15412,#15413,#15414));
#5362=EDGE_LOOP('',(#15415,#15416,#15417,#15418));
#5363=EDGE_LOOP('',(#15419,#15420,#15421,#15422));
#5364=EDGE_LOOP('',(#15423,#15424,#15425,#15426));
#5365=EDGE_LOOP('',(#15427,#15428,#15429,#15430));
#5366=EDGE_LOOP('',(#15431,#15432,#15433,#15434));
#5367=EDGE_LOOP('',(#15435,#15436,#15437,#15438));
#5368=EDGE_LOOP('',(#15439,#15440,#15441,#15442));
#5369=EDGE_LOOP('',(#15443,#15444,#15445,#15446));
#5370=EDGE_LOOP('',(#15447,#15448,#15449,#15450,#15451,#15452,#15453,#15454,
#15455,#15456,#15457,#15458,#15459,#15460,#15461,#15462,#15463,#15464,#15465,
#15466));
#5371=EDGE_LOOP('',(#15467,#15468,#15469,#15470));
#5372=EDGE_LOOP('',(#15471,#15472,#15473,#15474));
#5373=EDGE_LOOP('',(#15475,#15476,#15477,#15478));
#5374=EDGE_LOOP('',(#15479,#15480));
#5375=EDGE_LOOP('',(#15481));
#5376=EDGE_LOOP('',(#15482));
#5377=EDGE_LOOP('',(#15483));
#5378=EDGE_LOOP('',(#15484));
#5379=EDGE_LOOP('',(#15485,#15486));
#5380=EDGE_LOOP('',(#15487));
#5381=EDGE_LOOP('',(#15488));
#5382=EDGE_LOOP('',(#15489));
#5383=EDGE_LOOP('',(#15490));
#5384=EDGE_LOOP('',(#15491,#15492,#15493,#15494,#15495,#15496));
#5385=EDGE_LOOP('',(#15497,#15498,#15499,#15500,#15501,#15502));
#5386=EDGE_LOOP('',(#15503,#15504,#15505,#15506,#15507,#15508));
#5387=EDGE_LOOP('',(#15509,#15510,#15511,#15512,#15513,#15514));
#5388=EDGE_LOOP('',(#15515,#15516,#15517,#15518));
#5389=EDGE_LOOP('',(#15519,#15520,#15521,#15522));
#5390=EDGE_LOOP('',(#15523,#15524,#15525,#15526,#15527));
#5391=EDGE_LOOP('',(#15528,#15529,#15530,#15531,#15532));
#5392=EDGE_LOOP('',(#15533,#15534,#15535,#15536,#15537));
#5393=EDGE_LOOP('',(#15538,#15539,#15540,#15541,#15542));
#5394=EDGE_LOOP('',(#15543,#15544,#15545,#15546));
#5395=EDGE_LOOP('',(#15547,#15548,#15549,#15550));
#5396=EDGE_LOOP('',(#15551,#15552,#15553,#15554,#15555));
#5397=EDGE_LOOP('',(#15556,#15557,#15558,#15559,#15560));
#5398=EDGE_LOOP('',(#15561,#15562,#15563,#15564,#15565));
#5399=EDGE_LOOP('',(#15566,#15567,#15568,#15569,#15570));
#5400=EDGE_LOOP('',(#15571,#15572,#15573,#15574));
#5401=EDGE_LOOP('',(#15575,#15576,#15577,#15578));
#5402=EDGE_LOOP('',(#15579,#15580,#15581,#15582));
#5403=EDGE_LOOP('',(#15583,#15584,#15585,#15586));
#5404=EDGE_LOOP('',(#15587,#15588,#15589,#15590));
#5405=EDGE_LOOP('',(#15591,#15592,#15593,#15594));
#5406=EDGE_LOOP('',(#15595,#15596,#15597,#15598));
#5407=EDGE_LOOP('',(#15599,#15600,#15601,#15602));
#5408=EDGE_LOOP('',(#15603,#15604,#15605,#15606,#15607,#15608,#15609,#15610,
#15611,#15612));
#5409=EDGE_LOOP('',(#15613));
#5410=EDGE_LOOP('',(#15614,#15615,#15616,#15617,#15618,#15619,#15620,#15621,
#15622,#15623));
#5411=EDGE_LOOP('',(#15624));
#5412=EDGE_LOOP('',(#15625,#15626,#15627,#15628,#15629,#15630));
#5413=EDGE_LOOP('',(#15631,#15632,#15633,#15634));
#5414=EDGE_LOOP('',(#15635,#15636,#15637));
#5415=EDGE_LOOP('',(#15638,#15639,#15640));
#5416=EDGE_LOOP('',(#15641,#15642,#15643,#15644));
#5417=EDGE_LOOP('',(#15645,#15646,#15647,#15648,#15649));
#5418=EDGE_LOOP('',(#15650,#15651,#15652,#15653));
#5419=EDGE_LOOP('',(#15654,#15655,#15656,#15657));
#5420=EDGE_LOOP('',(#15658,#15659,#15660,#15661));
#5421=EDGE_LOOP('',(#15662,#15663,#15664));
#5422=EDGE_LOOP('',(#15665,#15666,#15667,#15668));
#5423=EDGE_LOOP('',(#15669,#15670,#15671,#15672));
#5424=EDGE_LOOP('',(#15673,#15674,#15675));
#5425=EDGE_LOOP('',(#15676,#15677,#15678,#15679,#15680));
#5426=EDGE_LOOP('',(#15681,#15682,#15683,#15684,#15685));
#5427=EDGE_LOOP('',(#15686,#15687,#15688,#15689,#15690));
#5428=EDGE_LOOP('',(#15691,#15692,#15693,#15694));
#5429=EDGE_LOOP('',(#15695,#15696,#15697,#15698));
#5430=EDGE_LOOP('',(#15699,#15700,#15701,#15702));
#5431=EDGE_LOOP('',(#15703,#15704,#15705,#15706,#15707,#15708));
#5432=EDGE_LOOP('',(#15709,#15710,#15711));
#5433=EDGE_LOOP('',(#15712,#15713,#15714,#15715));
#5434=EDGE_LOOP('',(#15716,#15717,#15718,#15719,#15720));
#5435=EDGE_LOOP('',(#15721,#15722,#15723,#15724));
#5436=EDGE_LOOP('',(#15725,#15726,#15727,#15728));
#5437=EDGE_LOOP('',(#15729,#15730,#15731,#15732));
#5438=EDGE_LOOP('',(#15733,#15734,#15735));
#5439=EDGE_LOOP('',(#15736,#15737,#15738));
#5440=EDGE_LOOP('',(#15739,#15740,#15741,#15742));
#5441=EDGE_LOOP('',(#15743,#15744,#15745,#15746,#15747));
#5442=EDGE_LOOP('',(#15748,#15749,#15750,#15751,#15752));
#5443=EDGE_LOOP('',(#15753,#15754,#15755,#15756,#15757,#15758,#15759,#15760,
#15761,#15762));
#5444=EDGE_LOOP('',(#15763,#15764,#15765,#15766,#15767,#15768,#15769,#15770,
#15771,#15772));
#5445=EDGE_LOOP('',(#15773,#15774,#15775,#15776,#15777,#15778,#15779,#15780,
#15781,#15782));
#5446=EDGE_LOOP('',(#15783,#15784,#15785,#15786,#15787,#15788,#15789,#15790,
#15791,#15792));
#5447=EDGE_LOOP('',(#15793,#15794,#15795,#15796,#15797,#15798,#15799,#15800,
#15801,#15802));
#5448=EDGE_LOOP('',(#15803,#15804,#15805,#15806,#15807,#15808));
#5449=EDGE_LOOP('',(#15809,#15810,#15811,#15812));
#5450=EDGE_LOOP('',(#15813,#15814,#15815,#15816));
#5451=EDGE_LOOP('',(#15817,#15818,#15819,#15820));
#5452=EDGE_LOOP('',(#15821,#15822,#15823,#15824,#15825,#15826,#15827,#15828,
#15829,#15830));
#5453=EDGE_LOOP('',(#15831));
#5454=EDGE_LOOP('',(#15832));
#5455=EDGE_LOOP('',(#15833));
#5456=EDGE_LOOP('',(#15834));
#5457=EDGE_LOOP('',(#15835));
#5458=EDGE_LOOP('',(#15836,#15837,#15838,#15839,#15840,#15841));
#5459=EDGE_LOOP('',(#15842,#15843,#15844,#15845));
#5460=EDGE_LOOP('',(#15846,#15847,#15848,#15849,#15850,#15851,#15852,#15853,
#15854,#15855));
#5461=EDGE_LOOP('',(#15856,#15857));
#5462=EDGE_LOOP('',(#15858,#15859));
#5463=EDGE_LOOP('',(#15860,#15861));
#5464=EDGE_LOOP('',(#15862,#15863));
#5465=EDGE_LOOP('',(#15864,#15865));
#5466=EDGE_LOOP('',(#15866,#15867,#15868,#15869));
#5467=EDGE_LOOP('',(#15870,#15871,#15872,#15873));
#5468=EDGE_LOOP('',(#15874,#15875,#15876,#15877));
#5469=EDGE_LOOP('',(#15878,#15879,#15880,#15881));
#5470=EDGE_LOOP('',(#15882,#15883,#15884,#15885));
#5471=EDGE_LOOP('',(#15886,#15887,#15888,#15889,#15890,#15891,#15892,#15893,
#15894,#15895));
#5472=EDGE_LOOP('',(#15896));
#5473=EDGE_LOOP('',(#15897));
#5474=EDGE_LOOP('',(#15898));
#5475=EDGE_LOOP('',(#15899,#15900,#15901,#15902,#15903,#15904,#15905,#15906,
#15907,#15908,#15909,#15910));
#5476=EDGE_LOOP('',(#15911,#15912));
#5477=EDGE_LOOP('',(#15913,#15914,#15915,#15916));
#5478=EDGE_LOOP('',(#15917,#15918,#15919,#15920));
#5479=EDGE_LOOP('',(#15921,#15922));
#5480=EDGE_LOOP('',(#15923,#15924,#15925,#15926,#15927,#15928,#15929,#15930,
#15931,#15932,#15933,#15934));
#5481=EDGE_LOOP('',(#15935));
#5482=EDGE_LOOP('',(#15936));
#5483=EDGE_LOOP('',(#15937,#15938,#15939,#15940,#15941,#15942));
#5484=EDGE_LOOP('',(#15943,#15944,#15945,#15946,#15947,#15948,#15949,#15950,
#15951,#15952));
#5485=EDGE_LOOP('',(#15953,#15954,#15955,#15956,#15957,#15958,#15959,#15960,
#15961,#15962,#15963));
#5486=EDGE_LOOP('',(#15964,#15965,#15966,#15967,#15968,#15969));
#5487=EDGE_LOOP('',(#15970,#15971,#15972,#15973,#15974,#15975));
#5488=EDGE_LOOP('',(#15976,#15977,#15978,#15979,#15980,#15981,#15982));
#5489=EDGE_LOOP('',(#15983,#15984,#15985,#15986,#15987,#15988,#15989,#15990,
#15991));
#5490=EDGE_LOOP('',(#15992,#15993,#15994,#15995,#15996));
#5491=EDGE_LOOP('',(#15997));
#5492=EDGE_LOOP('',(#15998,#15999,#16000,#16001,#16002,#16003,#16004,#16005));
#5493=EDGE_LOOP('',(#16006,#16007,#16008,#16009,#16010,#16011,#16012,#16013));
#5494=EDGE_LOOP('',(#16014,#16015,#16016,#16017,#16018,#16019,#16020,#16021));
#5495=EDGE_LOOP('',(#16022,#16023,#16024,#16025,#16026,#16027,#16028,#16029));
#5496=EDGE_LOOP('',(#16030,#16031,#16032,#16033,#16034,#16035,#16036,#16037));
#5497=EDGE_LOOP('',(#16038,#16039,#16040,#16041));
#5498=EDGE_LOOP('',(#16042,#16043,#16044,#16045));
#5499=EDGE_LOOP('',(#16046,#16047,#16048,#16049));
#5500=EDGE_LOOP('',(#16050,#16051,#16052,#16053,#16054,#16055,#16056,#16057,
#16058,#16059,#16060,#16061));
#5501=EDGE_LOOP('',(#16062));
#5502=EDGE_LOOP('',(#16063));
#5503=EDGE_LOOP('',(#16064));
#5504=EDGE_LOOP('',(#16065,#16066,#16067,#16068));
#5505=EDGE_LOOP('',(#16069,#16070,#16071,#16072));
#5506=EDGE_LOOP('',(#16073,#16074,#16075,#16076));
#5507=EDGE_LOOP('',(#16077,#16078,#16079,#16080,#16081));
#5508=EDGE_LOOP('',(#16082,#16083,#16084,#16085));
#5509=EDGE_LOOP('',(#16086,#16087,#16088,#16089,#16090));
#5510=EDGE_LOOP('',(#16091,#16092,#16093,#16094,#16095,#16096));
#5511=EDGE_LOOP('',(#16097,#16098,#16099,#16100));
#5512=EDGE_LOOP('',(#16101,#16102,#16103,#16104,#16105,#16106));
#5513=EDGE_LOOP('',(#16107,#16108,#16109,#16110,#16111,#16112));
#5514=EDGE_LOOP('',(#16113,#16114,#16115));
#5515=EDGE_LOOP('',(#16116,#16117,#16118,#16119,#16120,#16121,#16122));
#5516=EDGE_LOOP('',(#16123,#16124,#16125));
#5517=EDGE_LOOP('',(#16126,#16127,#16128,#16129,#16130,#16131,#16132));
#5518=EDGE_LOOP('',(#16133,#16134,#16135));
#5519=EDGE_LOOP('',(#16136,#16137,#16138));
#5520=EDGE_LOOP('',(#16139,#16140,#16141,#16142,#16143,#16144));
#5521=EDGE_LOOP('',(#16145,#16146,#16147,#16148));
#5522=EDGE_LOOP('',(#16149,#16150,#16151,#16152));
#5523=EDGE_LOOP('',(#16153,#16154,#16155,#16156));
#5524=EDGE_LOOP('',(#16157,#16158,#16159,#16160));
#5525=EDGE_LOOP('',(#16161,#16162,#16163,#16164));
#5526=EDGE_LOOP('',(#16165,#16166,#16167,#16168,#16169));
#5527=EDGE_LOOP('',(#16170,#16171,#16172,#16173));
#5528=EDGE_LOOP('',(#16174,#16175,#16176,#16177));
#5529=EDGE_LOOP('',(#16178,#16179,#16180,#16181));
#5530=EDGE_LOOP('',(#16182,#16183,#16184,#16185));
#5531=EDGE_LOOP('',(#16186,#16187,#16188,#16189));
#5532=EDGE_LOOP('',(#16190,#16191,#16192,#16193,#16194));
#5533=EDGE_LOOP('',(#16195,#16196,#16197,#16198,#16199));
#5534=EDGE_LOOP('',(#16200,#16201,#16202,#16203));
#5535=EDGE_LOOP('',(#16204,#16205,#16206,#16207));
#5536=EDGE_LOOP('',(#16208,#16209,#16210,#16211));
#5537=EDGE_LOOP('',(#16212,#16213,#16214,#16215));
#5538=EDGE_LOOP('',(#16216,#16217,#16218,#16219));
#5539=EDGE_LOOP('',(#16220,#16221,#16222,#16223));
#5540=EDGE_LOOP('',(#16224,#16225,#16226,#16227,#16228));
#5541=EDGE_LOOP('',(#16229,#16230,#16231,#16232,#16233,#16234,#16235));
#5542=EDGE_LOOP('',(#16236,#16237,#16238,#16239));
#5543=EDGE_LOOP('',(#16240,#16241,#16242,#16243));
#5544=EDGE_LOOP('',(#16244,#16245,#16246,#16247));
#5545=EDGE_LOOP('',(#16248,#16249,#16250,#16251));
#5546=EDGE_LOOP('',(#16252,#16253,#16254,#16255));
#5547=EDGE_LOOP('',(#16256,#16257,#16258,#16259));
#5548=EDGE_LOOP('',(#16260,#16261,#16262));
#5549=EDGE_LOOP('',(#16263,#16264,#16265,#16266));
#5550=EDGE_LOOP('',(#16267,#16268,#16269,#16270,#16271,#16272,#16273));
#5551=EDGE_LOOP('',(#16274,#16275,#16276,#16277));
#5552=EDGE_LOOP('',(#16278,#16279,#16280,#16281));
#5553=EDGE_LOOP('',(#16282,#16283,#16284,#16285));
#5554=EDGE_LOOP('',(#16286,#16287,#16288,#16289));
#5555=EDGE_LOOP('',(#16290,#16291,#16292,#16293));
#5556=EDGE_LOOP('',(#16294,#16295,#16296,#16297));
#5557=EDGE_LOOP('',(#16298,#16299,#16300,#16301));
#5558=EDGE_LOOP('',(#16302,#16303,#16304,#16305,#16306));
#5559=EDGE_LOOP('',(#16307,#16308,#16309,#16310));
#5560=EDGE_LOOP('',(#16311,#16312,#16313,#16314));
#5561=EDGE_LOOP('',(#16315,#16316,#16317,#16318));
#5562=EDGE_LOOP('',(#16319,#16320,#16321));
#5563=EDGE_LOOP('',(#16322,#16323,#16324,#16325));
#5564=EDGE_LOOP('',(#16326,#16327,#16328,#16329,#16330,#16331));
#5565=EDGE_LOOP('',(#16332,#16333,#16334,#16335,#16336));
#5566=EDGE_LOOP('',(#16337,#16338,#16339,#16340));
#5567=EDGE_LOOP('',(#16341,#16342,#16343,#16344,#16345));
#5568=EDGE_LOOP('',(#16346,#16347,#16348,#16349,#16350));
#5569=EDGE_LOOP('',(#16351,#16352,#16353,#16354));
#5570=EDGE_LOOP('',(#16355,#16356,#16357,#16358));
#5571=EDGE_LOOP('',(#16359,#16360,#16361,#16362));
#5572=EDGE_LOOP('',(#16363,#16364,#16365,#16366,#16367));
#5573=EDGE_LOOP('',(#16368,#16369,#16370,#16371));
#5574=EDGE_LOOP('',(#16372,#16373,#16374,#16375));
#5575=EDGE_LOOP('',(#16376,#16377,#16378,#16379));
#5576=EDGE_LOOP('',(#16380,#16381,#16382,#16383,#16384));
#5577=EDGE_LOOP('',(#16385,#16386,#16387,#16388));
#5578=EDGE_LOOP('',(#16389,#16390,#16391,#16392));
#5579=EDGE_LOOP('',(#16393,#16394,#16395,#16396));
#5580=EDGE_LOOP('',(#16397,#16398,#16399,#16400,#16401));
#5581=EDGE_LOOP('',(#16402,#16403,#16404,#16405));
#5582=EDGE_LOOP('',(#16406,#16407,#16408));
#5583=EDGE_LOOP('',(#16409,#16410,#16411,#16412));
#5584=EDGE_LOOP('',(#16413,#16414,#16415));
#5585=EDGE_LOOP('',(#16416,#16417,#16418));
#5586=EDGE_LOOP('',(#16419,#16420,#16421,#16422));
#5587=EDGE_LOOP('',(#16423,#16424,#16425,#16426));
#5588=EDGE_LOOP('',(#16427,#16428,#16429,#16430));
#5589=EDGE_LOOP('',(#16431,#16432,#16433,#16434));
#5590=EDGE_LOOP('',(#16435,#16436,#16437,#16438,#16439));
#5591=EDGE_LOOP('',(#16440,#16441,#16442,#16443));
#5592=EDGE_LOOP('',(#16444,#16445,#16446,#16447));
#5593=EDGE_LOOP('',(#16448,#16449,#16450,#16451));
#5594=EDGE_LOOP('',(#16452,#16453,#16454,#16455));
#5595=EDGE_LOOP('',(#16456,#16457,#16458,#16459));
#5596=EDGE_LOOP('',(#16460,#16461,#16462));
#5597=EDGE_LOOP('',(#16463,#16464,#16465,#16466));
#5598=EDGE_LOOP('',(#16467,#16468,#16469,#16470));
#5599=EDGE_LOOP('',(#16471,#16472,#16473,#16474));
#5600=EDGE_LOOP('',(#16475,#16476,#16477,#16478));
#5601=EDGE_LOOP('',(#16479,#16480,#16481,#16482));
#5602=EDGE_LOOP('',(#16483,#16484,#16485,#16486));
#5603=EDGE_LOOP('',(#16487,#16488,#16489));
#5604=EDGE_LOOP('',(#16490,#16491,#16492));
#5605=EDGE_LOOP('',(#16493,#16494,#16495,#16496));
#5606=EDGE_LOOP('',(#16497,#16498,#16499,#16500));
#5607=EDGE_LOOP('',(#16501,#16502,#16503,#16504));
#5608=EDGE_LOOP('',(#16505,#16506,#16507,#16508));
#5609=EDGE_LOOP('',(#16509,#16510,#16511,#16512));
#5610=EDGE_LOOP('',(#16513,#16514,#16515,#16516));
#5611=EDGE_LOOP('',(#16517,#16518,#16519,#16520));
#5612=EDGE_LOOP('',(#16521,#16522,#16523));
#5613=EDGE_LOOP('',(#16524,#16525,#16526,#16527));
#5614=EDGE_LOOP('',(#16528,#16529,#16530,#16531));
#5615=EDGE_LOOP('',(#16532,#16533,#16534,#16535));
#5616=EDGE_LOOP('',(#16536,#16537,#16538,#16539));
#5617=EDGE_LOOP('',(#16540,#16541,#16542,#16543,#16544));
#5618=EDGE_LOOP('',(#16545,#16546,#16547));
#5619=EDGE_LOOP('',(#16548));
#5620=EDGE_LOOP('',(#16549,#16550,#16551,#16552));
#5621=EDGE_LOOP('',(#16553));
#5622=EDGE_LOOP('',(#16554));
#5623=CIRCLE('',#17838,0.0046);
#5624=CIRCLE('',#17839,0.010874);
#5625=CIRCLE('',#17840,0.0046);
#5626=CIRCLE('',#17841,0.012);
#5627=CIRCLE('',#17842,0.0046);
#5628=CIRCLE('',#17843,0.010874);
#5629=CIRCLE('',#17844,0.0046);
#5630=CIRCLE('',#17845,0.012);
#5631=CIRCLE('',#17846,0.0046);
#5632=CIRCLE('',#17847,0.010874);
#5633=CIRCLE('',#17848,0.0046);
#5634=CIRCLE('',#17849,0.012);
#5635=CIRCLE('',#17850,0.0046);
#5636=CIRCLE('',#17851,0.010874);
#5637=CIRCLE('',#17852,0.0046);
#5638=CIRCLE('',#17853,0.012);
#5639=CIRCLE('',#17854,0.0046);
#5640=CIRCLE('',#17855,0.010874);
#5641=CIRCLE('',#17856,0.0046);
#5642=CIRCLE('',#17857,0.012);
#5643=CIRCLE('',#17858,0.0046);
#5644=CIRCLE('',#17859,0.010874);
#5645=CIRCLE('',#17860,0.0046);
#5646=CIRCLE('',#17861,0.012);
#5647=CIRCLE('',#17862,0.0046);
#5648=CIRCLE('',#17863,0.010874);
#5649=CIRCLE('',#17864,0.0046);
#5650=CIRCLE('',#17865,0.012);
#5651=CIRCLE('',#17866,0.0046);
#5652=CIRCLE('',#17867,0.010874);
#5653=CIRCLE('',#17868,0.0046);
#5654=CIRCLE('',#17869,0.012);
#5655=CIRCLE('',#17870,0.0046);
#5656=CIRCLE('',#17871,0.010874);
#5657=CIRCLE('',#17872,0.0046);
#5658=CIRCLE('',#17873,0.012);
#5659=CIRCLE('',#17874,0.0046);
#5660=CIRCLE('',#17875,0.010874);
#5661=CIRCLE('',#17876,0.0046);
#5662=CIRCLE('',#17877,0.012);
#5663=CIRCLE('',#17878,0.0046);
#5664=CIRCLE('',#17879,0.010874);
#5665=CIRCLE('',#17880,0.0046);
#5666=CIRCLE('',#17881,0.012);
#5667=CIRCLE('',#17882,0.0046);
#5668=CIRCLE('',#17883,0.010874);
#5669=CIRCLE('',#17884,0.0046);
#5670=CIRCLE('',#17885,0.012);
#5671=CIRCLE('',#17886,0.0046);
#5672=CIRCLE('',#17887,0.010874);
#5673=CIRCLE('',#17888,0.0046);
#5674=CIRCLE('',#17889,0.012);
#5675=CIRCLE('',#17890,0.0046);
#5676=CIRCLE('',#17891,0.010874);
#5677=CIRCLE('',#17892,0.0046);
#5678=CIRCLE('',#17893,0.012);
#5679=CIRCLE('',#17894,0.0046);
#5680=CIRCLE('',#17895,0.010874);
#5681=CIRCLE('',#17896,0.0046);
#5682=CIRCLE('',#17897,0.012);
#5683=CIRCLE('',#17898,0.0046);
#5684=CIRCLE('',#17899,0.010874);
#5685=CIRCLE('',#17900,0.0046);
#5686=CIRCLE('',#17901,0.012);
#5687=CIRCLE('',#17902,0.0046);
#5688=CIRCLE('',#17903,0.010874);
#5689=CIRCLE('',#17904,0.0046);
#5690=CIRCLE('',#17905,0.012);
#5691=CIRCLE('',#17906,0.0046);
#5692=CIRCLE('',#17907,0.010874);
#5693=CIRCLE('',#17908,0.0046);
#5694=CIRCLE('',#17909,0.012);
#5695=CIRCLE('',#17910,0.0046);
#5696=CIRCLE('',#17911,0.010874);
#5697=CIRCLE('',#17912,0.0046);
#5698=CIRCLE('',#17913,0.012);
#5699=CIRCLE('',#17914,0.0046);
#5700=CIRCLE('',#17915,0.010874);
#5701=CIRCLE('',#17916,0.0046);
#5702=CIRCLE('',#17917,0.012);
#5703=CIRCLE('',#17918,0.0046);
#5704=CIRCLE('',#17919,0.010874);
#5705=CIRCLE('',#17920,0.0046);
#5706=CIRCLE('',#17921,0.012);
#5707=CIRCLE('',#17922,0.0046);
#5708=CIRCLE('',#17923,0.010874);
#5709=CIRCLE('',#17924,0.0046);
#5710=CIRCLE('',#17925,0.012);
#5711=CIRCLE('',#17926,0.0046);
#5712=CIRCLE('',#17927,0.010874);
#5713=CIRCLE('',#17928,0.0046);
#5714=CIRCLE('',#17929,0.012);
#5715=CIRCLE('',#17930,0.0046);
#5716=CIRCLE('',#17931,0.010874);
#5717=CIRCLE('',#17932,0.0046);
#5718=CIRCLE('',#17933,0.012);
#5719=CIRCLE('',#17934,0.0046);
#5720=CIRCLE('',#17935,0.010874);
#5721=CIRCLE('',#17936,0.0046);
#5722=CIRCLE('',#17937,0.012);
#5723=CIRCLE('',#17938,0.0046);
#5724=CIRCLE('',#17939,0.010874);
#5725=CIRCLE('',#17940,0.0046);
#5726=CIRCLE('',#17941,0.012);
#5727=CIRCLE('',#17942,0.0046);
#5728=CIRCLE('',#17943,0.010874);
#5729=CIRCLE('',#17944,0.0046);
#5730=CIRCLE('',#17945,0.012);
#5731=CIRCLE('',#17946,0.0046);
#5732=CIRCLE('',#17947,0.010874);
#5733=CIRCLE('',#17948,0.0046);
#5734=CIRCLE('',#17949,0.012);
#5735=CIRCLE('',#17950,0.0046);
#5736=CIRCLE('',#17951,0.010874);
#5737=CIRCLE('',#17952,0.0046);
#5738=CIRCLE('',#17953,0.012);
#5739=CIRCLE('',#17954,0.0046);
#5740=CIRCLE('',#17955,0.010874);
#5741=CIRCLE('',#17956,0.0046);
#5742=CIRCLE('',#17957,0.012);
#5743=CIRCLE('',#17958,0.0046);
#5744=CIRCLE('',#17959,0.010874);
#5745=CIRCLE('',#17960,0.0046);
#5746=CIRCLE('',#17961,0.012);
#5747=CIRCLE('',#17962,0.0046);
#5748=CIRCLE('',#17963,0.010874);
#5749=CIRCLE('',#17964,0.0046);
#5750=CIRCLE('',#17965,0.012);
#5751=CIRCLE('',#17966,0.0046);
#5752=CIRCLE('',#17967,0.010874);
#5753=CIRCLE('',#17968,0.0046);
#5754=CIRCLE('',#17969,0.012);
#5755=CIRCLE('',#17970,0.0046);
#5756=CIRCLE('',#17971,0.010874);
#5757=CIRCLE('',#17972,0.0046);
#5758=CIRCLE('',#17973,0.012);
#5759=CIRCLE('',#17974,0.0046);
#5760=CIRCLE('',#17975,0.010874);
#5761=CIRCLE('',#17976,0.0046);
#5762=CIRCLE('',#17977,0.012);
#5763=CIRCLE('',#17978,0.0046);
#5764=CIRCLE('',#17979,0.010874);
#5765=CIRCLE('',#17980,0.0046);
#5766=CIRCLE('',#17981,0.012);
#5767=CIRCLE('',#17982,0.0046);
#5768=CIRCLE('',#17983,0.010874);
#5769=CIRCLE('',#17984,0.0046);
#5770=CIRCLE('',#17985,0.012);
#5771=CIRCLE('',#17986,0.0046);
#5772=CIRCLE('',#17987,0.010874);
#5773=CIRCLE('',#17988,0.0046);
#5774=CIRCLE('',#17989,0.012);
#5775=CIRCLE('',#17990,0.0046);
#5776=CIRCLE('',#17991,0.010874);
#5777=CIRCLE('',#17992,0.0046);
#5778=CIRCLE('',#17993,0.012);
#5779=CIRCLE('',#17994,0.0046);
#5780=CIRCLE('',#17995,0.010874);
#5781=CIRCLE('',#17996,0.0046);
#5782=CIRCLE('',#17997,0.012);
#5783=CIRCLE('',#17998,0.0046);
#5784=CIRCLE('',#17999,0.010874);
#5785=CIRCLE('',#18000,0.0046);
#5786=CIRCLE('',#18001,0.012);
#5787=CIRCLE('',#18002,0.0046);
#5788=CIRCLE('',#18003,0.010874);
#5789=CIRCLE('',#18004,0.0046);
#5790=CIRCLE('',#18005,0.012);
#5791=CIRCLE('',#18006,0.0046);
#5792=CIRCLE('',#18007,0.010874);
#5793=CIRCLE('',#18008,0.0046);
#5794=CIRCLE('',#18009,0.012);
#5795=CIRCLE('',#18010,0.0046);
#5796=CIRCLE('',#18011,0.010874);
#5797=CIRCLE('',#18012,0.0046);
#5798=CIRCLE('',#18013,0.012);
#5799=CIRCLE('',#18014,0.0046);
#5800=CIRCLE('',#18015,0.010874);
#5801=CIRCLE('',#18016,0.0046);
#5802=CIRCLE('',#18017,0.012);
#5803=CIRCLE('',#18018,0.0046);
#5804=CIRCLE('',#18019,0.010874);
#5805=CIRCLE('',#18020,0.0046);
#5806=CIRCLE('',#18021,0.012);
#5807=CIRCLE('',#18022,0.009);
#5808=CIRCLE('',#18024,0.012);
#5809=CIRCLE('',#18026,0.012);
#5810=CIRCLE('',#18028,0.012);
#5811=CIRCLE('',#18030,0.012);
#5812=CIRCLE('',#18032,0.012);
#5813=CIRCLE('',#18034,0.012);
#5814=CIRCLE('',#18036,0.012);
#5815=CIRCLE('',#18038,0.012);
#5816=CIRCLE('',#18040,0.012);
#5817=CIRCLE('',#18042,0.012);
#5818=CIRCLE('',#18044,0.012);
#5819=CIRCLE('',#18046,0.012);
#5820=CIRCLE('',#18048,0.012);
#5821=CIRCLE('',#18050,0.012);
#5822=CIRCLE('',#18052,0.012);
#5823=CIRCLE('',#18054,0.012);
#5824=CIRCLE('',#18056,0.012);
#5825=CIRCLE('',#18058,0.012);
#5826=CIRCLE('',#18060,0.012);
#5827=CIRCLE('',#18062,0.012);
#5828=CIRCLE('',#18064,0.012);
#5829=CIRCLE('',#18066,0.012);
#5830=CIRCLE('',#18068,0.012);
#5831=CIRCLE('',#18070,0.012);
#5832=CIRCLE('',#18072,0.012);
#5833=CIRCLE('',#18074,0.012);
#5834=CIRCLE('',#18076,0.012);
#5835=CIRCLE('',#18078,0.012);
#5836=CIRCLE('',#18080,0.012);
#5837=CIRCLE('',#18082,0.012);
#5838=CIRCLE('',#18084,0.012);
#5839=CIRCLE('',#18086,0.012);
#5840=CIRCLE('',#18088,0.012);
#5841=CIRCLE('',#18090,0.012);
#5842=CIRCLE('',#18092,0.012);
#5843=CIRCLE('',#18094,0.012);
#5844=CIRCLE('',#18096,0.012);
#5845=CIRCLE('',#18098,0.012);
#5846=CIRCLE('',#18100,0.012);
#5847=CIRCLE('',#18102,0.012);
#5848=CIRCLE('',#18104,0.012);
#5849=CIRCLE('',#18106,0.012);
#5850=CIRCLE('',#18108,0.012);
#5851=CIRCLE('',#18110,0.012);
#5852=CIRCLE('',#18112,0.012);
#5853=CIRCLE('',#18114,0.0046);
#5854=CIRCLE('',#18115,0.0046);
#5855=CIRCLE('',#18116,0.010874);
#5856=CIRCLE('',#18117,0.0046);
#5857=CIRCLE('',#18118,0.0046);
#5858=CIRCLE('',#18119,0.010874);
#5859=CIRCLE('',#18120,0.0046);
#5860=CIRCLE('',#18121,0.0046);
#5861=CIRCLE('',#18122,0.010874);
#5862=CIRCLE('',#18123,0.0046);
#5863=CIRCLE('',#18124,0.0046);
#5864=CIRCLE('',#18125,0.010874);
#5865=CIRCLE('',#18126,0.0046);
#5866=CIRCLE('',#18127,0.0046);
#5867=CIRCLE('',#18128,0.010874);
#5868=CIRCLE('',#18129,0.0046);
#5869=CIRCLE('',#18130,0.0046);
#5870=CIRCLE('',#18131,0.010874);
#5871=CIRCLE('',#18132,0.0046);
#5872=CIRCLE('',#18133,0.0046);
#5873=CIRCLE('',#18134,0.010874);
#5874=CIRCLE('',#18135,0.0046);
#5875=CIRCLE('',#18136,0.0046);
#5876=CIRCLE('',#18137,0.010874);
#5877=CIRCLE('',#18138,0.0046);
#5878=CIRCLE('',#18139,0.0046);
#5879=CIRCLE('',#18140,0.010874);
#5880=CIRCLE('',#18141,0.0046);
#5881=CIRCLE('',#18142,0.0046);
#5882=CIRCLE('',#18143,0.010874);
#5883=CIRCLE('',#18144,0.0046);
#5884=CIRCLE('',#18145,0.0046);
#5885=CIRCLE('',#18146,0.010874);
#5886=CIRCLE('',#18147,0.0046);
#5887=CIRCLE('',#18148,0.012);
#5888=CIRCLE('',#18149,0.0046);
#5889=CIRCLE('',#18150,0.010874);
#5890=CIRCLE('',#18151,0.0046);
#5891=CIRCLE('',#18152,0.0046);
#5892=CIRCLE('',#18153,0.010874);
#5893=CIRCLE('',#18154,0.0046);
#5894=CIRCLE('',#18155,0.0046);
#5895=CIRCLE('',#18156,0.010874);
#5896=CIRCLE('',#18157,0.0046);
#5897=CIRCLE('',#18158,0.0046);
#5898=CIRCLE('',#18159,0.010874);
#5899=CIRCLE('',#18160,0.0046);
#5900=CIRCLE('',#18161,0.0046);
#5901=CIRCLE('',#18162,0.010874);
#5902=CIRCLE('',#18163,0.0046);
#5903=CIRCLE('',#18164,0.0046);
#5904=CIRCLE('',#18165,0.010874);
#5905=CIRCLE('',#18166,0.0046);
#5906=CIRCLE('',#18167,0.0046);
#5907=CIRCLE('',#18168,0.010874);
#5908=CIRCLE('',#18169,0.0046);
#5909=CIRCLE('',#18170,0.0046);
#5910=CIRCLE('',#18171,0.010874);
#5911=CIRCLE('',#18172,0.0046);
#5912=CIRCLE('',#18173,0.0046);
#5913=CIRCLE('',#18174,0.010874);
#5914=CIRCLE('',#18175,0.0046);
#5915=CIRCLE('',#18176,0.0046);
#5916=CIRCLE('',#18177,0.010874);
#5917=CIRCLE('',#18178,0.0046);
#5918=CIRCLE('',#18179,0.0046);
#5919=CIRCLE('',#18180,0.010874);
#5920=CIRCLE('',#18181,0.0046);
#5921=CIRCLE('',#18182,0.0046);
#5922=CIRCLE('',#18183,0.010874);
#5923=CIRCLE('',#18184,0.0046);
#5924=CIRCLE('',#18185,0.0046);
#5925=CIRCLE('',#18186,0.010874);
#5926=CIRCLE('',#18187,0.0046);
#5927=CIRCLE('',#18188,0.0046);
#5928=CIRCLE('',#18189,0.010874);
#5929=CIRCLE('',#18190,0.0046);
#5930=CIRCLE('',#18191,0.0046);
#5931=CIRCLE('',#18192,0.010874);
#5932=CIRCLE('',#18193,0.0046);
#5933=CIRCLE('',#18194,0.0046);
#5934=CIRCLE('',#18195,0.010874);
#5935=CIRCLE('',#18196,0.0046);
#5936=CIRCLE('',#18197,0.0046);
#5937=CIRCLE('',#18198,0.010874);
#5938=CIRCLE('',#18199,0.0046);
#5939=CIRCLE('',#18200,0.0046);
#5940=CIRCLE('',#18201,0.010874);
#5941=CIRCLE('',#18202,0.0046);
#5942=CIRCLE('',#18203,0.0046);
#5943=CIRCLE('',#18204,0.010874);
#5944=CIRCLE('',#18205,0.0046);
#5945=CIRCLE('',#18206,0.0046);
#5946=CIRCLE('',#18207,0.010874);
#5947=CIRCLE('',#18208,0.0046);
#5948=CIRCLE('',#18209,0.0046);
#5949=CIRCLE('',#18210,0.010874);
#5950=CIRCLE('',#18211,0.0046);
#5951=CIRCLE('',#18212,0.0046);
#5952=CIRCLE('',#18213,0.010874);
#5953=CIRCLE('',#18214,0.0046);
#5954=CIRCLE('',#18215,0.0046);
#5955=CIRCLE('',#18216,0.010874);
#5956=CIRCLE('',#18217,0.0046);
#5957=CIRCLE('',#18218,0.0046);
#5958=CIRCLE('',#18219,0.010874);
#5959=CIRCLE('',#18220,0.0046);
#5960=CIRCLE('',#18221,0.0046);
#5961=CIRCLE('',#18222,0.010874);
#5962=CIRCLE('',#18223,0.0046);
#5963=CIRCLE('',#18224,0.0046);
#5964=CIRCLE('',#18225,0.010874);
#5965=CIRCLE('',#18226,0.0046);
#5966=CIRCLE('',#18227,0.0046);
#5967=CIRCLE('',#18228,0.010874);
#5968=CIRCLE('',#18229,0.0046);
#5969=CIRCLE('',#18230,0.0046);
#5970=CIRCLE('',#18231,0.010874);
#5971=CIRCLE('',#18232,0.0046);
#5972=CIRCLE('',#18233,0.0046);
#5973=CIRCLE('',#18234,0.010874);
#5974=CIRCLE('',#18235,0.0046);
#5975=CIRCLE('',#18236,0.0046);
#5976=CIRCLE('',#18237,0.010874);
#5977=CIRCLE('',#18238,0.0046);
#5978=CIRCLE('',#18239,0.0046);
#5979=CIRCLE('',#18240,0.010874);
#5980=CIRCLE('',#18241,0.0046);
#5981=CIRCLE('',#18242,0.0046);
#5982=CIRCLE('',#18243,0.010874);
#5983=CIRCLE('',#18244,0.0046);
#5984=CIRCLE('',#18245,0.0046);
#5985=CIRCLE('',#18246,0.010874);
#5986=CIRCLE('',#18247,0.0046);
#5987=CIRCLE('',#18248,0.0046);
#5988=CIRCLE('',#18249,0.010874);
#5989=CIRCLE('',#18250,0.0046);
#5990=CIRCLE('',#18251,0.0046);
#5991=CIRCLE('',#18252,0.010874);
#5992=CIRCLE('',#18253,0.009);
#5993=CIRCLE('',#18396,0.005);
#5994=CIRCLE('',#18397,0.005);
#5995=CIRCLE('',#18398,0.005);
#5996=CIRCLE('',#18399,0.005);
#5997=CIRCLE('',#18401,0.0074756477610481);
#5998=CIRCLE('',#18402,0.0074756477610481);
#5999=CIRCLE('',#18403,0.0074756477610481);
#6000=CIRCLE('',#18405,0.00932888901198444);
#6001=CIRCLE('',#18406,0.00932888901198444);
#6002=CIRCLE('',#18407,0.00932888901198444);
#6003=CIRCLE('',#18408,0.00932888901198444);
#6004=CIRCLE('',#18410,0.00932888901198444);
#6005=CIRCLE('',#18411,0.00932888901198444);
#6006=CIRCLE('',#18412,0.00932888901198444);
#6007=CIRCLE('',#18414,0.00882888901198444);
#6008=CIRCLE('',#18415,0.0055);
#6009=CIRCLE('',#18417,0.00882888901198444);
#6010=CIRCLE('',#18419,0.00898940279602035);
#6011=CIRCLE('',#18420,0.00898940279602035);
#6012=CIRCLE('',#18421,0.00898940279602035);
#6013=CIRCLE('',#18423,0.00912888901198444);
#6014=CIRCLE('',#18424,0.00912888901198444);
#6015=CIRCLE('',#18425,0.00912888901198444);
#6016=CIRCLE('',#18427,0.00932888901198444);
#6017=CIRCLE('',#18428,0.00932888901198444);
#6018=CIRCLE('',#18429,0.00932888901198444);
#6019=CIRCLE('',#18431,0.00932888901198444);
#6020=CIRCLE('',#18432,0.00932888901198444);
#6021=CIRCLE('',#18433,0.00932888901198444);
#6022=CIRCLE('',#18435,0.00898940279602035);
#6023=CIRCLE('',#18436,0.00898940279602035);
#6024=CIRCLE('',#18437,0.00898940279602035);
#6025=CIRCLE('',#18439,0.00912888901198443);
#6026=CIRCLE('',#18440,0.00912888901198443);
#6027=CIRCLE('',#18441,0.00912888901198443);
#6028=CIRCLE('',#18443,0.00932888901198444);
#6029=CIRCLE('',#18444,0.00932888901198444);
#6030=CIRCLE('',#18445,0.00932888901198444);
#6031=CIRCLE('',#18447,0.0091288890119844);
#6032=CIRCLE('',#18448,0.0091288890119844);
#6033=CIRCLE('',#18449,0.0091288890119844);
#6034=CIRCLE('',#18451,0.00932888901198444);
#6035=CIRCLE('',#18452,0.00932888901198444);
#6036=CIRCLE('',#18453,0.00932888901198444);
#6037=CIRCLE('',#18455,0.00912888901198441);
#6038=CIRCLE('',#18456,0.00912888901198441);
#6039=CIRCLE('',#18457,0.00912888901198441);
#6040=CIRCLE('',#18459,0.00932888901198444);
#6041=CIRCLE('',#18460,0.00932888901198444);
#6042=CIRCLE('',#18461,0.00932888901198444);
#6043=CIRCLE('',#18463,0.00912888901198442);
#6044=CIRCLE('',#18464,0.00912888901198442);
#6045=CIRCLE('',#18465,0.00912888901198442);
#6046=CIRCLE('',#18467,0.00932888901198444);
#6047=CIRCLE('',#18468,0.00932888901198444);
#6048=CIRCLE('',#18469,0.00932888901198444);
#6049=CIRCLE('',#18471,0.0079756477610481);
#6050=CIRCLE('',#18473,0.0045);
#6051=CIRCLE('',#18480,0.0005);
#6052=CIRCLE('',#18482,0.0005);
#6053=CIRCLE('',#18484,0.0005);
#6054=CIRCLE('',#18486,0.0005);
#6055=CIRCLE('',#18488,0.0005);
#6056=CIRCLE('',#18490,0.0005);
#6057=CIRCLE('',#18492,0.0005);
#6058=CIRCLE('',#18494,0.0005);
#6059=CIRCLE('',#18496,0.0005);
#6060=CIRCLE('',#18498,0.0005);
#6061=CIRCLE('',#18500,0.0005);
#6062=CIRCLE('',#18502,0.0005);
#6063=CIRCLE('',#18504,0.0005);
#6064=CIRCLE('',#18506,0.0005);
#6065=CIRCLE('',#18508,0.0005);
#6066=CIRCLE('',#18510,0.0005);
#6067=CIRCLE('',#18512,0.0005);
#6068=CIRCLE('',#18514,0.0005);
#6069=CIRCLE('',#18516,0.0005);
#6070=CIRCLE('',#18519,0.0012);
#6071=CIRCLE('',#18521,0.00407884422956621);
#6072=CIRCLE('',#18522,0.00926353205762594);
#6073=CIRCLE('',#18523,0.00911324794481585);
#6074=CIRCLE('',#18524,0.00911756273482394);
#6075=CIRCLE('',#18526,0.00925178497204344);
#6076=CIRCLE('',#18527,0.00913306539255981);
#6077=CIRCLE('',#18528,0.00926684648530518);
#6078=CIRCLE('',#18529,0.0092508836596066);
#6079=CIRCLE('',#18532,0.00806904972011834);
#6080=CIRCLE('',#18534,0.00806904972011834);
#6081=CIRCLE('',#18537,0.00806904972011834);
#6082=CIRCLE('',#18539,0.00407884422956621);
#6083=CIRCLE('',#18540,0.00407884422999999);
#6084=CIRCLE('',#18541,0.00921926258718324);
#6085=CIRCLE('',#18542,0.00921925444913531);
#6086=CIRCLE('',#18553,0.00816904972011834);
#6087=CIRCLE('',#18556,0.00816904972011834);
#6088=CIRCLE('',#18558,0.00816904972011834);
#6089=CIRCLE('',#18559,9.9999992588795E-5);
#6090=CIRCLE('',#18560,9.99999925874768E-5);
#6091=CIRCLE('',#18563,0.000104492701428376);
#6092=CIRCLE('',#18564,0.0001);
#6093=CIRCLE('',#18567,0.0001);
#6094=CIRCLE('',#18568,0.0001);
#6095=CIRCLE('',#18570,0.000104493909288024);
#6096=CIRCLE('',#18571,9.99999925875666E-5);
#6097=CIRCLE('',#18573,0.000104492715876204);
#6098=CIRCLE('',#18574,9.99999925888095E-5);
#6099=CIRCLE('',#18578,0.0001);
#6100=CIRCLE('',#18580,0.0001);
#6101=CIRCLE('',#18582,9.99999969896661E-5);
#6102=CIRCLE('',#18583,9.99999999999991E-5);
#6103=CIRCLE('',#18584,0.000100000000000023);
#6104=CIRCLE('',#18586,9.99782235912355E-5);
#6105=CIRCLE('',#18587,0.0001);
#6106=CIRCLE('',#18590,0.0001);
#6107=CIRCLE('',#18593,0.0001);
#6108=CIRCLE('',#18595,0.0001);
#6109=CIRCLE('',#18597,0.0001);
#6110=CIRCLE('',#18601,0.0001);
#6111=CIRCLE('',#18602,9.99999999999974E-5);
#6112=CIRCLE('',#18604,9.99999969896684E-5);
#6113=CIRCLE('',#18606,0.0001);
#6114=CIRCLE('',#18608,0.0001);
#6115=CIRCLE('',#18611,9.99999999227393E-5);
#6116=CIRCLE('',#18612,9.99999999233536E-5);
#6117=CIRCLE('',#18613,9.99999999230291E-5);
#6118=CIRCLE('',#18614,9.99999999233779E-5);
#6119=CIRCLE('',#18617,0.00911255899884414);
#6120=CIRCLE('',#18618,0.00911585801383145);
#6121=CIRCLE('',#18748,0.00134890248414929);
#6122=CIRCLE('',#18749,0.00134890252382471);
#6123=CIRCLE('',#18751,0.0055);
#6124=CIRCLE('',#18752,0.017);
#6125=CIRCLE('',#18753,0.0005);
#6126=CIRCLE('',#18754,0.017);
#6127=CIRCLE('',#18755,0.0005);
#6128=CIRCLE('',#18756,0.017);
#6129=CIRCLE('',#18757,0.0005);
#6130=CIRCLE('',#18758,0.017);
#6131=CIRCLE('',#18759,0.0005);
#6132=CIRCLE('',#18761,0.0055);
#6133=CIRCLE('',#18763,0.0045);
#6134=CIRCLE('',#18765,0.017);
#6135=CIRCLE('',#18766,0.0005);
#6136=CIRCLE('',#18767,0.017);
#6137=CIRCLE('',#18768,0.0005);
#6138=CIRCLE('',#18769,0.017);
#6139=CIRCLE('',#18770,0.0005);
#6140=CIRCLE('',#18771,0.017);
#6141=CIRCLE('',#18772,0.0005);
#6142=CIRCLE('',#18773,0.00278445714771807);
#6143=CIRCLE('',#18783,0.00278445714771807);
#6144=CIRCLE('',#18784,0.00278445714771807);
#6145=CIRCLE('',#18786,0.00268445714771808);
#6146=CIRCLE('',#18787,0.00126635989804114);
#6147=CIRCLE('',#18789,0.0001);
#6148=CIRCLE('',#18791,0.00116635989804114);
#6149=CIRCLE('',#18792,0.00116635989804114);
#6150=CIRCLE('',#18794,0.00106635989804114);
#6151=CIRCLE('',#18797,0.00134579174568697);
#6152=CIRCLE('',#18798,0.00134832773590515);
#6153=CIRCLE('',#18799,0.00134579174568697);
#6154=CIRCLE('',#18802,0.00125);
#6155=CIRCLE('',#18805,0.000100021493280238);
#6156=CIRCLE('',#18807,0.0001);
#6157=CIRCLE('',#18809,0.0001);
#6158=CIRCLE('',#18811,0.001);
#6159=CIRCLE('',#18814,0.0002);
#6160=CIRCLE('',#18815,0.0014);
#6161=CIRCLE('',#18816,0.0002);
#6162=CIRCLE('',#18817,0.0006);
#6163=CIRCLE('',#18819,0.0002);
#6164=CIRCLE('',#18820,0.0014);
#6165=CIRCLE('',#18821,0.0002);
#6166=CIRCLE('',#18822,0.0006);
#6167=CIRCLE('',#18833,0.0015);
#6168=CIRCLE('',#18834,0.0015);
#6169=CIRCLE('',#18841,0.0005);
#6170=CIRCLE('',#18842,0.0005);
#6171=CIRCLE('',#18843,0.0005);
#6172=CIRCLE('',#18889,0.0001);
#6173=CIRCLE('',#18891,0.0001);
#6174=CIRCLE('',#18892,0.0001);
#6175=CIRCLE('',#18894,0.0001);
#6176=CIRCLE('',#18900,0.0001);
#6177=CIRCLE('',#18902,0.0001);
#6178=CIRCLE('',#18906,0.0001);
#6179=CIRCLE('',#18908,0.0001);
#6180=CIRCLE('',#18910,0.0001);
#6181=CIRCLE('',#18912,0.0001);
#6182=CIRCLE('',#18914,0.0001);
#6183=CIRCLE('',#18916,0.0001);
#6184=CIRCLE('',#18919,0.0001);
#6185=CIRCLE('',#18921,0.0001);
#6186=CIRCLE('',#18924,0.0015);
#6187=CIRCLE('',#18925,0.0015);
#6188=CIRCLE('',#18941,0.0002);
#6189=CIRCLE('',#18942,0.0014);
#6190=CIRCLE('',#18943,0.0002);
#6191=CIRCLE('',#18944,0.0002);
#6192=CIRCLE('',#18945,0.0006);
#6193=CIRCLE('',#18947,0.0002);
#6194=CIRCLE('',#18948,0.0002);
#6195=CIRCLE('',#18949,0.0014);
#6196=CIRCLE('',#18950,0.0002);
#6197=CIRCLE('',#18951,0.0006);
#6198=CIRCLE('',#18953,0.0005);
#6199=CIRCLE('',#18954,0.0005);
#6200=CIRCLE('',#18955,0.0005);
#6201=CIRCLE('',#18993,0.0001);
#6202=CIRCLE('',#18995,0.0001);
#6203=CIRCLE('',#18996,0.0001);
#6204=CIRCLE('',#18998,0.0001);
#6205=CIRCLE('',#19004,0.0001);
#6206=CIRCLE('',#19006,0.0001);
#6207=CIRCLE('',#19010,0.0001);
#6208=CIRCLE('',#19012,0.0001);
#6209=CIRCLE('',#19014,0.0001);
#6210=CIRCLE('',#19015,0.0001);
#6211=CIRCLE('',#19017,0.0001);
#6212=CIRCLE('',#19019,0.0001);
#6213=CIRCLE('',#19021,0.0001);
#6214=CIRCLE('',#19022,0.0001);
#6215=CIRCLE('',#19024,0.0001);
#6216=CIRCLE('',#19026,0.0001);
#6217=CIRCLE('',#19028,0.0001);
#6218=CIRCLE('',#19030,0.0001);
#6219=CIRCLE('',#19032,0.0001);
#6220=CIRCLE('',#19034,0.0001);
#6221=CIRCLE('',#19036,0.0001);
#6222=CIRCLE('',#19038,0.0001);
#6223=CIRCLE('',#19040,0.0001);
#6224=CIRCLE('',#19042,0.0001);
#6225=CIRCLE('',#19045,0.0001);
#6226=CIRCLE('',#19047,0.0001);
#6227=CIRCLE('',#19050,0.0011);
#6228=CIRCLE('',#19051,0.0011);
#6229=CIRCLE('',#19054,0.0005);
#6230=CIRCLE('',#19055,0.0005);
#6231=CIRCLE('',#19058,0.00125);
#6232=CIRCLE('',#19059,0.00125);
#6233=CIRCLE('',#19065,0.0085);
#6234=CIRCLE('',#19066,0.0055);
#6235=CIRCLE('',#19068,0.009);
#6236=CIRCLE('',#19069,0.009);
#6237=CIRCLE('',#19070,0.009);
#6238=CIRCLE('',#19072,0.0085);
#6239=CIRCLE('',#19073,0.0055);
#6240=CIRCLE('',#19076,0.0005);
#6241=CIRCLE('',#19078,0.0005);
#6242=CIRCLE('',#19081,0.00318247006517847);
#6243=CIRCLE('',#19082,0.00314126219074625);
#6244=CIRCLE('',#19083,0.00318247006517847);
#6245=CIRCLE('',#19084,0.00319919707806175);
#6246=CIRCLE('',#19085,0.00319919707806175);
#6247=CIRCLE('',#19086,0.00318247006517847);
#6248=CIRCLE('',#19087,0.00314126219074625);
#6249=CIRCLE('',#19088,0.00318247006517847);
#6250=CIRCLE('',#19089,0.00319919707806175);
#6251=CIRCLE('',#19090,0.00319919707806175);
#6252=CIRCLE('',#19091,0.00318247006517847);
#6253=CIRCLE('',#19092,0.00314126219074625);
#6254=CIRCLE('',#19093,0.0032);
#6255=CIRCLE('',#19094,0.002);
#6256=CIRCLE('',#19095,0.002);
#6257=CIRCLE('',#19096,0.00314126219074625);
#6258=CIRCLE('',#19097,0.00318247006517847);
#6259=CIRCLE('',#19098,0.00319919707806175);
#6260=CIRCLE('',#19099,0.00319919707806175);
#6261=CIRCLE('',#19100,0.00318247006517847);
#6262=CIRCLE('',#19101,0.00314126219074625);
#6263=CIRCLE('',#19102,0.00318247006517847);
#6264=CIRCLE('',#19103,0.00319919707806175);
#6265=CIRCLE('',#19104,0.00319919707806175);
#6266=CIRCLE('',#19106,0.002);
#6267=CIRCLE('',#19107,0.0011);
#6268=CIRCLE('',#19110,0.0008);
#6269=CIRCLE('',#19112,0.001);
#6270=CIRCLE('',#19113,0.001);
#6271=CIRCLE('',#19137,0.0001);
#6272=CIRCLE('',#19140,0.0135);
#6273=CIRCLE('',#19141,0.0135);
#6274=CIRCLE('',#19143,0.0135);
#6275=CIRCLE('',#19144,0.0135);
#6276=CIRCLE('',#19146,0.0134);
#6277=CIRCLE('',#19147,0.0134);
#6278=CIRCLE('',#19148,0.0091);
#6279=CIRCLE('',#19149,0.0013);
#6280=CIRCLE('',#19150,0.0006);
#6281=CIRCLE('',#19151,0.0006);
#6282=CIRCLE('',#19153,0.0134);
#6283=CIRCLE('',#19154,0.0134);
#6284=CIRCLE('',#19155,0.0091);
#6285=CIRCLE('',#19156,0.0013);
#6286=CIRCLE('',#19157,0.0006);
#6287=CIRCLE('',#19158,0.0006);
#6288=CIRCLE('',#19160,0.009);
#6289=CIRCLE('',#19161,0.009);
#6290=CIRCLE('',#19162,0.009);
#6291=CIRCLE('',#19163,0.009);
#6292=CIRCLE('',#19165,0.0012);
#6293=CIRCLE('',#19166,0.0012);
#6294=CIRCLE('',#19167,0.0012);
#6295=CIRCLE('',#19168,0.0012);
#6296=CIRCLE('',#19170,0.0005);
#6297=CIRCLE('',#19171,0.0005);
#6298=CIRCLE('',#19172,0.0005);
#6299=CIRCLE('',#19173,0.0005);
#6300=CIRCLE('',#19175,0.0005);
#6301=CIRCLE('',#19176,0.0005);
#6302=CIRCLE('',#19177,0.0005);
#6303=CIRCLE('',#19178,0.0005);
#6304=CIRCLE('',#19182,0.0001);
#6305=CIRCLE('',#19184,0.0001);
#6306=CIRCLE('',#19186,0.0001);
#6307=CIRCLE('',#19188,0.0001);
#6308=CIRCLE('',#19192,0.0001);
#6309=CIRCLE('',#19194,0.0001);
#6310=CIRCLE('',#19196,0.0001);
#6311=CIRCLE('',#19198,0.0001);
#6312=CIRCLE('',#19201,0.00236773842762747);
#6313=CIRCLE('',#19202,0.00236775519479021);
#6314=CIRCLE('',#19206,0.00265162305984738);
#6315=CIRCLE('',#19207,0.00265162305984738);
#6316=CIRCLE('',#19211,0.00236775519476243);
#6317=CIRCLE('',#19212,0.00236773842771933);
#6318=CIRCLE('',#19214,0.00170789487802692);
#6319=CIRCLE('',#19215,0.00170789487802692);
#6320=CIRCLE('',#19217,0.00160789487802693);
#6321=CIRCLE('',#19220,0.00255162305984738);
#6322=CIRCLE('',#19221,0.0011);
#6323=CIRCLE('',#19223,0.00160789487802693);
#6324=CIRCLE('',#19226,0.00255162305984738);
#6325=CIRCLE('',#19227,0.0011);
#6326=CIRCLE('',#19229,0.001);
#6327=CIRCLE('',#19230,0.001);
#6328=CIRCLE('',#19231,0.001);
#6329=CIRCLE('',#19232,0.001);
#6330=CIRCLE('',#19234,0.0001);
#6331=CIRCLE('',#19235,0.0001);
#6332=CIRCLE('',#19237,0.0001);
#6333=CIRCLE('',#19239,0.0001);
#6334=CIRCLE('',#19240,0.0001);
#6335=CIRCLE('',#19242,0.0001);
#6336=CIRCLE('',#19245,0.0001);
#6337=CIRCLE('',#19247,0.0001);
#6338=CIRCLE('',#19249,0.0001);
#6339=CIRCLE('',#19250,0.0001);
#6340=CIRCLE('',#19253,0.000100001088290115);
#6341=CIRCLE('',#19255,0.0001);
#6342=CIRCLE('',#19257,0.0001);
#6343=CIRCLE('',#19261,0.0001);
#6344=CIRCLE('',#19262,0.0001);
#6345=CIRCLE('',#19263,0.0001);
#6346=CIRCLE('',#19265,0.0001);
#6347=CIRCLE('',#19267,0.0001);
#6348=CIRCLE('',#19269,0.000100001089498111);
#6349=CIRCLE('',#19271,9.99999999999998E-5);
#6350=CIRCLE('',#19272,0.0001);
#6351=CIRCLE('',#19274,0.0001);
#6352=CIRCLE('',#19276,0.0001);
#6353=CIRCLE('',#19279,0.0001);
#6354=CIRCLE('',#19281,0.0001);
#6355=CIRCLE('',#19283,0.0001);
#6356=CIRCLE('',#19285,0.0001);
#6357=CIRCLE('',#19287,0.0001);
#6358=CIRCLE('',#19290,0.0001);
#6359=CIRCLE('',#19292,0.0001);
#6360=CIRCLE('',#19295,0.0125);
#6361=CIRCLE('',#19296,0.0125);
#6362=CIRCLE('',#19297,0.0125);
#6363=CIRCLE('',#19299,0.001);
#6364=CIRCLE('',#19300,0.001);
#6365=CIRCLE('',#19302,0.0132323601801219);
#6366=CIRCLE('',#19303,0.0132323601801219);
#6367=CIRCLE('',#19305,0.0132323601801219);
#6368=CIRCLE('',#19306,0.0132323601801219);
#6369=CIRCLE('',#19308,0.0123);
#6370=CIRCLE('',#19309,0.0127);
#6371=CIRCLE('',#19310,0.0125);
#6372=CIRCLE('',#19311,0.0130323601801219);
#6373=CIRCLE('',#19312,0.0004);
#6374=CIRCLE('',#19313,0.0013);
#6375=CIRCLE('',#19314,0.0130323601801219);
#6376=CIRCLE('',#19315,0.0013);
#6377=CIRCLE('',#19316,0.0004);
#6378=CIRCLE('',#19317,0.0130323601801219);
#6379=CIRCLE('',#19318,0.0005);
#6380=CIRCLE('',#19319,0.0005);
#6381=CIRCLE('',#19320,0.0005);
#6382=CIRCLE('',#19321,0.0005);
#6383=CIRCLE('',#19323,0.0125);
#6384=CIRCLE('',#19325,0.0125);
#6385=CIRCLE('',#19326,0.0125);
#6386=CIRCLE('',#19328,0.00500000000000001);
#6387=CIRCLE('',#19329,0.005);
#6388=CIRCLE('',#19330,0.005);
#6389=CIRCLE('',#19331,0.005);
#6390=CIRCLE('',#19332,0.005);
#6391=CIRCLE('',#19333,0.005);
#6392=CIRCLE('',#19335,0.0165);
#6393=CIRCLE('',#19336,0.0165);
#6394=CIRCLE('',#19339,0.0165);
#6395=CIRCLE('',#19340,0.0165);
#6396=CIRCLE('',#19343,0.0165);
#6397=CIRCLE('',#19344,0.0165);
#6398=CIRCLE('',#19346,0.0027);
#6399=CIRCLE('',#19347,0.0163);
#6400=CIRCLE('',#19348,0.0163);
#6401=CIRCLE('',#19349,0.0163);
#6402=CIRCLE('',#19350,0.0005);
#6403=CIRCLE('',#19351,0.0005);
#6404=CIRCLE('',#19352,0.0092);
#6405=CIRCLE('',#19354,0.0163);
#6406=CIRCLE('',#19355,0.0163);
#6407=CIRCLE('',#19356,0.0163);
#6408=CIRCLE('',#19357,0.0137);
#6409=CIRCLE('',#19358,0.0137);
#6410=CIRCLE('',#19360,0.0135);
#6411=CIRCLE('',#19361,0.0135);
#6412=CIRCLE('',#19363,0.0135);
#6413=CIRCLE('',#19364,0.0135);
#6414=CIRCLE('',#19366,0.0127);
#6415=CIRCLE('',#19367,0.0127);
#6416=CIRCLE('',#19368,0.0127);
#6417=CIRCLE('',#19369,0.0004);
#6418=CIRCLE('',#19370,0.0134323601801219);
#6419=CIRCLE('',#19371,0.0002);
#6420=CIRCLE('',#19372,0.0015);
#6421=CIRCLE('',#19373,0.0015);
#6422=CIRCLE('',#19374,0.0002);
#6423=CIRCLE('',#19375,0.0134323601801219);
#6424=CIRCLE('',#19376,0.0004);
#6425=CIRCLE('',#19378,0.0123);
#6426=CIRCLE('',#19379,0.0092);
#6427=CIRCLE('',#19381,0.009);
#6428=CIRCLE('',#19382,0.009);
#6429=CIRCLE('',#19383,0.009);
#6430=CIRCLE('',#19384,0.009);
#6431=CIRCLE('',#19390,0.004);
#6432=CIRCLE('',#19397,0.0132323601801219);
#6433=CIRCLE('',#19398,0.0132323601801219);
#6434=CIRCLE('',#19400,0.0015);
#6435=CIRCLE('',#19402,0.0015);
#6436=CIRCLE('',#19404,0.0023);
#6437=CIRCLE('',#19405,0.0012);
#6438=CIRCLE('',#19406,0.0005);
#6439=CIRCLE('',#19407,0.0005);
#6440=CIRCLE('',#19409,0.0025);
#6441=CIRCLE('',#19410,0.0025);
#6442=CIRCLE('',#19413,0.015);
#6443=CIRCLE('',#19414,0.015);
#6444=CIRCLE('',#19415,0.015);
#6445=CIRCLE('',#19416,0.015);
#6446=CIRCLE('',#19422,0.0002);
#6447=CIRCLE('',#19423,0.0002);
#6448=CIRCLE('',#19425,0.0002);
#6449=CIRCLE('',#19426,0.0002);
#6450=CIRCLE('',#19428,0.0002);
#6451=CIRCLE('',#19431,0.0002);
#6452=CIRCLE('',#19432,0.0002);
#6453=CIRCLE('',#19434,0.0002);
#6454=CIRCLE('',#19436,0.0002);
#6455=CIRCLE('',#19440,0.0002);
#6456=CIRCLE('',#19442,0.0002);
#6457=CIRCLE('',#19443,0.0002);
#6458=CIRCLE('',#19448,0.0002);
#6459=CIRCLE('',#19450,0.0002);
#6460=CIRCLE('',#19452,0.0002);
#6461=CIRCLE('',#19454,0.0002);
#6462=CIRCLE('',#19455,0.000199995253972718);
#6463=CIRCLE('',#19457,0.0002);
#6464=CIRCLE('',#19458,0.0002);
#6465=CIRCLE('',#19460,0.0002);
#6466=CIRCLE('',#19462,0.000200484899633866);
#6467=CIRCLE('',#19464,0.0002);
#6468=CIRCLE('',#19466,0.0002);
#6469=CIRCLE('',#19468,0.0002);
#6470=CIRCLE('',#19469,0.0002);
#6471=CIRCLE('',#19472,0.00017797030966603);
#6472=CIRCLE('',#19474,0.0002);
#6473=CIRCLE('',#19476,0.0002);
#6474=CIRCLE('',#19478,0.0002);
#6475=CIRCLE('',#19480,0.000199995408286236);
#6476=CIRCLE('',#19482,0.0002);
#6477=CIRCLE('',#19484,0.0002);
#6478=CIRCLE('',#19486,0.0002);
#6479=CIRCLE('',#19488,0.0002);
#6480=CIRCLE('',#19490,0.0002);
#6481=CIRCLE('',#19494,0.0002);
#6482=CIRCLE('',#19496,0.0002);
#6483=CIRCLE('',#19498,0.0002);
#6484=CIRCLE('',#19499,0.0002);
#6485=CIRCLE('',#19501,0.0002);
#6486=CIRCLE('',#19504,0.0125);
#6487=CIRCLE('',#19505,0.0002);
#6488=CIRCLE('',#19507,0.0002);
#6489=CIRCLE('',#19508,0.0002);
#6490=CIRCLE('',#19510,0.0002);
#6491=CIRCLE('',#19511,0.000200000000000081);
#6492=CIRCLE('',#19513,0.0002);
#6493=CIRCLE('',#19515,0.000199999999999959);
#6494=CIRCLE('',#19517,0.0002);
#6495=CIRCLE('',#19518,0.0002);
#6496=CIRCLE('',#19520,0.0002);
#6497=CIRCLE('',#19522,0.0002);
#6498=CIRCLE('',#19524,0.0002);
#6499=CIRCLE('',#19529,0.0002);
#6500=CIRCLE('',#19531,0.0002);
#6501=CIRCLE('',#19533,0.0002);
#6502=CIRCLE('',#19535,0.0002);
#6503=CIRCLE('',#19536,0.0002);
#6504=CIRCLE('',#19538,0.0002);
#6505=CIRCLE('',#19540,0.0002);
#6506=CIRCLE('',#19542,0.0002);
#6507=CIRCLE('',#19545,0.0002);
#6508=CIRCLE('',#19549,0.002);
#6509=CIRCLE('',#19550,0.00199565795815631);
#6510=CIRCLE('',#19552,0.00199545369122859);
#6511=CIRCLE('',#19554,0.00175917590714212);
#6512=CIRCLE('',#19555,0.002);
#6513=CIRCLE('',#19556,0.00199999989085889);
#6514=CIRCLE('',#19559,0.00199999684224345);
#6515=CIRCLE('',#19560,0.002);
#6516=CIRCLE('',#19561,0.00198947184167493);
#6517=CIRCLE('',#19563,0.00198949433969945);
#6518=CIRCLE('',#19565,0.00197761179274946);
#6519=CIRCLE('',#19567,0.00199597791916769);
#6520=CIRCLE('',#19568,0.002);
#6521=CIRCLE('',#19576,0.001);
#6522=CIRCLE('',#19579,0.001);
#6523=CIRCLE('',#19580,0.00102870127000254);
#6524=CIRCLE('',#19582,0.0005);
#6525=CIRCLE('',#19584,0.0005);
#6526=VERTEX_POINT('',#23729);
#6527=VERTEX_POINT('',#23730);
#6528=VERTEX_POINT('',#23732);
#6529=VERTEX_POINT('',#23734);
#6530=VERTEX_POINT('',#23736);
#6531=VERTEX_POINT('',#23738);
#6532=VERTEX_POINT('',#23740);
#6533=VERTEX_POINT('',#23742);
#6534=VERTEX_POINT('',#23744);
#6535=VERTEX_POINT('',#23746);
#6536=VERTEX_POINT('',#23748);
#6537=VERTEX_POINT('',#23750);
#6538=VERTEX_POINT('',#23752);
#6539=VERTEX_POINT('',#23754);
#6540=VERTEX_POINT('',#23756);
#6541=VERTEX_POINT('',#23758);
#6542=VERTEX_POINT('',#23760);
#6543=VERTEX_POINT('',#23762);
#6544=VERTEX_POINT('',#23764);
#6545=VERTEX_POINT('',#23766);
#6546=VERTEX_POINT('',#23768);
#6547=VERTEX_POINT('',#23770);
#6548=VERTEX_POINT('',#23772);
#6549=VERTEX_POINT('',#23774);
#6550=VERTEX_POINT('',#23776);
#6551=VERTEX_POINT('',#23778);
#6552=VERTEX_POINT('',#23780);
#6553=VERTEX_POINT('',#23782);
#6554=VERTEX_POINT('',#23784);
#6555=VERTEX_POINT('',#23786);
#6556=VERTEX_POINT('',#23788);
#6557=VERTEX_POINT('',#23790);
#6558=VERTEX_POINT('',#23792);
#6559=VERTEX_POINT('',#23794);
#6560=VERTEX_POINT('',#23796);
#6561=VERTEX_POINT('',#23798);
#6562=VERTEX_POINT('',#23800);
#6563=VERTEX_POINT('',#23802);
#6564=VERTEX_POINT('',#23804);
#6565=VERTEX_POINT('',#23806);
#6566=VERTEX_POINT('',#23808);
#6567=VERTEX_POINT('',#23810);
#6568=VERTEX_POINT('',#23812);
#6569=VERTEX_POINT('',#23814);
#6570=VERTEX_POINT('',#23816);
#6571=VERTEX_POINT('',#23818);
#6572=VERTEX_POINT('',#23820);
#6573=VERTEX_POINT('',#23822);
#6574=VERTEX_POINT('',#23824);
#6575=VERTEX_POINT('',#23826);
#6576=VERTEX_POINT('',#23828);
#6577=VERTEX_POINT('',#23830);
#6578=VERTEX_POINT('',#23832);
#6579=VERTEX_POINT('',#23834);
#6580=VERTEX_POINT('',#23836);
#6581=VERTEX_POINT('',#23838);
#6582=VERTEX_POINT('',#23840);
#6583=VERTEX_POINT('',#23842);
#6584=VERTEX_POINT('',#23844);
#6585=VERTEX_POINT('',#23846);
#6586=VERTEX_POINT('',#23848);
#6587=VERTEX_POINT('',#23850);
#6588=VERTEX_POINT('',#23852);
#6589=VERTEX_POINT('',#23854);
#6590=VERTEX_POINT('',#23856);
#6591=VERTEX_POINT('',#23858);
#6592=VERTEX_POINT('',#23860);
#6593=VERTEX_POINT('',#23862);
#6594=VERTEX_POINT('',#23864);
#6595=VERTEX_POINT('',#23866);
#6596=VERTEX_POINT('',#23868);
#6597=VERTEX_POINT('',#23870);
#6598=VERTEX_POINT('',#23872);
#6599=VERTEX_POINT('',#23874);
#6600=VERTEX_POINT('',#23876);
#6601=VERTEX_POINT('',#23878);
#6602=VERTEX_POINT('',#23880);
#6603=VERTEX_POINT('',#23882);
#6604=VERTEX_POINT('',#23884);
#6605=VERTEX_POINT('',#23886);
#6606=VERTEX_POINT('',#23888);
#6607=VERTEX_POINT('',#23890);
#6608=VERTEX_POINT('',#23892);
#6609=VERTEX_POINT('',#23894);
#6610=VERTEX_POINT('',#23896);
#6611=VERTEX_POINT('',#23898);
#6612=VERTEX_POINT('',#23900);
#6613=VERTEX_POINT('',#23902);
#6614=VERTEX_POINT('',#23904);
#6615=VERTEX_POINT('',#23906);
#6616=VERTEX_POINT('',#23908);
#6617=VERTEX_POINT('',#23910);
#6618=VERTEX_POINT('',#23912);
#6619=VERTEX_POINT('',#23914);
#6620=VERTEX_POINT('',#23916);
#6621=VERTEX_POINT('',#23918);
#6622=VERTEX_POINT('',#23920);
#6623=VERTEX_POINT('',#23922);
#6624=VERTEX_POINT('',#23924);
#6625=VERTEX_POINT('',#23926);
#6626=VERTEX_POINT('',#23928);
#6627=VERTEX_POINT('',#23930);
#6628=VERTEX_POINT('',#23932);
#6629=VERTEX_POINT('',#23934);
#6630=VERTEX_POINT('',#23936);
#6631=VERTEX_POINT('',#23938);
#6632=VERTEX_POINT('',#23940);
#6633=VERTEX_POINT('',#23942);
#6634=VERTEX_POINT('',#23944);
#6635=VERTEX_POINT('',#23946);
#6636=VERTEX_POINT('',#23948);
#6637=VERTEX_POINT('',#23950);
#6638=VERTEX_POINT('',#23952);
#6639=VERTEX_POINT('',#23954);
#6640=VERTEX_POINT('',#23956);
#6641=VERTEX_POINT('',#23958);
#6642=VERTEX_POINT('',#23960);
#6643=VERTEX_POINT('',#23962);
#6644=VERTEX_POINT('',#23964);
#6645=VERTEX_POINT('',#23966);
#6646=VERTEX_POINT('',#23968);
#6647=VERTEX_POINT('',#23970);
#6648=VERTEX_POINT('',#23972);
#6649=VERTEX_POINT('',#23974);
#6650=VERTEX_POINT('',#23976);
#6651=VERTEX_POINT('',#23978);
#6652=VERTEX_POINT('',#23980);
#6653=VERTEX_POINT('',#23982);
#6654=VERTEX_POINT('',#23984);
#6655=VERTEX_POINT('',#23986);
#6656=VERTEX_POINT('',#23988);
#6657=VERTEX_POINT('',#23990);
#6658=VERTEX_POINT('',#23992);
#6659=VERTEX_POINT('',#23994);
#6660=VERTEX_POINT('',#23996);
#6661=VERTEX_POINT('',#23998);
#6662=VERTEX_POINT('',#24000);
#6663=VERTEX_POINT('',#24002);
#6664=VERTEX_POINT('',#24004);
#6665=VERTEX_POINT('',#24006);
#6666=VERTEX_POINT('',#24008);
#6667=VERTEX_POINT('',#24010);
#6668=VERTEX_POINT('',#24012);
#6669=VERTEX_POINT('',#24014);
#6670=VERTEX_POINT('',#24016);
#6671=VERTEX_POINT('',#24018);
#6672=VERTEX_POINT('',#24020);
#6673=VERTEX_POINT('',#24022);
#6674=VERTEX_POINT('',#24024);
#6675=VERTEX_POINT('',#24026);
#6676=VERTEX_POINT('',#24028);
#6677=VERTEX_POINT('',#24030);
#6678=VERTEX_POINT('',#24032);
#6679=VERTEX_POINT('',#24034);
#6680=VERTEX_POINT('',#24036);
#6681=VERTEX_POINT('',#24038);
#6682=VERTEX_POINT('',#24040);
#6683=VERTEX_POINT('',#24042);
#6684=VERTEX_POINT('',#24044);
#6685=VERTEX_POINT('',#24046);
#6686=VERTEX_POINT('',#24048);
#6687=VERTEX_POINT('',#24050);
#6688=VERTEX_POINT('',#24052);
#6689=VERTEX_POINT('',#24054);
#6690=VERTEX_POINT('',#24056);
#6691=VERTEX_POINT('',#24058);
#6692=VERTEX_POINT('',#24060);
#6693=VERTEX_POINT('',#24062);
#6694=VERTEX_POINT('',#24064);
#6695=VERTEX_POINT('',#24066);
#6696=VERTEX_POINT('',#24068);
#6697=VERTEX_POINT('',#24070);
#6698=VERTEX_POINT('',#24072);
#6699=VERTEX_POINT('',#24074);
#6700=VERTEX_POINT('',#24076);
#6701=VERTEX_POINT('',#24078);
#6702=VERTEX_POINT('',#24080);
#6703=VERTEX_POINT('',#24082);
#6704=VERTEX_POINT('',#24084);
#6705=VERTEX_POINT('',#24086);
#6706=VERTEX_POINT('',#24088);
#6707=VERTEX_POINT('',#24090);
#6708=VERTEX_POINT('',#24092);
#6709=VERTEX_POINT('',#24094);
#6710=VERTEX_POINT('',#24097);
#6711=VERTEX_POINT('',#24100);
#6712=VERTEX_POINT('',#24102);
#6713=VERTEX_POINT('',#24106);
#6714=VERTEX_POINT('',#24108);
#6715=VERTEX_POINT('',#24112);
#6716=VERTEX_POINT('',#24114);
#6717=VERTEX_POINT('',#24118);
#6718=VERTEX_POINT('',#24120);
#6719=VERTEX_POINT('',#24124);
#6720=VERTEX_POINT('',#24126);
#6721=VERTEX_POINT('',#24130);
#6722=VERTEX_POINT('',#24132);
#6723=VERTEX_POINT('',#24136);
#6724=VERTEX_POINT('',#24138);
#6725=VERTEX_POINT('',#24142);
#6726=VERTEX_POINT('',#24144);
#6727=VERTEX_POINT('',#24148);
#6728=VERTEX_POINT('',#24150);
#6729=VERTEX_POINT('',#24154);
#6730=VERTEX_POINT('',#24156);
#6731=VERTEX_POINT('',#24160);
#6732=VERTEX_POINT('',#24162);
#6733=VERTEX_POINT('',#24166);
#6734=VERTEX_POINT('',#24168);
#6735=VERTEX_POINT('',#24172);
#6736=VERTEX_POINT('',#24174);
#6737=VERTEX_POINT('',#24178);
#6738=VERTEX_POINT('',#24180);
#6739=VERTEX_POINT('',#24184);
#6740=VERTEX_POINT('',#24186);
#6741=VERTEX_POINT('',#24190);
#6742=VERTEX_POINT('',#24192);
#6743=VERTEX_POINT('',#24196);
#6744=VERTEX_POINT('',#24198);
#6745=VERTEX_POINT('',#24202);
#6746=VERTEX_POINT('',#24204);
#6747=VERTEX_POINT('',#24208);
#6748=VERTEX_POINT('',#24210);
#6749=VERTEX_POINT('',#24214);
#6750=VERTEX_POINT('',#24216);
#6751=VERTEX_POINT('',#24220);
#6752=VERTEX_POINT('',#24222);
#6753=VERTEX_POINT('',#24226);
#6754=VERTEX_POINT('',#24228);
#6755=VERTEX_POINT('',#24232);
#6756=VERTEX_POINT('',#24234);
#6757=VERTEX_POINT('',#24238);
#6758=VERTEX_POINT('',#24240);
#6759=VERTEX_POINT('',#24244);
#6760=VERTEX_POINT('',#24246);
#6761=VERTEX_POINT('',#24250);
#6762=VERTEX_POINT('',#24252);
#6763=VERTEX_POINT('',#24256);
#6764=VERTEX_POINT('',#24258);
#6765=VERTEX_POINT('',#24262);
#6766=VERTEX_POINT('',#24264);
#6767=VERTEX_POINT('',#24268);
#6768=VERTEX_POINT('',#24270);
#6769=VERTEX_POINT('',#24274);
#6770=VERTEX_POINT('',#24276);
#6771=VERTEX_POINT('',#24280);
#6772=VERTEX_POINT('',#24282);
#6773=VERTEX_POINT('',#24286);
#6774=VERTEX_POINT('',#24288);
#6775=VERTEX_POINT('',#24292);
#6776=VERTEX_POINT('',#24294);
#6777=VERTEX_POINT('',#24298);
#6778=VERTEX_POINT('',#24300);
#6779=VERTEX_POINT('',#24304);
#6780=VERTEX_POINT('',#24306);
#6781=VERTEX_POINT('',#24310);
#6782=VERTEX_POINT('',#24312);
#6783=VERTEX_POINT('',#24316);
#6784=VERTEX_POINT('',#24318);
#6785=VERTEX_POINT('',#24322);
#6786=VERTEX_POINT('',#24324);
#6787=VERTEX_POINT('',#24328);
#6788=VERTEX_POINT('',#24330);
#6789=VERTEX_POINT('',#24334);
#6790=VERTEX_POINT('',#24336);
#6791=VERTEX_POINT('',#24340);
#6792=VERTEX_POINT('',#24342);
#6793=VERTEX_POINT('',#24346);
#6794=VERTEX_POINT('',#24348);
#6795=VERTEX_POINT('',#24352);
#6796=VERTEX_POINT('',#24354);
#6797=VERTEX_POINT('',#24358);
#6798=VERTEX_POINT('',#24360);
#6799=VERTEX_POINT('',#24364);
#6800=VERTEX_POINT('',#24366);
#6801=VERTEX_POINT('',#24370);
#6802=VERTEX_POINT('',#24372);
#6803=VERTEX_POINT('',#24374);
#6804=VERTEX_POINT('',#24377);
#6805=VERTEX_POINT('',#24379);
#6806=VERTEX_POINT('',#24382);
#6807=VERTEX_POINT('',#24384);
#6808=VERTEX_POINT('',#24387);
#6809=VERTEX_POINT('',#24389);
#6810=VERTEX_POINT('',#24392);
#6811=VERTEX_POINT('',#24394);
#6812=VERTEX_POINT('',#24397);
#6813=VERTEX_POINT('',#24399);
#6814=VERTEX_POINT('',#24402);
#6815=VERTEX_POINT('',#24404);
#6816=VERTEX_POINT('',#24407);
#6817=VERTEX_POINT('',#24409);
#6818=VERTEX_POINT('',#24412);
#6819=VERTEX_POINT('',#24414);
#6820=VERTEX_POINT('',#24417);
#6821=VERTEX_POINT('',#24419);
#6822=VERTEX_POINT('',#24422);
#6823=VERTEX_POINT('',#24424);
#6824=VERTEX_POINT('',#24426);
#6825=VERTEX_POINT('',#24428);
#6826=VERTEX_POINT('',#24430);
#6827=VERTEX_POINT('',#24432);
#6828=VERTEX_POINT('',#24435);
#6829=VERTEX_POINT('',#24437);
#6830=VERTEX_POINT('',#24440);
#6831=VERTEX_POINT('',#24442);
#6832=VERTEX_POINT('',#24445);
#6833=VERTEX_POINT('',#24447);
#6834=VERTEX_POINT('',#24450);
#6835=VERTEX_POINT('',#24452);
#6836=VERTEX_POINT('',#24455);
#6837=VERTEX_POINT('',#24457);
#6838=VERTEX_POINT('',#24460);
#6839=VERTEX_POINT('',#24462);
#6840=VERTEX_POINT('',#24465);
#6841=VERTEX_POINT('',#24467);
#6842=VERTEX_POINT('',#24470);
#6843=VERTEX_POINT('',#24472);
#6844=VERTEX_POINT('',#24475);
#6845=VERTEX_POINT('',#24477);
#6846=VERTEX_POINT('',#24480);
#6847=VERTEX_POINT('',#24482);
#6848=VERTEX_POINT('',#24485);
#6849=VERTEX_POINT('',#24487);
#6850=VERTEX_POINT('',#24490);
#6851=VERTEX_POINT('',#24492);
#6852=VERTEX_POINT('',#24495);
#6853=VERTEX_POINT('',#24497);
#6854=VERTEX_POINT('',#24500);
#6855=VERTEX_POINT('',#24502);
#6856=VERTEX_POINT('',#24505);
#6857=VERTEX_POINT('',#24507);
#6858=VERTEX_POINT('',#24510);
#6859=VERTEX_POINT('',#24512);
#6860=VERTEX_POINT('',#24515);
#6861=VERTEX_POINT('',#24517);
#6862=VERTEX_POINT('',#24520);
#6863=VERTEX_POINT('',#24522);
#6864=VERTEX_POINT('',#24525);
#6865=VERTEX_POINT('',#24527);
#6866=VERTEX_POINT('',#24530);
#6867=VERTEX_POINT('',#24532);
#6868=VERTEX_POINT('',#24535);
#6869=VERTEX_POINT('',#24537);
#6870=VERTEX_POINT('',#24540);
#6871=VERTEX_POINT('',#24542);
#6872=VERTEX_POINT('',#24545);
#6873=VERTEX_POINT('',#24547);
#6874=VERTEX_POINT('',#24550);
#6875=VERTEX_POINT('',#24552);
#6876=VERTEX_POINT('',#24555);
#6877=VERTEX_POINT('',#24557);
#6878=VERTEX_POINT('',#24560);
#6879=VERTEX_POINT('',#24562);
#6880=VERTEX_POINT('',#24565);
#6881=VERTEX_POINT('',#24567);
#6882=VERTEX_POINT('',#24570);
#6883=VERTEX_POINT('',#24572);
#6884=VERTEX_POINT('',#24575);
#6885=VERTEX_POINT('',#24577);
#6886=VERTEX_POINT('',#24580);
#6887=VERTEX_POINT('',#24582);
#6888=VERTEX_POINT('',#24585);
#6889=VERTEX_POINT('',#24587);
#6890=VERTEX_POINT('',#24590);
#6891=VERTEX_POINT('',#24592);
#6892=VERTEX_POINT('',#24595);
#6893=VERTEX_POINT('',#24597);
#6894=VERTEX_POINT('',#24600);
#6895=VERTEX_POINT('',#24603);
#6896=VERTEX_POINT('',#24898);
#6897=VERTEX_POINT('',#24899);
#6898=VERTEX_POINT('',#24903);
#6899=VERTEX_POINT('',#25046);
#6900=VERTEX_POINT('',#25050);
#6901=VERTEX_POINT('',#25209);
#6902=VERTEX_POINT('',#25212);
#6903=VERTEX_POINT('',#25215);
#6904=VERTEX_POINT('',#25224);
#6905=VERTEX_POINT('',#25244);
#6906=VERTEX_POINT('',#25297);
#6907=VERTEX_POINT('',#25298);
#6908=VERTEX_POINT('',#25301);
#6909=VERTEX_POINT('',#25303);
#6910=VERTEX_POINT('',#25307);
#6911=VERTEX_POINT('',#25309);
#6912=VERTEX_POINT('',#25311);
#6913=VERTEX_POINT('',#25315);
#6914=VERTEX_POINT('',#25316);
#6915=VERTEX_POINT('',#25319);
#6916=VERTEX_POINT('',#25321);
#6917=VERTEX_POINT('',#25325);
#6918=VERTEX_POINT('',#25327);
#6919=VERTEX_POINT('',#25329);
#6920=VERTEX_POINT('',#25333);
#6921=VERTEX_POINT('',#25335);
#6922=VERTEX_POINT('',#25338);
#6923=VERTEX_POINT('',#25341);
#6924=VERTEX_POINT('',#25342);
#6925=VERTEX_POINT('',#25345);
#6926=VERTEX_POINT('',#25349);
#6927=VERTEX_POINT('',#25350);
#6928=VERTEX_POINT('',#25353);
#6929=VERTEX_POINT('',#25357);
#6930=VERTEX_POINT('',#25359);
#6931=VERTEX_POINT('',#25361);
#6932=VERTEX_POINT('',#25365);
#6933=VERTEX_POINT('',#25367);
#6934=VERTEX_POINT('',#25369);
#6935=VERTEX_POINT('',#25373);
#6936=VERTEX_POINT('',#25374);
#6937=VERTEX_POINT('',#25377);
#6938=VERTEX_POINT('',#25381);
#6939=VERTEX_POINT('',#25382);
#6940=VERTEX_POINT('',#25385);
#6941=VERTEX_POINT('',#25389);
#6942=VERTEX_POINT('',#25391);
#6943=VERTEX_POINT('',#25393);
#6944=VERTEX_POINT('',#25397);
#6945=VERTEX_POINT('',#25398);
#6946=VERTEX_POINT('',#25401);
#6947=VERTEX_POINT('',#25405);
#6948=VERTEX_POINT('',#25407);
#6949=VERTEX_POINT('',#25409);
#6950=VERTEX_POINT('',#25413);
#6951=VERTEX_POINT('',#25414);
#6952=VERTEX_POINT('',#25417);
#6953=VERTEX_POINT('',#25421);
#6954=VERTEX_POINT('',#25423);
#6955=VERTEX_POINT('',#25425);
#6956=VERTEX_POINT('',#25429);
#6957=VERTEX_POINT('',#25430);
#6958=VERTEX_POINT('',#25433);
#6959=VERTEX_POINT('',#25437);
#6960=VERTEX_POINT('',#25439);
#6961=VERTEX_POINT('',#25441);
#6962=VERTEX_POINT('',#25504);
#6963=VERTEX_POINT('',#25545);
#6964=VERTEX_POINT('',#25554);
#6965=VERTEX_POINT('',#25557);
#6966=VERTEX_POINT('',#25560);
#6967=VERTEX_POINT('',#25561);
#6968=VERTEX_POINT('',#25587);
#6969=VERTEX_POINT('',#25625);
#6970=VERTEX_POINT('',#25841);
#6971=VERTEX_POINT('',#25842);
#6972=VERTEX_POINT('',#26001);
#6973=VERTEX_POINT('',#26002);
#6974=VERTEX_POINT('',#26007);
#6975=VERTEX_POINT('',#26027);
#6976=VERTEX_POINT('',#26056);
#6977=VERTEX_POINT('',#26064);
#6978=VERTEX_POINT('',#26069);
#6979=VERTEX_POINT('',#26157);
#6980=VERTEX_POINT('',#26158);
#6981=VERTEX_POINT('',#26161);
#6982=VERTEX_POINT('',#26166);
#6983=VERTEX_POINT('',#26351);
#6984=VERTEX_POINT('',#26357);
#6985=VERTEX_POINT('',#26542);
#6986=VERTEX_POINT('',#26547);
#6987=VERTEX_POINT('',#26550);
#6988=VERTEX_POINT('',#26590);
#6989=VERTEX_POINT('',#26613);
#6990=VERTEX_POINT('',#26678);
#6991=VERTEX_POINT('',#26691);
#6992=VERTEX_POINT('',#26732);
#6993=VERTEX_POINT('',#26867);
#6994=VERTEX_POINT('',#26868);
#6995=VERTEX_POINT('',#26871);
#6996=VERTEX_POINT('',#26914);
#6997=VERTEX_POINT('',#26943);
#6998=VERTEX_POINT('',#26978);
#6999=VERTEX_POINT('',#27004);
#7000=VERTEX_POINT('',#27006);
#7001=VERTEX_POINT('',#27008);
#7002=VERTEX_POINT('',#27019);
#7003=VERTEX_POINT('',#27027);
#7004=VERTEX_POINT('',#27032);
#7005=VERTEX_POINT('',#27061);
#7006=VERTEX_POINT('',#27075);
#7007=VERTEX_POINT('',#27098);
#7008=VERTEX_POINT('',#27115);
#7009=VERTEX_POINT('',#27118);
#7010=VERTEX_POINT('',#27129);
#7011=VERTEX_POINT('',#27141);
#7012=VERTEX_POINT('',#27154);
#7013=VERTEX_POINT('',#27156);
#7014=VERTEX_POINT('',#27169);
#7015=VERTEX_POINT('',#27181);
#7016=VERTEX_POINT('',#27192);
#7017=VERTEX_POINT('',#27195);
#7018=VERTEX_POINT('',#27206);
#7019=VERTEX_POINT('',#27218);
#7020=VERTEX_POINT('',#27231);
#7021=VERTEX_POINT('',#27233);
#7022=VERTEX_POINT('',#27246);
#7023=VERTEX_POINT('',#27258);
#7024=VERTEX_POINT('',#27269);
#7025=VERTEX_POINT('',#27272);
#7026=VERTEX_POINT('',#27283);
#7027=VERTEX_POINT('',#27295);
#7028=VERTEX_POINT('',#27308);
#7029=VERTEX_POINT('',#27340);
#7030=VERTEX_POINT('',#27354);
#7031=VERTEX_POINT('',#27366);
#7032=VERTEX_POINT('',#27377);
#7033=VERTEX_POINT('',#27380);
#7034=VERTEX_POINT('',#27391);
#7035=VERTEX_POINT('',#27396);
#7036=VERTEX_POINT('',#27425);
#7037=VERTEX_POINT('',#27475);
#7038=VERTEX_POINT('',#27483);
#7039=VERTEX_POINT('',#27492);
#7040=VERTEX_POINT('',#27500);
#7041=VERTEX_POINT('',#27529);
#7042=VERTEX_POINT('',#27555);
#7043=VERTEX_POINT('',#27575);
#7044=VERTEX_POINT('',#27578);
#7045=VERTEX_POINT('',#27598);
#7046=VERTEX_POINT('',#27624);
#7047=VERTEX_POINT('',#27653);
#7048=VERTEX_POINT('',#27655);
#7049=VERTEX_POINT('',#27675);
#7050=VERTEX_POINT('',#27685);
#7051=VERTEX_POINT('',#27688);
#7052=VERTEX_POINT('',#27711);
#7053=VERTEX_POINT('',#27770);
#7054=VERTEX_POINT('',#27772);
#7055=VERTEX_POINT('',#27794);
#7056=VERTEX_POINT('',#27805);
#7057=VERTEX_POINT('',#27808);
#7058=VERTEX_POINT('',#27831);
#7059=VERTEX_POINT('',#27890);
#7060=VERTEX_POINT('',#27892);
#7061=VERTEX_POINT('',#27914);
#7062=VERTEX_POINT('',#27925);
#7063=VERTEX_POINT('',#27928);
#7064=VERTEX_POINT('',#27939);
#7065=VERTEX_POINT('',#27998);
#7066=VERTEX_POINT('',#28000);
#7067=VERTEX_POINT('',#28022);
#7068=VERTEX_POINT('',#28033);
#7069=VERTEX_POINT('',#28036);
#7070=VERTEX_POINT('',#28047);
#7071=VERTEX_POINT('',#28106);
#7072=VERTEX_POINT('',#28108);
#7073=VERTEX_POINT('',#28130);
#7074=VERTEX_POINT('',#28141);
#7075=VERTEX_POINT('',#28144);
#7076=VERTEX_POINT('',#28155);
#7077=VERTEX_POINT('',#28177);
#7078=VERTEX_POINT('',#28179);
#7079=VERTEX_POINT('',#28201);
#7080=VERTEX_POINT('',#28212);
#7081=VERTEX_POINT('',#28215);
#7082=VERTEX_POINT('',#28232);
#7083=VERTEX_POINT('',#28254);
#7084=VERTEX_POINT('',#28256);
#7085=VERTEX_POINT('',#28263);
#7086=VERTEX_POINT('',#28273);
#7087=VERTEX_POINT('',#28276);
#7088=VERTEX_POINT('',#28296);
#7089=VERTEX_POINT('',#28349);
#7090=VERTEX_POINT('',#28351);
#7091=VERTEX_POINT('',#28404);
#7092=VERTEX_POINT('',#28414);
#7093=VERTEX_POINT('',#28417);
#7094=VERTEX_POINT('',#28437);
#7095=VERTEX_POINT('',#28490);
#7096=VERTEX_POINT('',#28492);
#7097=VERTEX_POINT('',#28545);
#7098=VERTEX_POINT('',#28555);
#7099=VERTEX_POINT('',#28558);
#7100=VERTEX_POINT('',#28578);
#7101=VERTEX_POINT('',#28631);
#7102=VERTEX_POINT('',#28633);
#7103=VERTEX_POINT('',#28653);
#7104=VERTEX_POINT('',#28663);
#7105=VERTEX_POINT('',#28666);
#7106=VERTEX_POINT('',#28686);
#7107=VERTEX_POINT('',#28739);
#7108=VERTEX_POINT('',#28741);
#7109=VERTEX_POINT('',#28761);
#7110=VERTEX_POINT('',#28771);
#7111=VERTEX_POINT('',#28774);
#7112=VERTEX_POINT('',#28794);
#7113=VERTEX_POINT('',#28847);
#7114=VERTEX_POINT('',#28849);
#7115=VERTEX_POINT('',#28869);
#7116=VERTEX_POINT('',#28879);
#7117=VERTEX_POINT('',#28882);
#7118=VERTEX_POINT('',#28902);
#7119=VERTEX_POINT('',#28907);
#7120=VERTEX_POINT('',#28960);
#7121=VERTEX_POINT('',#28970);
#7122=VERTEX_POINT('',#28980);
#7123=VERTEX_POINT('',#29030);
#7124=VERTEX_POINT('',#29053);
#7125=VERTEX_POINT('',#29056);
#7126=VERTEX_POINT('',#29061);
#7127=VERTEX_POINT('',#29066);
#7128=VERTEX_POINT('',#29080);
#7129=VERTEX_POINT('',#29085);
#7130=VERTEX_POINT('',#29090);
#7131=VERTEX_POINT('',#29108);
#7132=VERTEX_POINT('',#29269);
#7133=VERTEX_POINT('',#29270);
#7134=VERTEX_POINT('',#29275);
#7135=VERTEX_POINT('',#29331);
#7136=VERTEX_POINT('',#29350);
#7137=VERTEX_POINT('',#29421);
#7138=VERTEX_POINT('',#29462);
#7139=VERTEX_POINT('',#29467);
#7140=VERTEX_POINT('',#29475);
#7141=VERTEX_POINT('',#29510);
#7142=VERTEX_POINT('',#29515);
#7143=VERTEX_POINT('',#29526);
#7144=VERTEX_POINT('',#29537);
#7145=VERTEX_POINT('',#29546);
#7146=VERTEX_POINT('',#29553);
#7147=VERTEX_POINT('',#29560);
#7148=VERTEX_POINT('',#29567);
#7149=VERTEX_POINT('',#29574);
#7150=VERTEX_POINT('',#29581);
#7151=VERTEX_POINT('',#29595);
#7152=VERTEX_POINT('',#29669);
#7153=VERTEX_POINT('',#29734);
#7154=VERTEX_POINT('',#29772);
#7155=VERTEX_POINT('',#29779);
#7156=VERTEX_POINT('',#29781);
#7157=VERTEX_POINT('',#29788);
#7158=VERTEX_POINT('',#29790);
#7159=VERTEX_POINT('',#29797);
#7160=VERTEX_POINT('',#29806);
#7161=VERTEX_POINT('',#29814);
#7162=VERTEX_POINT('',#29825);
#7163=VERTEX_POINT('',#29834);
#7164=VERTEX_POINT('',#29841);
#7165=VERTEX_POINT('',#29848);
#7166=VERTEX_POINT('',#29855);
#7167=VERTEX_POINT('',#29862);
#7168=VERTEX_POINT('',#29869);
#7169=VERTEX_POINT('',#29892);
#7170=VERTEX_POINT('',#29893);
#7171=VERTEX_POINT('',#29900);
#7172=VERTEX_POINT('',#29909);
#7173=VERTEX_POINT('',#29985);
#7174=VERTEX_POINT('',#29986);
#7175=VERTEX_POINT('',#29995);
#7176=VERTEX_POINT('',#30002);
#7177=VERTEX_POINT('',#30157);
#7178=VERTEX_POINT('',#30177);
#7179=VERTEX_POINT('',#30304);
#7180=VERTEX_POINT('',#30305);
#7181=VERTEX_POINT('',#30312);
#7182=VERTEX_POINT('',#30325);
#7183=VERTEX_POINT('',#30396);
#7184=VERTEX_POINT('',#30431);
#7185=VERTEX_POINT('',#30436);
#7186=VERTEX_POINT('',#30454);
#7187=VERTEX_POINT('',#30459);
#7188=VERTEX_POINT('',#30473);
#7189=VERTEX_POINT('',#30478);
#7190=VERTEX_POINT('',#30483);
#7191=VERTEX_POINT('',#30501);
#7192=VERTEX_POINT('',#30506);
#7193=VERTEX_POINT('',#30520);
#7194=VERTEX_POINT('',#30542);
#7195=VERTEX_POINT('',#30577);
#7196=VERTEX_POINT('',#30586);
#7197=VERTEX_POINT('',#30596);
#7198=VERTEX_POINT('',#30613);
#7199=VERTEX_POINT('',#30643);
#7200=VERTEX_POINT('',#30658);
#7201=VERTEX_POINT('',#30697);
#7202=VERTEX_POINT('',#30712);
#7203=VERTEX_POINT('',#30751);
#7204=VERTEX_POINT('',#30766);
#7205=VERTEX_POINT('',#30805);
#7206=VERTEX_POINT('',#30820);
#7207=VERTEX_POINT('',#30859);
#7208=VERTEX_POINT('',#30874);
#7209=VERTEX_POINT('',#30913);
#7210=VERTEX_POINT('',#30928);
#7211=VERTEX_POINT('',#30964);
#7212=VERTEX_POINT('',#30980);
#7213=VERTEX_POINT('',#30997);
#7214=VERTEX_POINT('',#31013);
#7215=VERTEX_POINT('',#31030);
#7216=VERTEX_POINT('',#31046);
#7217=VERTEX_POINT('',#31063);
#7218=VERTEX_POINT('',#31079);
#7219=VERTEX_POINT('',#31121);
#7220=VERTEX_POINT('',#31137);
#7221=VERTEX_POINT('',#31179);
#7222=VERTEX_POINT('',#31194);
#7223=VERTEX_POINT('',#31196);
#7224=VERTEX_POINT('',#31235);
#7225=VERTEX_POINT('',#31246);
#7226=VERTEX_POINT('',#31272);
#7227=VERTEX_POINT('',#31281);
#7228=VERTEX_POINT('',#31304);
#7229=VERTEX_POINT('',#31310);
#7230=VERTEX_POINT('',#31323);
#7231=VERTEX_POINT('',#31355);
#7232=VERTEX_POINT('',#31374);
#7233=VERTEX_POINT('',#31380);
#7234=VERTEX_POINT('',#31394);
#7235=VERTEX_POINT('',#31396);
#7236=VERTEX_POINT('',#31414);
#7237=VERTEX_POINT('',#31420);
#7238=VERTEX_POINT('',#31434);
#7239=VERTEX_POINT('',#31436);
#7240=VERTEX_POINT('',#31454);
#7241=VERTEX_POINT('',#31462);
#7242=VERTEX_POINT('',#31479);
#7243=VERTEX_POINT('',#31505);
#7244=VERTEX_POINT('',#31510);
#7245=VERTEX_POINT('',#31518);
#7246=VERTEX_POINT('',#31535);
#7247=VERTEX_POINT('',#31537);
#7248=VERTEX_POINT('',#31539);
#7249=VERTEX_POINT('',#31568);
#7250=VERTEX_POINT('',#31591);
#7251=VERTEX_POINT('',#31608);
#7252=VERTEX_POINT('',#31625);
#7253=VERTEX_POINT('',#31786);
#7254=VERTEX_POINT('',#31840);
#7255=VERTEX_POINT('',#31857);
#7256=VERTEX_POINT('',#31874);
#7257=VERTEX_POINT('',#31897);
#7258=VERTEX_POINT('',#31907);
#7259=VERTEX_POINT('',#31909);
#7260=VERTEX_POINT('',#31911);
#7261=VERTEX_POINT('',#31913);
#7262=VERTEX_POINT('',#31921);
#7263=VERTEX_POINT('',#31926);
#7264=VERTEX_POINT('',#31931);
#7265=VERTEX_POINT('',#31957);
#7266=VERTEX_POINT('',#31971);
#7267=VERTEX_POINT('',#31994);
#7268=VERTEX_POINT('',#32014);
#7269=VERTEX_POINT('',#32028);
#7270=VERTEX_POINT('',#32057);
#7271=VERTEX_POINT('',#32065);
#7272=VERTEX_POINT('',#32076);
#7273=VERTEX_POINT('',#32078);
#7274=VERTEX_POINT('',#32080);
#7275=VERTEX_POINT('',#32088);
#7276=VERTEX_POINT('',#32108);
#7277=VERTEX_POINT('',#32283);
#7278=VERTEX_POINT('',#32284);
#7279=VERTEX_POINT('',#32286);
#7280=VERTEX_POINT('',#32293);
#7281=VERTEX_POINT('',#32313);
#7282=VERTEX_POINT('',#32315);
#7283=VERTEX_POINT('',#32383);
#7284=VERTEX_POINT('',#32384);
#7285=VERTEX_POINT('',#32386);
#7286=VERTEX_POINT('',#32408);
#7287=VERTEX_POINT('',#32430);
#7288=VERTEX_POINT('',#32432);
#7289=VERTEX_POINT('',#32475);
#7290=VERTEX_POINT('',#32476);
#7291=VERTEX_POINT('',#32478);
#7292=VERTEX_POINT('',#32500);
#7293=VERTEX_POINT('',#32522);
#7294=VERTEX_POINT('',#32524);
#7295=VERTEX_POINT('',#32604);
#7296=VERTEX_POINT('',#32605);
#7297=VERTEX_POINT('',#32607);
#7298=VERTEX_POINT('',#32629);
#7299=VERTEX_POINT('',#32651);
#7300=VERTEX_POINT('',#32653);
#7301=VERTEX_POINT('',#32733);
#7302=VERTEX_POINT('',#32734);
#7303=VERTEX_POINT('',#32736);
#7304=VERTEX_POINT('',#32756);
#7305=VERTEX_POINT('',#32776);
#7306=VERTEX_POINT('',#32778);
#7307=VERTEX_POINT('',#32883);
#7308=VERTEX_POINT('',#32884);
#7309=VERTEX_POINT('',#32886);
#7310=VERTEX_POINT('',#32908);
#7311=VERTEX_POINT('',#32930);
#7312=VERTEX_POINT('',#32932);
#7313=VERTEX_POINT('',#33049);
#7314=VERTEX_POINT('',#33050);
#7315=VERTEX_POINT('',#33052);
#7316=VERTEX_POINT('',#33065);
#7317=VERTEX_POINT('',#33077);
#7318=VERTEX_POINT('',#33089);
#7319=VERTEX_POINT('',#33103);
#7320=VERTEX_POINT('',#33105);
#7321=VERTEX_POINT('',#33118);
#7322=VERTEX_POINT('',#33130);
#7323=VERTEX_POINT('',#33154);
#7324=VERTEX_POINT('',#33155);
#7325=VERTEX_POINT('',#33157);
#7326=VERTEX_POINT('',#33179);
#7327=VERTEX_POINT('',#33201);
#7328=VERTEX_POINT('',#33203);
#7329=VERTEX_POINT('',#33320);
#7330=VERTEX_POINT('',#33321);
#7331=VERTEX_POINT('',#33323);
#7332=VERTEX_POINT('',#33343);
#7333=VERTEX_POINT('',#33363);
#7334=VERTEX_POINT('',#33365);
#7335=VERTEX_POINT('',#33470);
#7336=VERTEX_POINT('',#33471);
#7337=VERTEX_POINT('',#33473);
#7338=VERTEX_POINT('',#33493);
#7339=VERTEX_POINT('',#33513);
#7340=VERTEX_POINT('',#33515);
#7341=VERTEX_POINT('',#33620);
#7342=VERTEX_POINT('',#33621);
#7343=VERTEX_POINT('',#33623);
#7344=VERTEX_POINT('',#33643);
#7345=VERTEX_POINT('',#33663);
#7346=VERTEX_POINT('',#33665);
#7347=VERTEX_POINT('',#33770);
#7348=VERTEX_POINT('',#33771);
#7349=VERTEX_POINT('',#33773);
#7350=VERTEX_POINT('',#33793);
#7351=VERTEX_POINT('',#33813);
#7352=VERTEX_POINT('',#33815);
#7353=VERTEX_POINT('',#33920);
#7354=VERTEX_POINT('',#33921);
#7355=VERTEX_POINT('',#33923);
#7356=VERTEX_POINT('',#33936);
#7357=VERTEX_POINT('',#33948);
#7358=VERTEX_POINT('',#33960);
#7359=VERTEX_POINT('',#33974);
#7360=VERTEX_POINT('',#33976);
#7361=VERTEX_POINT('',#33989);
#7362=VERTEX_POINT('',#34001);
#7363=VERTEX_POINT('',#34025);
#7364=VERTEX_POINT('',#34026);
#7365=VERTEX_POINT('',#34058);
#7366=VERTEX_POINT('',#34072);
#7367=VERTEX_POINT('',#34084);
#7368=VERTEX_POINT('',#34096);
#7369=VERTEX_POINT('',#34109);
#7370=VERTEX_POINT('',#34141);
#7371=VERTEX_POINT('',#34154);
#7372=VERTEX_POINT('',#34167);
#7373=VERTEX_POINT('',#34191);
#7374=VERTEX_POINT('',#34192);
#7375=VERTEX_POINT('',#34202);
#7376=VERTEX_POINT('',#34211);
#7377=VERTEX_POINT('',#34243);
#7378=VERTEX_POINT('',#34269);
#7379=VERTEX_POINT('',#34298);
#7380=VERTEX_POINT('',#34324);
#7381=VERTEX_POINT('',#34353);
#7382=VERTEX_POINT('',#34373);
#7383=VERTEX_POINT('',#34378);
#7384=VERTEX_POINT('',#34407);
#7385=VERTEX_POINT('',#34482);
#7386=VERTEX_POINT('',#34483);
#7387=VERTEX_POINT('',#34485);
#7388=VERTEX_POINT('',#34505);
#7389=VERTEX_POINT('',#34525);
#7390=VERTEX_POINT('',#34527);
#7391=VERTEX_POINT('',#34556);
#7392=VERTEX_POINT('',#34582);
#7393=VERTEX_POINT('',#34636);
#7394=VERTEX_POINT('',#34637);
#7395=VERTEX_POINT('',#34732);
#7396=VERTEX_POINT('',#34741);
#7397=VERTEX_POINT('',#34751);
#7398=VERTEX_POINT('',#34768);
#7399=VERTEX_POINT('',#34788);
#7400=VERTEX_POINT('',#34814);
#7401=VERTEX_POINT('',#34819);
#7402=VERTEX_POINT('',#34872);
#7403=VERTEX_POINT('',#34882);
#7404=VERTEX_POINT('',#35096);
#7405=VERTEX_POINT('',#35101);
#7406=VERTEX_POINT('',#35113);
#7407=VERTEX_POINT('',#35125);
#7408=VERTEX_POINT('',#35126);
#7409=VERTEX_POINT('',#35131);
#7410=VERTEX_POINT('',#35133);
#7411=VERTEX_POINT('',#35138);
#7412=VERTEX_POINT('',#35145);
#7413=VERTEX_POINT('',#35146);
#7414=VERTEX_POINT('',#35148);
#7415=VERTEX_POINT('',#35153);
#7416=VERTEX_POINT('',#35158);
#7417=VERTEX_POINT('',#35165);
#7418=VERTEX_POINT('',#35166);
#7419=VERTEX_POINT('',#35168);
#7420=VERTEX_POINT('',#35173);
#7421=VERTEX_POINT('',#35178);
#7422=VERTEX_POINT('',#35196);
#7423=VERTEX_POINT('',#35197);
#7424=VERTEX_POINT('',#35202);
#7425=VERTEX_POINT('',#35204);
#7426=VERTEX_POINT('',#35209);
#7427=VERTEX_POINT('',#35216);
#7428=VERTEX_POINT('',#35385);
#7429=VERTEX_POINT('',#35387);
#7430=VERTEX_POINT('',#35410);
#7431=VERTEX_POINT('',#35433);
#7432=VERTEX_POINT('',#35460);
#7433=VERTEX_POINT('',#35462);
#7434=VERTEX_POINT('',#35470);
#7435=VERTEX_POINT('',#35511);
#7436=VERTEX_POINT('',#35573);
#7437=VERTEX_POINT('',#35602);
#7438=VERTEX_POINT('',#35610);
#7439=VERTEX_POINT('',#35612);
#7440=VERTEX_POINT('',#35620);
#7441=VERTEX_POINT('',#35705);
#7442=VERTEX_POINT('',#35710);
#7443=VERTEX_POINT('',#35715);
#7444=VERTEX_POINT('',#35726);
#7445=VERTEX_POINT('',#35731);
#7446=VERTEX_POINT('',#35742);
#7447=VERTEX_POINT('',#35752);
#7448=VERTEX_POINT('',#35788);
#7449=VERTEX_POINT('',#35822);
#7450=VERTEX_POINT('',#35858);
#7451=VERTEX_POINT('',#35892);
#7452=VERTEX_POINT('',#35897);
#7453=VERTEX_POINT('',#35902);
#7454=VERTEX_POINT('',#35907);
#7455=VERTEX_POINT('',#35912);
#7456=VERTEX_POINT('',#35914);
#7457=VERTEX_POINT('',#35924);
#7458=VERTEX_POINT('',#35925);
#7459=VERTEX_POINT('',#35927);
#7460=VERTEX_POINT('',#35933);
#7461=VERTEX_POINT('',#35938);
#7462=VERTEX_POINT('',#35943);
#7463=VERTEX_POINT('',#35951);
#7464=VERTEX_POINT('',#35979);
#7465=VERTEX_POINT('',#35990);
#7466=VERTEX_POINT('',#36010);
#7467=VERTEX_POINT('',#36027);
#7468=VERTEX_POINT('',#36053);
#7469=VERTEX_POINT('',#36067);
#7470=VERTEX_POINT('',#36069);
#7471=VERTEX_POINT('',#36080);
#7472=VERTEX_POINT('',#36103);
#7473=VERTEX_POINT('',#36120);
#7474=VERTEX_POINT('',#36163);
#7475=VERTEX_POINT('',#36164);
#7476=VERTEX_POINT('',#36166);
#7477=VERTEX_POINT('',#36177);
#7478=VERTEX_POINT('',#36197);
#7479=VERTEX_POINT('',#36214);
#7480=VERTEX_POINT('',#36253);
#7481=VERTEX_POINT('',#36264);
#7482=VERTEX_POINT('',#36287);
#7483=VERTEX_POINT('',#36304);
#7484=VERTEX_POINT('',#36347);
#7485=VERTEX_POINT('',#36353);
#7486=VERTEX_POINT('',#36358);
#7487=VERTEX_POINT('',#36396);
#7488=VERTEX_POINT('',#36404);
#7489=VERTEX_POINT('',#36438);
#7490=VERTEX_POINT('',#36446);
#7491=VERTEX_POINT('',#36468);
#7492=VERTEX_POINT('',#36469);
#7493=VERTEX_POINT('',#36486);
#7494=VERTEX_POINT('',#36494);
#7495=VERTEX_POINT('',#37292);
#7496=VERTEX_POINT('',#37303);
#7497=VERTEX_POINT('',#37310);
#7498=VERTEX_POINT('',#37312);
#7499=VERTEX_POINT('',#37319);
#7500=VERTEX_POINT('',#37321);
#7501=VERTEX_POINT('',#37335);
#7502=VERTEX_POINT('',#37336);
#7503=VERTEX_POINT('',#37354);
#7504=VERTEX_POINT('',#37363);
#7505=VERTEX_POINT('',#37368);
#7506=VERTEX_POINT('',#37386);
#7507=VERTEX_POINT('',#37409);
#7508=VERTEX_POINT('',#37410);
#7509=VERTEX_POINT('',#37428);
#7510=VERTEX_POINT('',#37450);
#7511=VERTEX_POINT('',#37455);
#7512=VERTEX_POINT('',#37473);
#7513=VERTEX_POINT('',#37498);
#7514=VERTEX_POINT('',#37499);
#7515=VERTEX_POINT('',#37549);
#7516=VERTEX_POINT('',#37569);
#7517=VERTEX_POINT('',#37574);
#7518=VERTEX_POINT('',#37594);
#7519=VERTEX_POINT('',#37649);
#7520=VERTEX_POINT('',#37650);
#7521=VERTEX_POINT('',#37700);
#7522=VERTEX_POINT('',#37720);
#7523=VERTEX_POINT('',#37725);
#7524=VERTEX_POINT('',#37775);
#7525=VERTEX_POINT('',#37845);
#7526=VERTEX_POINT('',#37846);
#7527=VERTEX_POINT('',#37864);
#7528=VERTEX_POINT('',#37885);
#7529=VERTEX_POINT('',#37890);
#7530=VERTEX_POINT('',#37909);
#7531=VERTEX_POINT('',#37932);
#7532=VERTEX_POINT('',#37933);
#7533=VERTEX_POINT('',#37953);
#7534=VERTEX_POINT('',#37974);
#7535=VERTEX_POINT('',#37979);
#7536=VERTEX_POINT('',#38032);
#7537=VERTEX_POINT('',#38087);
#7538=VERTEX_POINT('',#38088);
#7539=VERTEX_POINT('',#38107);
#7540=VERTEX_POINT('',#38128);
#7541=VERTEX_POINT('',#38133);
#7542=VERTEX_POINT('',#38154);
#7543=VERTEX_POINT('',#38178);
#7544=VERTEX_POINT('',#38179);
#7545=VERTEX_POINT('',#38199);
#7546=VERTEX_POINT('',#38224);
#7547=VERTEX_POINT('',#38229);
#7548=VERTEX_POINT('',#38279);
#7549=VERTEX_POINT('',#38334);
#7550=VERTEX_POINT('',#38335);
#7551=VERTEX_POINT('',#38353);
#7552=VERTEX_POINT('',#38374);
#7553=VERTEX_POINT('',#38379);
#7554=VERTEX_POINT('',#38399);
#7555=VERTEX_POINT('',#38422);
#7556=VERTEX_POINT('',#38423);
#7557=VERTEX_POINT('',#38441);
#7558=VERTEX_POINT('',#38461);
#7559=VERTEX_POINT('',#38466);
#7560=VERTEX_POINT('',#38485);
#7561=VERTEX_POINT('',#38508);
#7562=VERTEX_POINT('',#38509);
#7563=VERTEX_POINT('',#38527);
#7564=VERTEX_POINT('',#38548);
#7565=VERTEX_POINT('',#38553);
#7566=VERTEX_POINT('',#38573);
#7567=VERTEX_POINT('',#38596);
#7568=VERTEX_POINT('',#38597);
#7569=VERTEX_POINT('',#38615);
#7570=VERTEX_POINT('',#38636);
#7571=VERTEX_POINT('',#38641);
#7572=VERTEX_POINT('',#38660);
#7573=VERTEX_POINT('',#38683);
#7574=VERTEX_POINT('',#38684);
#7575=VERTEX_POINT('',#38703);
#7576=VERTEX_POINT('',#38725);
#7577=VERTEX_POINT('',#38730);
#7578=VERTEX_POINT('',#38752);
#7579=VERTEX_POINT('',#38776);
#7580=VERTEX_POINT('',#38777);
#7581=VERTEX_POINT('',#38795);
#7582=VERTEX_POINT('',#38817);
#7583=VERTEX_POINT('',#38827);
#7584=VERTEX_POINT('',#38848);
#7585=VERTEX_POINT('',#38893);
#7586=VERTEX_POINT('',#38894);
#7587=VERTEX_POINT('',#38912);
#7588=VERTEX_POINT('',#38931);
#7589=VERTEX_POINT('',#38954);
#7590=VERTEX_POINT('',#38963);
#7591=VERTEX_POINT('',#38990);
#7592=VERTEX_POINT('',#38991);
#7593=VERTEX_POINT('',#39009);
#7594=VERTEX_POINT('',#39030);
#7595=VERTEX_POINT('',#39035);
#7596=VERTEX_POINT('',#39053);
#7597=VERTEX_POINT('',#39076);
#7598=VERTEX_POINT('',#39077);
#7599=VERTEX_POINT('',#39086);
#7600=VERTEX_POINT('',#39106);
#7601=VERTEX_POINT('',#39115);
#7602=VERTEX_POINT('',#39122);
#7603=VERTEX_POINT('',#39173);
#7604=VERTEX_POINT('',#39174);
#7605=VERTEX_POINT('',#39192);
#7606=VERTEX_POINT('',#39201);
#7607=VERTEX_POINT('',#39206);
#7608=VERTEX_POINT('',#39224);
#7609=VERTEX_POINT('',#39247);
#7610=VERTEX_POINT('',#39248);
#7611=VERTEX_POINT('',#39266);
#7612=VERTEX_POINT('',#39286);
#7613=VERTEX_POINT('',#39291);
#7614=VERTEX_POINT('',#39311);
#7615=VERTEX_POINT('',#39334);
#7616=VERTEX_POINT('',#39335);
#7617=VERTEX_POINT('',#39385);
#7618=VERTEX_POINT('',#39405);
#7619=VERTEX_POINT('',#39410);
#7620=VERTEX_POINT('',#39460);
#7621=VERTEX_POINT('',#39483);
#7622=VERTEX_POINT('',#39484);
#7623=VERTEX_POINT('',#39534);
#7624=VERTEX_POINT('',#39554);
#7625=VERTEX_POINT('',#39559);
#7626=VERTEX_POINT('',#39609);
#7627=VERTEX_POINT('',#39664);
#7628=VERTEX_POINT('',#39665);
#7629=VERTEX_POINT('',#39683);
#7630=VERTEX_POINT('',#39701);
#7631=VERTEX_POINT('',#39708);
#7632=VERTEX_POINT('',#39726);
#7633=VERTEX_POINT('',#39749);
#7634=VERTEX_POINT('',#39750);
#7635=VERTEX_POINT('',#39770);
#7636=VERTEX_POINT('',#39790);
#7637=VERTEX_POINT('',#39795);
#7638=VERTEX_POINT('',#39845);
#7639=VERTEX_POINT('',#39900);
#7640=VERTEX_POINT('',#39901);
#7641=VERTEX_POINT('',#39920);
#7642=VERTEX_POINT('',#39939);
#7643=VERTEX_POINT('',#39944);
#7644=VERTEX_POINT('',#39963);
#7645=VERTEX_POINT('',#39987);
#7646=VERTEX_POINT('',#39988);
#7647=VERTEX_POINT('',#40008);
#7648=VERTEX_POINT('',#40028);
#7649=VERTEX_POINT('',#40033);
#7650=VERTEX_POINT('',#40083);
#7651=VERTEX_POINT('',#40138);
#7652=VERTEX_POINT('',#40139);
#7653=VERTEX_POINT('',#40157);
#7654=VERTEX_POINT('',#40208);
#7655=VERTEX_POINT('',#40213);
#7656=VERTEX_POINT('',#40231);
#7657=VERTEX_POINT('',#40254);
#7658=VERTEX_POINT('',#40255);
#7659=VERTEX_POINT('',#40273);
#7660=VERTEX_POINT('',#40320);
#7661=VERTEX_POINT('',#40325);
#7662=VERTEX_POINT('',#40343);
#7663=VERTEX_POINT('',#40366);
#7664=VERTEX_POINT('',#40367);
#7665=VERTEX_POINT('',#40385);
#7666=VERTEX_POINT('',#40403);
#7667=VERTEX_POINT('',#40408);
#7668=VERTEX_POINT('',#40426);
#7669=VERTEX_POINT('',#40449);
#7670=VERTEX_POINT('',#40450);
#7671=VERTEX_POINT('',#40468);
#7672=VERTEX_POINT('',#40486);
#7673=VERTEX_POINT('',#40491);
#7674=VERTEX_POINT('',#40509);
#7675=VERTEX_POINT('',#40532);
#7676=VERTEX_POINT('',#40533);
#7677=VERTEX_POINT('',#40552);
#7678=VERTEX_POINT('',#40571);
#7679=VERTEX_POINT('',#40576);
#7680=VERTEX_POINT('',#40595);
#7681=VERTEX_POINT('',#40619);
#7682=VERTEX_POINT('',#40620);
#7683=VERTEX_POINT('',#40638);
#7684=VERTEX_POINT('',#40656);
#7685=VERTEX_POINT('',#40682);
#7686=VERTEX_POINT('',#40701);
#7687=VERTEX_POINT('',#40729);
#7688=VERTEX_POINT('',#40730);
#7689=VERTEX_POINT('',#40748);
#7690=VERTEX_POINT('',#40768);
#7691=VERTEX_POINT('',#40775);
#7692=VERTEX_POINT('',#40784);
#7693=VERTEX_POINT('',#40825);
#7694=VERTEX_POINT('',#40826);
#7695=VERTEX_POINT('',#40844);
#7696=VERTEX_POINT('',#40862);
#7697=VERTEX_POINT('',#40867);
#7698=VERTEX_POINT('',#40885);
#7699=VERTEX_POINT('',#40908);
#7700=VERTEX_POINT('',#40909);
#7701=VERTEX_POINT('',#40929);
#7702=VERTEX_POINT('',#40947);
#7703=VERTEX_POINT('',#40956);
#7704=VERTEX_POINT('',#40976);
#7705=VERTEX_POINT('',#47233);
#7706=VERTEX_POINT('',#47234);
#7707=VERTEX_POINT('',#47238);
#7708=VERTEX_POINT('',#47250);
#7709=VERTEX_POINT('',#47254);
#7710=VERTEX_POINT('',#47317);
#7711=VERTEX_POINT('',#47318);
#7712=VERTEX_POINT('',#47322);
#7713=VERTEX_POINT('',#47336);
#7714=VERTEX_POINT('',#47359);
#7715=VERTEX_POINT('',#47370);
#7716=VERTEX_POINT('',#47387);
#7717=VERTEX_POINT('',#47410);
#7718=VERTEX_POINT('',#47418);
#7719=VERTEX_POINT('',#47492);
#7720=VERTEX_POINT('',#47493);
#7721=VERTEX_POINT('',#47497);
#7722=VERTEX_POINT('',#47516);
#7723=VERTEX_POINT('',#47518);
#7724=VERTEX_POINT('',#47539);
#7725=VERTEX_POINT('',#47568);
#7726=VERTEX_POINT('',#47599);
#7727=VERTEX_POINT('',#47622);
#7728=VERTEX_POINT('',#47624);
#7729=VERTEX_POINT('',#47628);
#7730=VERTEX_POINT('',#47633);
#7731=VERTEX_POINT('',#47641);
#7732=VERTEX_POINT('',#47646);
#7733=VERTEX_POINT('',#47651);
#7734=VERTEX_POINT('',#47664);
#7735=VERTEX_POINT('',#47666);
#7736=VERTEX_POINT('',#47667);
#7737=VERTEX_POINT('',#47669);
#7738=VERTEX_POINT('',#47671);
#7739=VERTEX_POINT('',#47673);
#7740=VERTEX_POINT('',#47675);
#7741=VERTEX_POINT('',#47677);
#7742=VERTEX_POINT('',#47679);
#7743=VERTEX_POINT('',#47683);
#7744=VERTEX_POINT('',#47687);
#7745=VERTEX_POINT('',#47690);
#7746=VERTEX_POINT('',#47691);
#7747=VERTEX_POINT('',#47693);
#7748=VERTEX_POINT('',#47695);
#7749=VERTEX_POINT('',#47697);
#7750=VERTEX_POINT('',#47699);
#7751=VERTEX_POINT('',#47701);
#7752=VERTEX_POINT('',#47703);
#7753=VERTEX_POINT('',#47706);
#7754=VERTEX_POINT('',#47729);
#7755=VERTEX_POINT('',#47731);
#7756=VERTEX_POINT('',#47735);
#7757=VERTEX_POINT('',#47737);
#7758=VERTEX_POINT('',#47742);
#7759=VERTEX_POINT('',#47744);
#7760=VERTEX_POINT('',#47748);
#7761=VERTEX_POINT('',#47764);
#7762=VERTEX_POINT('',#47765);
#7763=VERTEX_POINT('',#47768);
#7764=VERTEX_POINT('',#47784);
#7765=VERTEX_POINT('',#47793);
#7766=VERTEX_POINT('',#47794);
#7767=VERTEX_POINT('',#47802);
#7768=VERTEX_POINT('',#47822);
#7769=VERTEX_POINT('',#47833);
#7770=VERTEX_POINT('',#47841);
#7771=VERTEX_POINT('',#47869);
#7772=VERTEX_POINT('',#47986);
#7773=VERTEX_POINT('',#47987);
#7774=VERTEX_POINT('',#47989);
#7775=VERTEX_POINT('',#47991);
#7776=VERTEX_POINT('',#47993);
#7777=VERTEX_POINT('',#47995);
#7778=VERTEX_POINT('',#47997);
#7779=VERTEX_POINT('',#47999);
#7780=VERTEX_POINT('',#48001);
#7781=VERTEX_POINT('',#48003);
#7782=VERTEX_POINT('',#48005);
#7783=VERTEX_POINT('',#48007);
#7784=VERTEX_POINT('',#48009);
#7785=VERTEX_POINT('',#48011);
#7786=VERTEX_POINT('',#48013);
#7787=VERTEX_POINT('',#48015);
#7788=VERTEX_POINT('',#48017);
#7789=VERTEX_POINT('',#48020);
#7790=VERTEX_POINT('',#48023);
#7791=VERTEX_POINT('',#48024);
#7792=VERTEX_POINT('',#48026);
#7793=VERTEX_POINT('',#48028);
#7794=VERTEX_POINT('',#48030);
#7795=VERTEX_POINT('',#48032);
#7796=VERTEX_POINT('',#48034);
#7797=VERTEX_POINT('',#48036);
#7798=VERTEX_POINT('',#48038);
#7799=VERTEX_POINT('',#48040);
#7800=VERTEX_POINT('',#48042);
#7801=VERTEX_POINT('',#48044);
#7802=VERTEX_POINT('',#48046);
#7803=VERTEX_POINT('',#48048);
#7804=VERTEX_POINT('',#48050);
#7805=VERTEX_POINT('',#48052);
#7806=VERTEX_POINT('',#48054);
#7807=VERTEX_POINT('',#48057);
#7808=VERTEX_POINT('',#48060);
#7809=VERTEX_POINT('',#48061);
#7810=VERTEX_POINT('',#48063);
#7811=VERTEX_POINT('',#48065);
#7812=VERTEX_POINT('',#48069);
#7813=VERTEX_POINT('',#48070);
#7814=VERTEX_POINT('',#48075);
#7815=VERTEX_POINT('',#48076);
#7816=VERTEX_POINT('',#48081);
#7817=VERTEX_POINT('',#48082);
#7818=VERTEX_POINT('',#48087);
#7819=VERTEX_POINT('',#48088);
#7820=VERTEX_POINT('',#48093);
#7821=VERTEX_POINT('',#48094);
#7822=VERTEX_POINT('',#48099);
#7823=VERTEX_POINT('',#48100);
#7824=VERTEX_POINT('',#48105);
#7825=VERTEX_POINT('',#48106);
#7826=VERTEX_POINT('',#48111);
#7827=VERTEX_POINT('',#48112);
#7828=VERTEX_POINT('',#48117);
#7829=VERTEX_POINT('',#48118);
#7830=VERTEX_POINT('',#48120);
#7831=VERTEX_POINT('',#48122);
#7832=VERTEX_POINT('',#48126);
#7833=VERTEX_POINT('',#48127);
#7834=VERTEX_POINT('',#48129);
#7835=VERTEX_POINT('',#48131);
#7836=VERTEX_POINT('',#48135);
#7837=VERTEX_POINT('',#48136);
#7838=VERTEX_POINT('',#48141);
#7839=VERTEX_POINT('',#48142);
#7840=VERTEX_POINT('',#48147);
#7841=VERTEX_POINT('',#48148);
#7842=VERTEX_POINT('',#48156);
#7843=VERTEX_POINT('',#48157);
#7844=VERTEX_POINT('',#48160);
#7845=VERTEX_POINT('',#48243);
#7846=VERTEX_POINT('',#48244);
#7847=VERTEX_POINT('',#48246);
#7848=VERTEX_POINT('',#48248);
#7849=VERTEX_POINT('',#48252);
#7850=VERTEX_POINT('',#48253);
#7851=VERTEX_POINT('',#48255);
#7852=VERTEX_POINT('',#48257);
#7853=VERTEX_POINT('',#48261);
#7854=VERTEX_POINT('',#48262);
#7855=VERTEX_POINT('',#48264);
#7856=VERTEX_POINT('',#48266);
#7857=VERTEX_POINT('',#48270);
#7858=VERTEX_POINT('',#48271);
#7859=VERTEX_POINT('',#48276);
#7860=VERTEX_POINT('',#48277);
#7861=VERTEX_POINT('',#48282);
#7862=VERTEX_POINT('',#48283);
#7863=VERTEX_POINT('',#48288);
#7864=VERTEX_POINT('',#48289);
#7865=VERTEX_POINT('',#48294);
#7866=VERTEX_POINT('',#48295);
#7867=VERTEX_POINT('',#48300);
#7868=VERTEX_POINT('',#48301);
#7869=VERTEX_POINT('',#48306);
#7870=VERTEX_POINT('',#48307);
#7871=VERTEX_POINT('',#48312);
#7872=VERTEX_POINT('',#48313);
#7873=VERTEX_POINT('',#48318);
#7874=VERTEX_POINT('',#48319);
#7875=VERTEX_POINT('',#48324);
#7876=VERTEX_POINT('',#48325);
#7877=VERTEX_POINT('',#48330);
#7878=VERTEX_POINT('',#48331);
#7879=VERTEX_POINT('',#48336);
#7880=VERTEX_POINT('',#48337);
#7881=VERTEX_POINT('',#48339);
#7882=VERTEX_POINT('',#48341);
#7883=VERTEX_POINT('',#48345);
#7884=VERTEX_POINT('',#48346);
#7885=VERTEX_POINT('',#48348);
#7886=VERTEX_POINT('',#48350);
#7887=VERTEX_POINT('',#48352);
#7888=VERTEX_POINT('',#48354);
#7889=VERTEX_POINT('',#48356);
#7890=VERTEX_POINT('',#48358);
#7891=VERTEX_POINT('',#48360);
#7892=VERTEX_POINT('',#48362);
#7893=VERTEX_POINT('',#48364);
#7894=VERTEX_POINT('',#48366);
#7895=VERTEX_POINT('',#48368);
#7896=VERTEX_POINT('',#48370);
#7897=VERTEX_POINT('',#48372);
#7898=VERTEX_POINT('',#48374);
#7899=VERTEX_POINT('',#48376);
#7900=VERTEX_POINT('',#48378);
#7901=VERTEX_POINT('',#48381);
#7902=VERTEX_POINT('',#48384);
#7903=VERTEX_POINT('',#48385);
#7904=VERTEX_POINT('',#48387);
#7905=VERTEX_POINT('',#48389);
#7906=VERTEX_POINT('',#48391);
#7907=VERTEX_POINT('',#48393);
#7908=VERTEX_POINT('',#48395);
#7909=VERTEX_POINT('',#48397);
#7910=VERTEX_POINT('',#48399);
#7911=VERTEX_POINT('',#48401);
#7912=VERTEX_POINT('',#48403);
#7913=VERTEX_POINT('',#48405);
#7914=VERTEX_POINT('',#48407);
#7915=VERTEX_POINT('',#48409);
#7916=VERTEX_POINT('',#48411);
#7917=VERTEX_POINT('',#48413);
#7918=VERTEX_POINT('',#48415);
#7919=VERTEX_POINT('',#48417);
#7920=VERTEX_POINT('',#48420);
#7921=VERTEX_POINT('',#48423);
#7922=VERTEX_POINT('',#48424);
#7923=VERTEX_POINT('',#48427);
#7924=VERTEX_POINT('',#48524);
#7925=VERTEX_POINT('',#48526);
#7926=VERTEX_POINT('',#48531);
#7927=VERTEX_POINT('',#48532);
#7928=VERTEX_POINT('',#48534);
#7929=VERTEX_POINT('',#48536);
#7930=VERTEX_POINT('',#48540);
#7931=VERTEX_POINT('',#48542);
#7932=VERTEX_POINT('',#48546);
#7933=VERTEX_POINT('',#48548);
#7934=VERTEX_POINT('',#48558);
#7935=VERTEX_POINT('',#48560);
#7936=VERTEX_POINT('',#48563);
#7937=VERTEX_POINT('',#48564);
#7938=VERTEX_POINT('',#48567);
#7939=VERTEX_POINT('',#48571);
#7940=VERTEX_POINT('',#48573);
#7941=VERTEX_POINT('',#48583);
#7942=VERTEX_POINT('',#48584);
#7943=VERTEX_POINT('',#48586);
#7944=VERTEX_POINT('',#48588);
#7945=VERTEX_POINT('',#48590);
#7946=VERTEX_POINT('',#48592);
#7947=VERTEX_POINT('',#48594);
#7948=VERTEX_POINT('',#48596);
#7949=VERTEX_POINT('',#48598);
#7950=VERTEX_POINT('',#48600);
#7951=VERTEX_POINT('',#48602);
#7952=VERTEX_POINT('',#48604);
#7953=VERTEX_POINT('',#48606);
#7954=VERTEX_POINT('',#48608);
#7955=VERTEX_POINT('',#48610);
#7956=VERTEX_POINT('',#48613);
#7957=VERTEX_POINT('',#48615);
#7958=VERTEX_POINT('',#48617);
#7959=VERTEX_POINT('',#48619);
#7960=VERTEX_POINT('',#48621);
#7961=VERTEX_POINT('',#48623);
#7962=VERTEX_POINT('',#48625);
#7963=VERTEX_POINT('',#48627);
#7964=VERTEX_POINT('',#48631);
#7965=VERTEX_POINT('',#48633);
#7966=VERTEX_POINT('',#48638);
#7967=VERTEX_POINT('',#48641);
#7968=VERTEX_POINT('',#48643);
#7969=VERTEX_POINT('',#48649);
#7970=VERTEX_POINT('',#48651);
#7971=VERTEX_POINT('',#48655);
#7972=VERTEX_POINT('',#48659);
#7973=VERTEX_POINT('',#48663);
#7974=VERTEX_POINT('',#48667);
#7975=VERTEX_POINT('',#48671);
#7976=VERTEX_POINT('',#48675);
#7977=VERTEX_POINT('',#48679);
#7978=VERTEX_POINT('',#48683);
#7979=VERTEX_POINT('',#48687);
#7980=VERTEX_POINT('',#48691);
#7981=VERTEX_POINT('',#48695);
#7982=VERTEX_POINT('',#48699);
#7983=VERTEX_POINT('',#48703);
#7984=VERTEX_POINT('',#48707);
#7985=VERTEX_POINT('',#48711);
#7986=VERTEX_POINT('',#48715);
#7987=VERTEX_POINT('',#48719);
#7988=VERTEX_POINT('',#48723);
#7989=VERTEX_POINT('',#48733);
#7990=VERTEX_POINT('',#48734);
#7991=VERTEX_POINT('',#48736);
#7992=VERTEX_POINT('',#48738);
#7993=VERTEX_POINT('',#48745);
#7994=VERTEX_POINT('',#48746);
#7995=VERTEX_POINT('',#48749);
#7996=VERTEX_POINT('',#48751);
#7997=VERTEX_POINT('',#48753);
#7998=VERTEX_POINT('',#48755);
#7999=VERTEX_POINT('',#48758);
#8000=VERTEX_POINT('',#48759);
#8001=VERTEX_POINT('',#48762);
#8002=VERTEX_POINT('',#48764);
#8003=VERTEX_POINT('',#48766);
#8004=VERTEX_POINT('',#48768);
#8005=VERTEX_POINT('',#48771);
#8006=VERTEX_POINT('',#48772);
#8007=VERTEX_POINT('',#48775);
#8008=VERTEX_POINT('',#48777);
#8009=VERTEX_POINT('',#48781);
#8010=VERTEX_POINT('',#48782);
#8011=VERTEX_POINT('',#48785);
#8012=VERTEX_POINT('',#48787);
#8013=VERTEX_POINT('',#48791);
#8014=VERTEX_POINT('',#48792);
#8015=VERTEX_POINT('',#48795);
#8016=VERTEX_POINT('',#48797);
#8017=VERTEX_POINT('',#48801);
#8018=VERTEX_POINT('',#48802);
#8019=VERTEX_POINT('',#48805);
#8020=VERTEX_POINT('',#48807);
#8021=VERTEX_POINT('',#48888);
#8022=VERTEX_POINT('',#48889);
#8023=VERTEX_POINT('',#48891);
#8024=VERTEX_POINT('',#48893);
#8025=VERTEX_POINT('',#48897);
#8026=VERTEX_POINT('',#48898);
#8027=VERTEX_POINT('',#48900);
#8028=VERTEX_POINT('',#48902);
#8029=VERTEX_POINT('',#48906);
#8030=VERTEX_POINT('',#48907);
#8031=VERTEX_POINT('',#48909);
#8032=VERTEX_POINT('',#48911);
#8033=VERTEX_POINT('',#48915);
#8034=VERTEX_POINT('',#48917);
#8035=VERTEX_POINT('',#48921);
#8036=VERTEX_POINT('',#48923);
#8037=VERTEX_POINT('',#48927);
#8038=VERTEX_POINT('',#48928);
#8039=VERTEX_POINT('',#48930);
#8040=VERTEX_POINT('',#48932);
#8041=VERTEX_POINT('',#48936);
#8042=VERTEX_POINT('',#48937);
#8043=VERTEX_POINT('',#48939);
#8044=VERTEX_POINT('',#48941);
#8045=VERTEX_POINT('',#48948);
#8046=VERTEX_POINT('',#48949);
#8047=VERTEX_POINT('',#48954);
#8048=VERTEX_POINT('',#48965);
#8049=VERTEX_POINT('',#48967);
#8050=VERTEX_POINT('',#48969);
#8051=VERTEX_POINT('',#48971);
#8052=VERTEX_POINT('',#48973);
#8053=VERTEX_POINT('',#48975);
#8054=VERTEX_POINT('',#48977);
#8055=VERTEX_POINT('',#48980);
#8056=VERTEX_POINT('',#48983);
#8057=VERTEX_POINT('',#48984);
#8058=VERTEX_POINT('',#48986);
#8059=VERTEX_POINT('',#48988);
#8060=VERTEX_POINT('',#48993);
#8061=VERTEX_POINT('',#49004);
#8062=VERTEX_POINT('',#49006);
#8063=VERTEX_POINT('',#49008);
#8064=VERTEX_POINT('',#49010);
#8065=VERTEX_POINT('',#49012);
#8066=VERTEX_POINT('',#49015);
#8067=VERTEX_POINT('',#49018);
#8068=VERTEX_POINT('',#49019);
#8069=VERTEX_POINT('',#49022);
#8070=VERTEX_POINT('',#49024);
#8071=VERTEX_POINT('',#49091);
#8072=VERTEX_POINT('',#49101);
#8073=VERTEX_POINT('',#49165);
#8074=VERTEX_POINT('',#49166);
#8075=VERTEX_POINT('',#49170);
#8076=VERTEX_POINT('',#49182);
#8077=VERTEX_POINT('',#49186);
#8078=VERTEX_POINT('',#49191);
#8079=VERTEX_POINT('',#49197);
#8080=VERTEX_POINT('',#49203);
#8081=VERTEX_POINT('',#49209);
#8082=VERTEX_POINT('',#49215);
#8083=VERTEX_POINT('',#49258);
#8084=VERTEX_POINT('',#49259);
#8085=VERTEX_POINT('',#49263);
#8086=VERTEX_POINT('',#49275);
#8087=VERTEX_POINT('',#49279);
#8088=VERTEX_POINT('',#49284);
#8089=VERTEX_POINT('',#49290);
#8090=VERTEX_POINT('',#49296);
#8091=VERTEX_POINT('',#49302);
#8092=VERTEX_POINT('',#49308);
#8093=VERTEX_POINT('',#49351);
#8094=VERTEX_POINT('',#49352);
#8095=VERTEX_POINT('',#49356);
#8096=VERTEX_POINT('',#49368);
#8097=VERTEX_POINT('',#49372);
#8098=VERTEX_POINT('',#49377);
#8099=VERTEX_POINT('',#49383);
#8100=VERTEX_POINT('',#49389);
#8101=VERTEX_POINT('',#49395);
#8102=VERTEX_POINT('',#49401);
#8103=VERTEX_POINT('',#49444);
#8104=VERTEX_POINT('',#49445);
#8105=VERTEX_POINT('',#49449);
#8106=VERTEX_POINT('',#49461);
#8107=VERTEX_POINT('',#49465);
#8108=VERTEX_POINT('',#49470);
#8109=VERTEX_POINT('',#49476);
#8110=VERTEX_POINT('',#49482);
#8111=VERTEX_POINT('',#49488);
#8112=VERTEX_POINT('',#49494);
#8113=VERTEX_POINT('',#49537);
#8114=VERTEX_POINT('',#49538);
#8115=VERTEX_POINT('',#49542);
#8116=VERTEX_POINT('',#49554);
#8117=VERTEX_POINT('',#49558);
#8118=VERTEX_POINT('',#49563);
#8119=VERTEX_POINT('',#49569);
#8120=VERTEX_POINT('',#49575);
#8121=VERTEX_POINT('',#49581);
#8122=VERTEX_POINT('',#49587);
#8123=VERTEX_POINT('',#49598);
#8124=VERTEX_POINT('',#49599);
#8125=VERTEX_POINT('',#49604);
#8126=VERTEX_POINT('',#49606);
#8127=VERTEX_POINT('',#49608);
#8128=VERTEX_POINT('',#49610);
#8129=VERTEX_POINT('',#49614);
#8130=VERTEX_POINT('',#49616);
#8131=VERTEX_POINT('',#49620);
#8132=VERTEX_POINT('',#49621);
#8133=VERTEX_POINT('',#49623);
#8134=VERTEX_POINT('',#49625);
#8135=VERTEX_POINT('',#49629);
#8136=VERTEX_POINT('',#49630);
#8137=VERTEX_POINT('',#49632);
#8138=VERTEX_POINT('',#49634);
#8139=VERTEX_POINT('',#49638);
#8140=VERTEX_POINT('',#49639);
#8141=VERTEX_POINT('',#49641);
#8142=VERTEX_POINT('',#49643);
#8143=VERTEX_POINT('',#49645);
#8144=VERTEX_POINT('',#49647);
#8145=VERTEX_POINT('',#49649);
#8146=VERTEX_POINT('',#49651);
#8147=VERTEX_POINT('',#49653);
#8148=VERTEX_POINT('',#49655);
#8149=VERTEX_POINT('',#49658);
#8150=VERTEX_POINT('',#49660);
#8151=VERTEX_POINT('',#49662);
#8152=VERTEX_POINT('',#49664);
#8153=VERTEX_POINT('',#49667);
#8154=VERTEX_POINT('',#49674);
#8155=VERTEX_POINT('',#49676);
#8156=VERTEX_POINT('',#49678);
#8157=VERTEX_POINT('',#49691);
#8158=VERTEX_POINT('',#49692);
#8159=VERTEX_POINT('',#49694);
#8160=VERTEX_POINT('',#49696);
#8161=VERTEX_POINT('',#49700);
#8162=VERTEX_POINT('',#49701);
#8163=VERTEX_POINT('',#49715);
#8164=VERTEX_POINT('',#49717);
#8165=VERTEX_POINT('',#49719);
#8166=VERTEX_POINT('',#49733);
#8167=VERTEX_POINT('',#49735);
#8168=VERTEX_POINT('',#49737);
#8169=VERTEX_POINT('',#49762);
#8170=VERTEX_POINT('',#49763);
#8171=VERTEX_POINT('',#49765);
#8172=VERTEX_POINT('',#49767);
#8173=VERTEX_POINT('',#49771);
#8174=VERTEX_POINT('',#49772);
#8175=VERTEX_POINT('',#49777);
#8176=VERTEX_POINT('',#49778);
#8177=VERTEX_POINT('',#49780);
#8178=VERTEX_POINT('',#49782);
#8179=VERTEX_POINT('',#49786);
#8180=VERTEX_POINT('',#49788);
#8181=VERTEX_POINT('',#49795);
#8182=VERTEX_POINT('',#49796);
#8183=VERTEX_POINT('',#49798);
#8184=VERTEX_POINT('',#49800);
#8185=VERTEX_POINT('',#49802);
#8186=VERTEX_POINT('',#49804);
#8187=VERTEX_POINT('',#49806);
#8188=VERTEX_POINT('',#49808);
#8189=VERTEX_POINT('',#49810);
#8190=VERTEX_POINT('',#49812);
#8191=VERTEX_POINT('',#49815);
#8192=VERTEX_POINT('',#49817);
#8193=VERTEX_POINT('',#49819);
#8194=VERTEX_POINT('',#49822);
#8195=VERTEX_POINT('',#49823);
#8196=VERTEX_POINT('',#49831);
#8197=VERTEX_POINT('',#49836);
#8198=VERTEX_POINT('',#49838);
#8199=VERTEX_POINT('',#49840);
#8200=VERTEX_POINT('',#49842);
#8201=VERTEX_POINT('',#49844);
#8202=VERTEX_POINT('',#49846);
#8203=VERTEX_POINT('',#49848);
#8204=VERTEX_POINT('',#49850);
#8205=VERTEX_POINT('',#49855);
#8206=VERTEX_POINT('',#49876);
#8207=VERTEX_POINT('',#49877);
#8208=VERTEX_POINT('',#49881);
#8209=VERTEX_POINT('',#49882);
#8210=VERTEX_POINT('',#49884);
#8211=VERTEX_POINT('',#49886);
#8212=VERTEX_POINT('',#49893);
#8213=VERTEX_POINT('',#49894);
#8214=VERTEX_POINT('',#49896);
#8215=VERTEX_POINT('',#49898);
#8216=VERTEX_POINT('',#49900);
#8217=VERTEX_POINT('',#49902);
#8218=VERTEX_POINT('',#49904);
#8219=VERTEX_POINT('',#49907);
#8220=VERTEX_POINT('',#49909);
#8221=VERTEX_POINT('',#49911);
#8222=VERTEX_POINT('',#49915);
#8223=VERTEX_POINT('',#49917);
#8224=VERTEX_POINT('',#49920);
#8225=VERTEX_POINT('',#49921);
#8226=VERTEX_POINT('',#49924);
#8227=VERTEX_POINT('',#49926);
#8228=VERTEX_POINT('',#49930);
#8229=VERTEX_POINT('',#49931);
#8230=VERTEX_POINT('',#49933);
#8231=VERTEX_POINT('',#49950);
#8232=VERTEX_POINT('',#49967);
#8233=VERTEX_POINT('',#49969);
#8234=VERTEX_POINT('',#49984);
#8235=VERTEX_POINT('',#49986);
#8236=VERTEX_POINT('',#49990);
#8237=VERTEX_POINT('',#49992);
#8238=VERTEX_POINT('',#50006);
#8239=VERTEX_POINT('',#50008);
#8240=VERTEX_POINT('',#50013);
#8241=VERTEX_POINT('',#50018);
#8242=VERTEX_POINT('',#50035);
#8243=VERTEX_POINT('',#50037);
#8244=VERTEX_POINT('',#50039);
#8245=VERTEX_POINT('',#50070);
#8246=VERTEX_POINT('',#50081);
#8247=VERTEX_POINT('',#50137);
#8248=VERTEX_POINT('',#50205);
#8249=VERTEX_POINT('',#50356);
#8250=VERTEX_POINT('',#50357);
#8251=VERTEX_POINT('',#50471);
#8252=VERTEX_POINT('',#50509);
#8253=VERTEX_POINT('',#50660);
#8254=VERTEX_POINT('',#50661);
#8255=VERTEX_POINT('',#50666);
#8256=VERTEX_POINT('',#50668);
#8257=VERTEX_POINT('',#50796);
#8258=VERTEX_POINT('',#50931);
#8259=VERTEX_POINT('',#50932);
#8260=VERTEX_POINT('',#50934);
#8261=VERTEX_POINT('',#50960);
#8262=VERTEX_POINT('',#51037);
#8263=VERTEX_POINT('',#51063);
#8264=VERTEX_POINT('',#51125);
#8265=VERTEX_POINT('',#51126);
#8266=VERTEX_POINT('',#51350);
#8267=VERTEX_POINT('',#51378);
#8268=VERTEX_POINT('',#51379);
#8269=VERTEX_POINT('',#51381);
#8270=VERTEX_POINT('',#51383);
#8271=VERTEX_POINT('',#51387);
#8272=VERTEX_POINT('',#51391);
#8273=VERTEX_POINT('',#51395);
#8274=VERTEX_POINT('',#51396);
#8275=VERTEX_POINT('',#51404);
#8276=VERTEX_POINT('',#51451);
#8277=VERTEX_POINT('',#51465);
#8278=VERTEX_POINT('',#51515);
#8279=VERTEX_POINT('',#51523);
#8280=VERTEX_POINT('',#51528);
#8281=VERTEX_POINT('',#51530);
#8282=VERTEX_POINT('',#51532);
#8283=VERTEX_POINT('',#51534);
#8284=VERTEX_POINT('',#51536);
#8285=VERTEX_POINT('',#51542);
#8286=VERTEX_POINT('',#51544);
#8287=VERTEX_POINT('',#51546);
#8288=VERTEX_POINT('',#51549);
#8289=VERTEX_POINT('',#51550);
#8290=VERTEX_POINT('',#51552);
#8291=VERTEX_POINT('',#51554);
#8292=VERTEX_POINT('',#51558);
#8293=VERTEX_POINT('',#51559);
#8294=VERTEX_POINT('',#51564);
#8295=VERTEX_POINT('',#51566);
#8296=VERTEX_POINT('',#51722);
#8297=VERTEX_POINT('',#51724);
#8298=VERTEX_POINT('',#51795);
#8299=VERTEX_POINT('',#51957);
#8300=VERTEX_POINT('',#52155);
#8301=VERTEX_POINT('',#52163);
#8302=VERTEX_POINT('',#52457);
#8303=VERTEX_POINT('',#52466);
#8304=VERTEX_POINT('',#52474);
#8305=VERTEX_POINT('',#52602);
#8306=VERTEX_POINT('',#52677);
#8307=VERTEX_POINT('',#52857);
#8308=VERTEX_POINT('',#52880);
#8309=VERTEX_POINT('',#53071);
#8310=VERTEX_POINT('',#53176);
#8311=VERTEX_POINT('',#53184);
#8312=VERTEX_POINT('',#53279);
#8313=VERTEX_POINT('',#53299);
#8314=VERTEX_POINT('',#53387);
#8315=VERTEX_POINT('',#53392);
#8316=VERTEX_POINT('',#53504);
#8317=VERTEX_POINT('',#53533);
#8318=VERTEX_POINT('',#53685);
#8319=VERTEX_POINT('',#53792);
#8320=VERTEX_POINT('',#53881);
#8321=VERTEX_POINT('',#53992);
#8322=VERTEX_POINT('',#54522);
#8323=VERTEX_POINT('',#54524);
#8324=VERTEX_POINT('',#54527);
#8325=VERTEX_POINT('',#54530);
#8326=EDGE_CURVE('',#6526,#6527,#5623,.T.);
#8327=EDGE_CURVE('',#6528,#6526,#5624,.T.);
#8328=EDGE_CURVE('',#6529,#6528,#5625,.T.);
#8329=EDGE_CURVE('',#6530,#6529,#5626,.T.);
#8330=EDGE_CURVE('',#6531,#6530,#5627,.T.);
#8331=EDGE_CURVE('',#6532,#6531,#5628,.T.);
#8332=EDGE_CURVE('',#6533,#6532,#5629,.T.);
#8333=EDGE_CURVE('',#6534,#6533,#5630,.T.);
#8334=EDGE_CURVE('',#6535,#6534,#5631,.T.);
#8335=EDGE_CURVE('',#6536,#6535,#5632,.T.);
#8336=EDGE_CURVE('',#6537,#6536,#5633,.T.);
#8337=EDGE_CURVE('',#6538,#6537,#5634,.T.);
#8338=EDGE_CURVE('',#6539,#6538,#5635,.T.);
#8339=EDGE_CURVE('',#6540,#6539,#5636,.T.);
#8340=EDGE_CURVE('',#6541,#6540,#5637,.T.);
#8341=EDGE_CURVE('',#6542,#6541,#5638,.T.);
#8342=EDGE_CURVE('',#6543,#6542,#5639,.T.);
#8343=EDGE_CURVE('',#6544,#6543,#5640,.T.);
#8344=EDGE_CURVE('',#6545,#6544,#5641,.T.);
#8345=EDGE_CURVE('',#6546,#6545,#5642,.T.);
#8346=EDGE_CURVE('',#6547,#6546,#5643,.T.);
#8347=EDGE_CURVE('',#6548,#6547,#5644,.T.);
#8348=EDGE_CURVE('',#6549,#6548,#5645,.T.);
#8349=EDGE_CURVE('',#6550,#6549,#5646,.T.);
#8350=EDGE_CURVE('',#6551,#6550,#5647,.T.);
#8351=EDGE_CURVE('',#6552,#6551,#5648,.T.);
#8352=EDGE_CURVE('',#6553,#6552,#5649,.T.);
#8353=EDGE_CURVE('',#6554,#6553,#5650,.T.);
#8354=EDGE_CURVE('',#6555,#6554,#5651,.T.);
#8355=EDGE_CURVE('',#6556,#6555,#5652,.T.);
#8356=EDGE_CURVE('',#6557,#6556,#5653,.T.);
#8357=EDGE_CURVE('',#6558,#6557,#5654,.T.);
#8358=EDGE_CURVE('',#6559,#6558,#5655,.T.);
#8359=EDGE_CURVE('',#6560,#6559,#5656,.T.);
#8360=EDGE_CURVE('',#6561,#6560,#5657,.T.);
#8361=EDGE_CURVE('',#6562,#6561,#5658,.T.);
#8362=EDGE_CURVE('',#6563,#6562,#5659,.T.);
#8363=EDGE_CURVE('',#6564,#6563,#5660,.T.);
#8364=EDGE_CURVE('',#6565,#6564,#5661,.T.);
#8365=EDGE_CURVE('',#6566,#6565,#5662,.T.);
#8366=EDGE_CURVE('',#6567,#6566,#5663,.T.);
#8367=EDGE_CURVE('',#6568,#6567,#5664,.T.);
#8368=EDGE_CURVE('',#6569,#6568,#5665,.T.);
#8369=EDGE_CURVE('',#6570,#6569,#5666,.T.);
#8370=EDGE_CURVE('',#6571,#6570,#5667,.T.);
#8371=EDGE_CURVE('',#6572,#6571,#5668,.T.);
#8372=EDGE_CURVE('',#6573,#6572,#5669,.T.);
#8373=EDGE_CURVE('',#6574,#6573,#5670,.T.);
#8374=EDGE_CURVE('',#6575,#6574,#5671,.T.);
#8375=EDGE_CURVE('',#6576,#6575,#5672,.T.);
#8376=EDGE_CURVE('',#6577,#6576,#5673,.T.);
#8377=EDGE_CURVE('',#6578,#6577,#5674,.T.);
#8378=EDGE_CURVE('',#6579,#6578,#5675,.T.);
#8379=EDGE_CURVE('',#6580,#6579,#5676,.T.);
#8380=EDGE_CURVE('',#6581,#6580,#5677,.T.);
#8381=EDGE_CURVE('',#6582,#6581,#5678,.T.);
#8382=EDGE_CURVE('',#6583,#6582,#5679,.T.);
#8383=EDGE_CURVE('',#6584,#6583,#5680,.T.);
#8384=EDGE_CURVE('',#6585,#6584,#5681,.T.);
#8385=EDGE_CURVE('',#6586,#6585,#5682,.T.);
#8386=EDGE_CURVE('',#6587,#6586,#5683,.T.);
#8387=EDGE_CURVE('',#6588,#6587,#5684,.T.);
#8388=EDGE_CURVE('',#6589,#6588,#5685,.T.);
#8389=EDGE_CURVE('',#6590,#6589,#5686,.T.);
#8390=EDGE_CURVE('',#6591,#6590,#5687,.T.);
#8391=EDGE_CURVE('',#6592,#6591,#5688,.T.);
#8392=EDGE_CURVE('',#6593,#6592,#5689,.T.);
#8393=EDGE_CURVE('',#6594,#6593,#5690,.T.);
#8394=EDGE_CURVE('',#6595,#6594,#5691,.T.);
#8395=EDGE_CURVE('',#6596,#6595,#5692,.T.);
#8396=EDGE_CURVE('',#6597,#6596,#5693,.T.);
#8397=EDGE_CURVE('',#6598,#6597,#5694,.T.);
#8398=EDGE_CURVE('',#6599,#6598,#5695,.T.);
#8399=EDGE_CURVE('',#6600,#6599,#5696,.T.);
#8400=EDGE_CURVE('',#6601,#6600,#5697,.T.);
#8401=EDGE_CURVE('',#6602,#6601,#5698,.T.);
#8402=EDGE_CURVE('',#6603,#6602,#5699,.T.);
#8403=EDGE_CURVE('',#6604,#6603,#5700,.T.);
#8404=EDGE_CURVE('',#6605,#6604,#5701,.T.);
#8405=EDGE_CURVE('',#6606,#6605,#5702,.T.);
#8406=EDGE_CURVE('',#6607,#6606,#5703,.T.);
#8407=EDGE_CURVE('',#6608,#6607,#5704,.T.);
#8408=EDGE_CURVE('',#6609,#6608,#5705,.T.);
#8409=EDGE_CURVE('',#6610,#6609,#5706,.T.);
#8410=EDGE_CURVE('',#6611,#6610,#5707,.T.);
#8411=EDGE_CURVE('',#6612,#6611,#5708,.T.);
#8412=EDGE_CURVE('',#6613,#6612,#5709,.T.);
#8413=EDGE_CURVE('',#6614,#6613,#5710,.T.);
#8414=EDGE_CURVE('',#6615,#6614,#5711,.T.);
#8415=EDGE_CURVE('',#6616,#6615,#5712,.T.);
#8416=EDGE_CURVE('',#6617,#6616,#5713,.T.);
#8417=EDGE_CURVE('',#6618,#6617,#5714,.T.);
#8418=EDGE_CURVE('',#6619,#6618,#5715,.T.);
#8419=EDGE_CURVE('',#6620,#6619,#5716,.T.);
#8420=EDGE_CURVE('',#6621,#6620,#5717,.T.);
#8421=EDGE_CURVE('',#6622,#6621,#5718,.T.);
#8422=EDGE_CURVE('',#6623,#6622,#5719,.T.);
#8423=EDGE_CURVE('',#6624,#6623,#5720,.T.);
#8424=EDGE_CURVE('',#6625,#6624,#5721,.T.);
#8425=EDGE_CURVE('',#6626,#6625,#5722,.T.);
#8426=EDGE_CURVE('',#6627,#6626,#5723,.T.);
#8427=EDGE_CURVE('',#6628,#6627,#5724,.T.);
#8428=EDGE_CURVE('',#6629,#6628,#5725,.T.);
#8429=EDGE_CURVE('',#6630,#6629,#5726,.T.);
#8430=EDGE_CURVE('',#6631,#6630,#5727,.T.);
#8431=EDGE_CURVE('',#6632,#6631,#5728,.T.);
#8432=EDGE_CURVE('',#6633,#6632,#5729,.T.);
#8433=EDGE_CURVE('',#6634,#6633,#5730,.T.);
#8434=EDGE_CURVE('',#6635,#6634,#5731,.T.);
#8435=EDGE_CURVE('',#6636,#6635,#5732,.T.);
#8436=EDGE_CURVE('',#6637,#6636,#5733,.T.);
#8437=EDGE_CURVE('',#6638,#6637,#5734,.T.);
#8438=EDGE_CURVE('',#6639,#6638,#5735,.T.);
#8439=EDGE_CURVE('',#6640,#6639,#5736,.T.);
#8440=EDGE_CURVE('',#6641,#6640,#5737,.T.);
#8441=EDGE_CURVE('',#6642,#6641,#5738,.T.);
#8442=EDGE_CURVE('',#6643,#6642,#5739,.T.);
#8443=EDGE_CURVE('',#6644,#6643,#5740,.T.);
#8444=EDGE_CURVE('',#6645,#6644,#5741,.T.);
#8445=EDGE_CURVE('',#6646,#6645,#5742,.T.);
#8446=EDGE_CURVE('',#6647,#6646,#5743,.T.);
#8447=EDGE_CURVE('',#6648,#6647,#5744,.T.);
#8448=EDGE_CURVE('',#6649,#6648,#5745,.T.);
#8449=EDGE_CURVE('',#6650,#6649,#5746,.T.);
#8450=EDGE_CURVE('',#6651,#6650,#5747,.T.);
#8451=EDGE_CURVE('',#6652,#6651,#5748,.T.);
#8452=EDGE_CURVE('',#6653,#6652,#5749,.T.);
#8453=EDGE_CURVE('',#6654,#6653,#5750,.T.);
#8454=EDGE_CURVE('',#6655,#6654,#5751,.T.);
#8455=EDGE_CURVE('',#6656,#6655,#5752,.T.);
#8456=EDGE_CURVE('',#6657,#6656,#5753,.T.);
#8457=EDGE_CURVE('',#6658,#6657,#5754,.T.);
#8458=EDGE_CURVE('',#6659,#6658,#5755,.T.);
#8459=EDGE_CURVE('',#6660,#6659,#5756,.T.);
#8460=EDGE_CURVE('',#6661,#6660,#5757,.T.);
#8461=EDGE_CURVE('',#6662,#6661,#5758,.T.);
#8462=EDGE_CURVE('',#6663,#6662,#5759,.T.);
#8463=EDGE_CURVE('',#6664,#6663,#5760,.T.);
#8464=EDGE_CURVE('',#6665,#6664,#5761,.T.);
#8465=EDGE_CURVE('',#6666,#6665,#5762,.T.);
#8466=EDGE_CURVE('',#6667,#6666,#5763,.T.);
#8467=EDGE_CURVE('',#6668,#6667,#5764,.T.);
#8468=EDGE_CURVE('',#6669,#6668,#5765,.T.);
#8469=EDGE_CURVE('',#6670,#6669,#5766,.T.);
#8470=EDGE_CURVE('',#6671,#6670,#5767,.T.);
#8471=EDGE_CURVE('',#6672,#6671,#5768,.T.);
#8472=EDGE_CURVE('',#6673,#6672,#5769,.T.);
#8473=EDGE_CURVE('',#6674,#6673,#5770,.T.);
#8474=EDGE_CURVE('',#6675,#6674,#5771,.T.);
#8475=EDGE_CURVE('',#6676,#6675,#5772,.T.);
#8476=EDGE_CURVE('',#6677,#6676,#5773,.T.);
#8477=EDGE_CURVE('',#6678,#6677,#5774,.T.);
#8478=EDGE_CURVE('',#6679,#6678,#5775,.T.);
#8479=EDGE_CURVE('',#6680,#6679,#5776,.T.);
#8480=EDGE_CURVE('',#6681,#6680,#5777,.T.);
#8481=EDGE_CURVE('',#6682,#6681,#5778,.T.);
#8482=EDGE_CURVE('',#6683,#6682,#5779,.T.);
#8483=EDGE_CURVE('',#6684,#6683,#5780,.T.);
#8484=EDGE_CURVE('',#6685,#6684,#5781,.T.);
#8485=EDGE_CURVE('',#6686,#6685,#5782,.T.);
#8486=EDGE_CURVE('',#6687,#6686,#5783,.T.);
#8487=EDGE_CURVE('',#6688,#6687,#5784,.T.);
#8488=EDGE_CURVE('',#6689,#6688,#5785,.T.);
#8489=EDGE_CURVE('',#6690,#6689,#5786,.T.);
#8490=EDGE_CURVE('',#6691,#6690,#5787,.T.);
#8491=EDGE_CURVE('',#6692,#6691,#5788,.T.);
#8492=EDGE_CURVE('',#6693,#6692,#5789,.T.);
#8493=EDGE_CURVE('',#6694,#6693,#5790,.T.);
#8494=EDGE_CURVE('',#6695,#6694,#5791,.T.);
#8495=EDGE_CURVE('',#6696,#6695,#5792,.T.);
#8496=EDGE_CURVE('',#6697,#6696,#5793,.T.);
#8497=EDGE_CURVE('',#6698,#6697,#5794,.T.);
#8498=EDGE_CURVE('',#6699,#6698,#5795,.T.);
#8499=EDGE_CURVE('',#6700,#6699,#5796,.T.);
#8500=EDGE_CURVE('',#6701,#6700,#5797,.T.);
#8501=EDGE_CURVE('',#6702,#6701,#5798,.T.);
#8502=EDGE_CURVE('',#6703,#6702,#5799,.T.);
#8503=EDGE_CURVE('',#6704,#6703,#5800,.T.);
#8504=EDGE_CURVE('',#6705,#6704,#5801,.T.);
#8505=EDGE_CURVE('',#6706,#6705,#5802,.T.);
#8506=EDGE_CURVE('',#6707,#6706,#5803,.T.);
#8507=EDGE_CURVE('',#6708,#6707,#5804,.T.);
#8508=EDGE_CURVE('',#6709,#6708,#5805,.T.);
#8509=EDGE_CURVE('',#6527,#6709,#5806,.T.);
#8510=EDGE_CURVE('',#6710,#6710,#5807,.F.);
#8511=EDGE_CURVE('',#6527,#6711,#1815,.T.);
#8512=EDGE_CURVE('',#6712,#6709,#1816,.F.);
#8513=EDGE_CURVE('',#6711,#6712,#5808,.T.);
#8514=EDGE_CURVE('',#6713,#6529,#1817,.F.);
#8515=EDGE_CURVE('',#6714,#6713,#5809,.T.);
#8516=EDGE_CURVE('',#6530,#6714,#1818,.T.);
#8517=EDGE_CURVE('',#6706,#6715,#1819,.T.);
#8518=EDGE_CURVE('',#6716,#6705,#1820,.F.);
#8519=EDGE_CURVE('',#6715,#6716,#5810,.T.);
#8520=EDGE_CURVE('',#6702,#6717,#1821,.T.);
#8521=EDGE_CURVE('',#6718,#6701,#1822,.F.);
#8522=EDGE_CURVE('',#6717,#6718,#5811,.T.);
#8523=EDGE_CURVE('',#6690,#6719,#1823,.T.);
#8524=EDGE_CURVE('',#6720,#6689,#1824,.F.);
#8525=EDGE_CURVE('',#6719,#6720,#5812,.T.);
#8526=EDGE_CURVE('',#6721,#6693,#1825,.F.);
#8527=EDGE_CURVE('',#6722,#6721,#5813,.T.);
#8528=EDGE_CURVE('',#6694,#6722,#1826,.T.);
#8529=EDGE_CURVE('',#6723,#6697,#1827,.F.);
#8530=EDGE_CURVE('',#6724,#6723,#5814,.T.);
#8531=EDGE_CURVE('',#6698,#6724,#1828,.T.);
#8532=EDGE_CURVE('',#6678,#6725,#1829,.T.);
#8533=EDGE_CURVE('',#6726,#6677,#1830,.F.);
#8534=EDGE_CURVE('',#6725,#6726,#5815,.T.);
#8535=EDGE_CURVE('',#6727,#6681,#1831,.F.);
#8536=EDGE_CURVE('',#6728,#6727,#5816,.T.);
#8537=EDGE_CURVE('',#6682,#6728,#1832,.T.);
#8538=EDGE_CURVE('',#6686,#6729,#1833,.T.);
#8539=EDGE_CURVE('',#6730,#6685,#1834,.F.);
#8540=EDGE_CURVE('',#6729,#6730,#5817,.T.);
#8541=EDGE_CURVE('',#6674,#6731,#1835,.T.);
#8542=EDGE_CURVE('',#6732,#6673,#1836,.F.);
#8543=EDGE_CURVE('',#6731,#6732,#5818,.T.);
#8544=EDGE_CURVE('',#6670,#6733,#1837,.T.);
#8545=EDGE_CURVE('',#6734,#6669,#1838,.F.);
#8546=EDGE_CURVE('',#6733,#6734,#5819,.T.);
#8547=EDGE_CURVE('',#6570,#6735,#1839,.T.);
#8548=EDGE_CURVE('',#6736,#6569,#1840,.F.);
#8549=EDGE_CURVE('',#6735,#6736,#5820,.T.);
#8550=EDGE_CURVE('',#6737,#6573,#1841,.F.);
#8551=EDGE_CURVE('',#6738,#6737,#5821,.T.);
#8552=EDGE_CURVE('',#6574,#6738,#1842,.T.);
#8553=EDGE_CURVE('',#6566,#6739,#1843,.T.);
#8554=EDGE_CURVE('',#6740,#6565,#1844,.F.);
#8555=EDGE_CURVE('',#6739,#6740,#5822,.T.);
#8556=EDGE_CURVE('',#6562,#6741,#1845,.T.);
#8557=EDGE_CURVE('',#6742,#6561,#1846,.F.);
#8558=EDGE_CURVE('',#6741,#6742,#5823,.T.);
#8559=EDGE_CURVE('',#6550,#6743,#1847,.T.);
#8560=EDGE_CURVE('',#6744,#6549,#1848,.F.);
#8561=EDGE_CURVE('',#6743,#6744,#5824,.T.);
#8562=EDGE_CURVE('',#6745,#6553,#1849,.F.);
#8563=EDGE_CURVE('',#6746,#6745,#5825,.T.);
#8564=EDGE_CURVE('',#6554,#6746,#1850,.T.);
#8565=EDGE_CURVE('',#6747,#6557,#1851,.F.);
#8566=EDGE_CURVE('',#6748,#6747,#5826,.T.);
#8567=EDGE_CURVE('',#6558,#6748,#1852,.T.);
#8568=EDGE_CURVE('',#6538,#6749,#1853,.T.);
#8569=EDGE_CURVE('',#6750,#6537,#1854,.F.);
#8570=EDGE_CURVE('',#6749,#6750,#5827,.T.);
#8571=EDGE_CURVE('',#6751,#6541,#1855,.F.);
#8572=EDGE_CURVE('',#6752,#6751,#5828,.T.);
#8573=EDGE_CURVE('',#6542,#6752,#1856,.T.);
#8574=EDGE_CURVE('',#6546,#6753,#1857,.T.);
#8575=EDGE_CURVE('',#6754,#6545,#1858,.F.);
#8576=EDGE_CURVE('',#6753,#6754,#5829,.T.);
#8577=EDGE_CURVE('',#6534,#6755,#1859,.T.);
#8578=EDGE_CURVE('',#6756,#6533,#1860,.F.);
#8579=EDGE_CURVE('',#6755,#6756,#5830,.T.);
#8580=EDGE_CURVE('',#6614,#6757,#1861,.T.);
#8581=EDGE_CURVE('',#6758,#6613,#1862,.F.);
#8582=EDGE_CURVE('',#6757,#6758,#5831,.T.);
#8583=EDGE_CURVE('',#6759,#6617,#1863,.F.);
#8584=EDGE_CURVE('',#6760,#6759,#5832,.T.);
#8585=EDGE_CURVE('',#6618,#6760,#1864,.T.);
#8586=EDGE_CURVE('',#6610,#6761,#1865,.T.);
#8587=EDGE_CURVE('',#6762,#6609,#1866,.F.);
#8588=EDGE_CURVE('',#6761,#6762,#5833,.T.);
#8589=EDGE_CURVE('',#6606,#6763,#1867,.T.);
#8590=EDGE_CURVE('',#6764,#6605,#1868,.F.);
#8591=EDGE_CURVE('',#6763,#6764,#5834,.T.);
#8592=EDGE_CURVE('',#6594,#6765,#1869,.T.);
#8593=EDGE_CURVE('',#6766,#6593,#1870,.F.);
#8594=EDGE_CURVE('',#6765,#6766,#5835,.T.);
#8595=EDGE_CURVE('',#6767,#6597,#1871,.F.);
#8596=EDGE_CURVE('',#6768,#6767,#5836,.T.);
#8597=EDGE_CURVE('',#6598,#6768,#1872,.T.);
#8598=EDGE_CURVE('',#6602,#6769,#1873,.T.);
#8599=EDGE_CURVE('',#6770,#6601,#1874,.F.);
#8600=EDGE_CURVE('',#6769,#6770,#5837,.T.);
#8601=EDGE_CURVE('',#6586,#6771,#1875,.T.);
#8602=EDGE_CURVE('',#6772,#6585,#1876,.F.);
#8603=EDGE_CURVE('',#6771,#6772,#5838,.T.);
#8604=EDGE_CURVE('',#6773,#6589,#1877,.F.);
#8605=EDGE_CURVE('',#6774,#6773,#5839,.T.);
#8606=EDGE_CURVE('',#6590,#6774,#1878,.T.);
#8607=EDGE_CURVE('',#6582,#6775,#1879,.T.);
#8608=EDGE_CURVE('',#6776,#6581,#1880,.F.);
#8609=EDGE_CURVE('',#6775,#6776,#5840,.T.);
#8610=EDGE_CURVE('',#6578,#6777,#1881,.T.);
#8611=EDGE_CURVE('',#6778,#6577,#1882,.F.);
#8612=EDGE_CURVE('',#6777,#6778,#5841,.T.);
#8613=EDGE_CURVE('',#6658,#6779,#1883,.T.);
#8614=EDGE_CURVE('',#6780,#6657,#1884,.F.);
#8615=EDGE_CURVE('',#6779,#6780,#5842,.T.);
#8616=EDGE_CURVE('',#6781,#6661,#1885,.F.);
#8617=EDGE_CURVE('',#6782,#6781,#5843,.T.);
#8618=EDGE_CURVE('',#6662,#6782,#1886,.T.);
#8619=EDGE_CURVE('',#6654,#6783,#1887,.T.);
#8620=EDGE_CURVE('',#6784,#6653,#1888,.F.);
#8621=EDGE_CURVE('',#6783,#6784,#5844,.T.);
#8622=EDGE_CURVE('',#6650,#6785,#1889,.T.);
#8623=EDGE_CURVE('',#6786,#6649,#1890,.F.);
#8624=EDGE_CURVE('',#6785,#6786,#5845,.T.);
#8625=EDGE_CURVE('',#6638,#6787,#1891,.T.);
#8626=EDGE_CURVE('',#6788,#6637,#1892,.F.);
#8627=EDGE_CURVE('',#6787,#6788,#5846,.T.);
#8628=EDGE_CURVE('',#6789,#6641,#1893,.F.);
#8629=EDGE_CURVE('',#6790,#6789,#5847,.T.);
#8630=EDGE_CURVE('',#6642,#6790,#1894,.T.);
#8631=EDGE_CURVE('',#6646,#6791,#1895,.T.);
#8632=EDGE_CURVE('',#6792,#6645,#1896,.F.);
#8633=EDGE_CURVE('',#6791,#6792,#5848,.T.);
#8634=EDGE_CURVE('',#6630,#6793,#1897,.T.);
#8635=EDGE_CURVE('',#6794,#6629,#1898,.F.);
#8636=EDGE_CURVE('',#6793,#6794,#5849,.T.);
#8637=EDGE_CURVE('',#6795,#6633,#1899,.F.);
#8638=EDGE_CURVE('',#6796,#6795,#5850,.T.);
#8639=EDGE_CURVE('',#6634,#6796,#1900,.T.);
#8640=EDGE_CURVE('',#6626,#6797,#1901,.T.);
#8641=EDGE_CURVE('',#6798,#6625,#1902,.F.);
#8642=EDGE_CURVE('',#6797,#6798,#5851,.T.);
#8643=EDGE_CURVE('',#6622,#6799,#1903,.T.);
#8644=EDGE_CURVE('',#6800,#6621,#1904,.F.);
#8645=EDGE_CURVE('',#6799,#6800,#5852,.T.);
#8646=EDGE_CURVE('',#6801,#6711,#5853,.T.);
#8647=EDGE_CURVE('',#6802,#6712,#5854,.T.);
#8648=EDGE_CURVE('',#6802,#6803,#5855,.T.);
#8649=EDGE_CURVE('',#6803,#6715,#5856,.T.);
#8650=EDGE_CURVE('',#6804,#6716,#5857,.T.);
#8651=EDGE_CURVE('',#6804,#6805,#5858,.T.);
#8652=EDGE_CURVE('',#6805,#6717,#5859,.T.);
#8653=EDGE_CURVE('',#6806,#6718,#5860,.T.);
#8654=EDGE_CURVE('',#6806,#6807,#5861,.T.);
#8655=EDGE_CURVE('',#6807,#6724,#5862,.T.);
#8656=EDGE_CURVE('',#6808,#6723,#5863,.T.);
#8657=EDGE_CURVE('',#6808,#6809,#5864,.T.);
#8658=EDGE_CURVE('',#6809,#6722,#5865,.T.);
#8659=EDGE_CURVE('',#6810,#6721,#5866,.T.);
#8660=EDGE_CURVE('',#6810,#6811,#5867,.T.);
#8661=EDGE_CURVE('',#6811,#6719,#5868,.T.);
#8662=EDGE_CURVE('',#6812,#6720,#5869,.T.);
#8663=EDGE_CURVE('',#6812,#6813,#5870,.T.);
#8664=EDGE_CURVE('',#6813,#6729,#5871,.T.);
#8665=EDGE_CURVE('',#6814,#6730,#5872,.T.);
#8666=EDGE_CURVE('',#6814,#6815,#5873,.T.);
#8667=EDGE_CURVE('',#6815,#6728,#5874,.T.);
#8668=EDGE_CURVE('',#6816,#6727,#5875,.T.);
#8669=EDGE_CURVE('',#6816,#6817,#5876,.T.);
#8670=EDGE_CURVE('',#6817,#6725,#5877,.T.);
#8671=EDGE_CURVE('',#6818,#6726,#5878,.T.);
#8672=EDGE_CURVE('',#6818,#6819,#5879,.T.);
#8673=EDGE_CURVE('',#6819,#6731,#5880,.T.);
#8674=EDGE_CURVE('',#6820,#6732,#5881,.T.);
#8675=EDGE_CURVE('',#6820,#6821,#5882,.T.);
#8676=EDGE_CURVE('',#6821,#6733,#5883,.T.);
#8677=EDGE_CURVE('',#6822,#6734,#5884,.T.);
#8678=EDGE_CURVE('',#6822,#6823,#5885,.T.);
#8679=EDGE_CURVE('',#6823,#6824,#5886,.T.);
#8680=EDGE_CURVE('',#6824,#6825,#5887,.T.);
#8681=EDGE_CURVE('',#6826,#6825,#5888,.T.);
#8682=EDGE_CURVE('',#6826,#6827,#5889,.T.);
#8683=EDGE_CURVE('',#6827,#6782,#5890,.T.);
#8684=EDGE_CURVE('',#6828,#6781,#5891,.T.);
#8685=EDGE_CURVE('',#6828,#6829,#5892,.T.);
#8686=EDGE_CURVE('',#6829,#6779,#5893,.T.);
#8687=EDGE_CURVE('',#6830,#6780,#5894,.T.);
#8688=EDGE_CURVE('',#6830,#6831,#5895,.T.);
#8689=EDGE_CURVE('',#6831,#6783,#5896,.T.);
#8690=EDGE_CURVE('',#6832,#6784,#5897,.T.);
#8691=EDGE_CURVE('',#6832,#6833,#5898,.T.);
#8692=EDGE_CURVE('',#6833,#6785,#5899,.T.);
#8693=EDGE_CURVE('',#6834,#6786,#5900,.T.);
#8694=EDGE_CURVE('',#6834,#6835,#5901,.T.);
#8695=EDGE_CURVE('',#6835,#6791,#5902,.T.);
#8696=EDGE_CURVE('',#6836,#6792,#5903,.T.);
#8697=EDGE_CURVE('',#6836,#6837,#5904,.T.);
#8698=EDGE_CURVE('',#6837,#6790,#5905,.T.);
#8699=EDGE_CURVE('',#6838,#6789,#5906,.T.);
#8700=EDGE_CURVE('',#6838,#6839,#5907,.T.);
#8701=EDGE_CURVE('',#6839,#6787,#5908,.T.);
#8702=EDGE_CURVE('',#6840,#6788,#5909,.T.);
#8703=EDGE_CURVE('',#6840,#6841,#5910,.T.);
#8704=EDGE_CURVE('',#6841,#6796,#5911,.T.);
#8705=EDGE_CURVE('',#6842,#6795,#5912,.T.);
#8706=EDGE_CURVE('',#6842,#6843,#5913,.T.);
#8707=EDGE_CURVE('',#6843,#6793,#5914,.T.);
#8708=EDGE_CURVE('',#6844,#6794,#5915,.T.);
#8709=EDGE_CURVE('',#6844,#6845,#5916,.T.);
#8710=EDGE_CURVE('',#6845,#6797,#5917,.T.);
#8711=EDGE_CURVE('',#6846,#6798,#5918,.T.);
#8712=EDGE_CURVE('',#6846,#6847,#5919,.T.);
#8713=EDGE_CURVE('',#6847,#6799,#5920,.T.);
#8714=EDGE_CURVE('',#6848,#6800,#5921,.T.);
#8715=EDGE_CURVE('',#6848,#6849,#5922,.T.);
#8716=EDGE_CURVE('',#6849,#6760,#5923,.T.);
#8717=EDGE_CURVE('',#6850,#6759,#5924,.T.);
#8718=EDGE_CURVE('',#6850,#6851,#5925,.T.);
#8719=EDGE_CURVE('',#6851,#6757,#5926,.T.);
#8720=EDGE_CURVE('',#6852,#6758,#5927,.T.);
#8721=EDGE_CURVE('',#6852,#6853,#5928,.T.);
#8722=EDGE_CURVE('',#6853,#6761,#5929,.T.);
#8723=EDGE_CURVE('',#6854,#6762,#5930,.T.);
#8724=EDGE_CURVE('',#6854,#6855,#5931,.T.);
#8725=EDGE_CURVE('',#6855,#6763,#5932,.T.);
#8726=EDGE_CURVE('',#6856,#6764,#5933,.T.);
#8727=EDGE_CURVE('',#6856,#6857,#5934,.T.);
#8728=EDGE_CURVE('',#6857,#6769,#5935,.T.);
#8729=EDGE_CURVE('',#6858,#6770,#5936,.T.);
#8730=EDGE_CURVE('',#6858,#6859,#5937,.T.);
#8731=EDGE_CURVE('',#6859,#6768,#5938,.T.);
#8732=EDGE_CURVE('',#6860,#6767,#5939,.T.);
#8733=EDGE_CURVE('',#6860,#6861,#5940,.T.);
#8734=EDGE_CURVE('',#6861,#6765,#5941,.T.);
#8735=EDGE_CURVE('',#6862,#6766,#5942,.T.);
#8736=EDGE_CURVE('',#6862,#6863,#5943,.T.);
#8737=EDGE_CURVE('',#6863,#6774,#5944,.T.);
#8738=EDGE_CURVE('',#6864,#6773,#5945,.T.);
#8739=EDGE_CURVE('',#6864,#6865,#5946,.T.);
#8740=EDGE_CURVE('',#6865,#6771,#5947,.T.);
#8741=EDGE_CURVE('',#6866,#6772,#5948,.T.);
#8742=EDGE_CURVE('',#6866,#6867,#5949,.T.);
#8743=EDGE_CURVE('',#6867,#6775,#5950,.T.);
#8744=EDGE_CURVE('',#6868,#6776,#5951,.T.);
#8745=EDGE_CURVE('',#6868,#6869,#5952,.T.);
#8746=EDGE_CURVE('',#6869,#6777,#5953,.T.);
#8747=EDGE_CURVE('',#6870,#6778,#5954,.T.);
#8748=EDGE_CURVE('',#6870,#6871,#5955,.T.);
#8749=EDGE_CURVE('',#6871,#6738,#5956,.T.);
#8750=EDGE_CURVE('',#6872,#6737,#5957,.T.);
#8751=EDGE_CURVE('',#6872,#6873,#5958,.T.);
#8752=EDGE_CURVE('',#6873,#6735,#5959,.T.);
#8753=EDGE_CURVE('',#6874,#6736,#5960,.T.);
#8754=EDGE_CURVE('',#6874,#6875,#5961,.T.);
#8755=EDGE_CURVE('',#6875,#6739,#5962,.T.);
#8756=EDGE_CURVE('',#6876,#6740,#5963,.T.);
#8757=EDGE_CURVE('',#6876,#6877,#5964,.T.);
#8758=EDGE_CURVE('',#6877,#6741,#5965,.T.);
#8759=EDGE_CURVE('',#6878,#6742,#5966,.T.);
#8760=EDGE_CURVE('',#6878,#6879,#5967,.T.);
#8761=EDGE_CURVE('',#6879,#6748,#5968,.T.);
#8762=EDGE_CURVE('',#6880,#6747,#5969,.T.);
#8763=EDGE_CURVE('',#6880,#6881,#5970,.T.);
#8764=EDGE_CURVE('',#6881,#6746,#5971,.T.);
#8765=EDGE_CURVE('',#6882,#6745,#5972,.T.);
#8766=EDGE_CURVE('',#6882,#6883,#5973,.T.);
#8767=EDGE_CURVE('',#6883,#6743,#5974,.T.);
#8768=EDGE_CURVE('',#6884,#6744,#5975,.T.);
#8769=EDGE_CURVE('',#6884,#6885,#5976,.T.);
#8770=EDGE_CURVE('',#6885,#6753,#5977,.T.);
#8771=EDGE_CURVE('',#6886,#6754,#5978,.T.);
#8772=EDGE_CURVE('',#6886,#6887,#5979,.T.);
#8773=EDGE_CURVE('',#6887,#6752,#5980,.T.);
#8774=EDGE_CURVE('',#6888,#6751,#5981,.T.);
#8775=EDGE_CURVE('',#6888,#6889,#5982,.T.);
#8776=EDGE_CURVE('',#6889,#6749,#5983,.T.);
#8777=EDGE_CURVE('',#6890,#6750,#5984,.T.);
#8778=EDGE_CURVE('',#6890,#6891,#5985,.T.);
#8779=EDGE_CURVE('',#6891,#6755,#5986,.T.);
#8780=EDGE_CURVE('',#6892,#6756,#5987,.T.);
#8781=EDGE_CURVE('',#6892,#6893,#5988,.T.);
#8782=EDGE_CURVE('',#6893,#6714,#5989,.T.);
#8783=EDGE_CURVE('',#6894,#6713,#5990,.T.);
#8784=EDGE_CURVE('',#6894,#6801,#5991,.T.);
#8785=EDGE_CURVE('',#6895,#6895,#5992,.F.);
#8786=EDGE_CURVE('',#6666,#6824,#1905,.T.);
#8787=EDGE_CURVE('',#6825,#6665,#1906,.F.);
#8788=EDGE_CURVE('',#6663,#6827,#1907,.T.);
#8789=EDGE_CURVE('',#6664,#6826,#1908,.T.);
#8790=EDGE_CURVE('',#6667,#6823,#1909,.T.);
#8791=EDGE_CURVE('',#6668,#6822,#1910,.T.);
#8792=EDGE_CURVE('',#6619,#6849,#1911,.T.);
#8793=EDGE_CURVE('',#6620,#6848,#1912,.T.);
#8794=EDGE_CURVE('',#6623,#6847,#1913,.T.);
#8795=EDGE_CURVE('',#6624,#6846,#1914,.T.);
#8796=EDGE_CURVE('',#6627,#6845,#1915,.T.);
#8797=EDGE_CURVE('',#6628,#6844,#1916,.T.);
#8798=EDGE_CURVE('',#6635,#6841,#1917,.T.);
#8799=EDGE_CURVE('',#6636,#6840,#1918,.T.);
#8800=EDGE_CURVE('',#6631,#6843,#1919,.T.);
#8801=EDGE_CURVE('',#6632,#6842,#1920,.T.);
#8802=EDGE_CURVE('',#6643,#6837,#1921,.T.);
#8803=EDGE_CURVE('',#6644,#6836,#1922,.T.);
#8804=EDGE_CURVE('',#6647,#6835,#1923,.T.);
#8805=EDGE_CURVE('',#6648,#6834,#1924,.T.);
#8806=EDGE_CURVE('',#6639,#6839,#1925,.T.);
#8807=EDGE_CURVE('',#6640,#6838,#1926,.T.);
#8808=EDGE_CURVE('',#6651,#6833,#1927,.T.);
#8809=EDGE_CURVE('',#6652,#6832,#1928,.T.);
#8810=EDGE_CURVE('',#6655,#6831,#1929,.T.);
#8811=EDGE_CURVE('',#6656,#6830,#1930,.T.);
#8812=EDGE_CURVE('',#6659,#6829,#1931,.T.);
#8813=EDGE_CURVE('',#6660,#6828,#1932,.T.);
#8814=EDGE_CURVE('',#6575,#6871,#1933,.T.);
#8815=EDGE_CURVE('',#6576,#6870,#1934,.T.);
#8816=EDGE_CURVE('',#6579,#6869,#1935,.T.);
#8817=EDGE_CURVE('',#6580,#6868,#1936,.T.);
#8818=EDGE_CURVE('',#6583,#6867,#1937,.T.);
#8819=EDGE_CURVE('',#6584,#6866,#1938,.T.);
#8820=EDGE_CURVE('',#6591,#6863,#1939,.T.);
#8821=EDGE_CURVE('',#6592,#6862,#1940,.T.);
#8822=EDGE_CURVE('',#6587,#6865,#1941,.T.);
#8823=EDGE_CURVE('',#6588,#6864,#1942,.T.);
#8824=EDGE_CURVE('',#6599,#6859,#1943,.T.);
#8825=EDGE_CURVE('',#6600,#6858,#1944,.T.);
#8826=EDGE_CURVE('',#6603,#6857,#1945,.T.);
#8827=EDGE_CURVE('',#6604,#6856,#1946,.T.);
#8828=EDGE_CURVE('',#6595,#6861,#1947,.T.);
#8829=EDGE_CURVE('',#6596,#6860,#1948,.T.);
#8830=EDGE_CURVE('',#6607,#6855,#1949,.T.);
#8831=EDGE_CURVE('',#6608,#6854,#1950,.T.);
#8832=EDGE_CURVE('',#6611,#6853,#1951,.T.);
#8833=EDGE_CURVE('',#6612,#6852,#1952,.T.);
#8834=EDGE_CURVE('',#6615,#6851,#1953,.T.);
#8835=EDGE_CURVE('',#6616,#6850,#1954,.T.);
#8836=EDGE_CURVE('',#6531,#6893,#1955,.T.);
#8837=EDGE_CURVE('',#6532,#6892,#1956,.T.);
#8838=EDGE_CURVE('',#6535,#6891,#1957,.T.);
#8839=EDGE_CURVE('',#6536,#6890,#1958,.T.);
#8840=EDGE_CURVE('',#6543,#6887,#1959,.T.);
#8841=EDGE_CURVE('',#6544,#6886,#1960,.T.);
#8842=EDGE_CURVE('',#6547,#6885,#1961,.T.);
#8843=EDGE_CURVE('',#6548,#6884,#1962,.T.);
#8844=EDGE_CURVE('',#6539,#6889,#1963,.T.);
#8845=EDGE_CURVE('',#6540,#6888,#1964,.T.);
#8846=EDGE_CURVE('',#6559,#6879,#1965,.T.);
#8847=EDGE_CURVE('',#6560,#6878,#1966,.T.);
#8848=EDGE_CURVE('',#6555,#6881,#1967,.T.);
#8849=EDGE_CURVE('',#6556,#6880,#1968,.T.);
#8850=EDGE_CURVE('',#6551,#6883,#1969,.T.);
#8851=EDGE_CURVE('',#6552,#6882,#1970,.T.);
#8852=EDGE_CURVE('',#6563,#6877,#1971,.T.);
#8853=EDGE_CURVE('',#6564,#6876,#1972,.T.);
#8854=EDGE_CURVE('',#6567,#6875,#1973,.T.);
#8855=EDGE_CURVE('',#6568,#6874,#1974,.T.);
#8856=EDGE_CURVE('',#6571,#6873,#1975,.T.);
#8857=EDGE_CURVE('',#6572,#6872,#1976,.T.);
#8858=EDGE_CURVE('',#6671,#6821,#1977,.T.);
#8859=EDGE_CURVE('',#6672,#6820,#1978,.T.);
#8860=EDGE_CURVE('',#6675,#6819,#1979,.T.);
#8861=EDGE_CURVE('',#6676,#6818,#1980,.T.);
#8862=EDGE_CURVE('',#6683,#6815,#1981,.T.);
#8863=EDGE_CURVE('',#6684,#6814,#1982,.T.);
#8864=EDGE_CURVE('',#6687,#6813,#1983,.T.);
#8865=EDGE_CURVE('',#6688,#6812,#1984,.T.);
#8866=EDGE_CURVE('',#6679,#6817,#1985,.T.);
#8867=EDGE_CURVE('',#6680,#6816,#1986,.T.);
#8868=EDGE_CURVE('',#6699,#6807,#1987,.T.);
#8869=EDGE_CURVE('',#6700,#6806,#1988,.T.);
#8870=EDGE_CURVE('',#6695,#6809,#1989,.T.);
#8871=EDGE_CURVE('',#6696,#6808,#1990,.T.);
#8872=EDGE_CURVE('',#6691,#6811,#1991,.T.);
#8873=EDGE_CURVE('',#6692,#6810,#1992,.T.);
#8874=EDGE_CURVE('',#6703,#6805,#1993,.T.);
#8875=EDGE_CURVE('',#6704,#6804,#1994,.T.);
#8876=EDGE_CURVE('',#6707,#6803,#1995,.T.);
#8877=EDGE_CURVE('',#6708,#6802,#1996,.T.);
#8878=EDGE_CURVE('',#6526,#6801,#1997,.T.);
#8879=EDGE_CURVE('',#6528,#6894,#1998,.T.);
#8880=EDGE_CURVE('',#6710,#6895,#1999,.T.);
#8881=EDGE_CURVE('',#6896,#6897,#1512,.T.);
#8882=EDGE_CURVE('',#6898,#6896,#343,.T.);
#8883=EDGE_CURVE('',#6898,#6899,#1513,.T.);
#8884=EDGE_CURVE('',#6900,#6899,#344,.T.);
#8885=EDGE_CURVE('',#6897,#6900,#345,.T.);
#8886=EDGE_CURVE('',#6900,#6901,#346,.T.);
#8887=EDGE_CURVE('',#6899,#6902,#347,.T.);
#8888=EDGE_CURVE('',#6902,#6903,#348,.F.);
#8889=EDGE_CURVE('',#6903,#6904,#349,.F.);
#8890=EDGE_CURVE('',#6904,#6905,#350,.F.);
#8891=EDGE_CURVE('',#6905,#6901,#351,.F.);
#8892=EDGE_CURVE('',#6906,#6907,#5993,.T.);
#8893=EDGE_CURVE('',#6907,#6906,#5994,.T.);
#8894=EDGE_CURVE('',#6906,#6908,#2000,.T.);
#8895=EDGE_CURVE('',#6908,#6909,#5995,.F.);
#8896=EDGE_CURVE('',#6909,#6908,#5996,.F.);
#8897=EDGE_CURVE('',#6910,#6910,#5997,.T.);
#8898=EDGE_CURVE('',#6910,#6911,#2001,.T.);
#8899=EDGE_CURVE('',#6911,#6912,#5998,.F.);
#8900=EDGE_CURVE('',#6912,#6911,#5999,.F.);
#8901=EDGE_CURVE('',#6913,#6914,#6000,.T.);
#8902=EDGE_CURVE('',#6914,#6913,#6001,.T.);
#8903=EDGE_CURVE('',#6913,#6915,#2002,.T.);
#8904=EDGE_CURVE('',#6915,#6916,#6002,.F.);
#8905=EDGE_CURVE('',#6916,#6915,#6003,.F.);
#8906=EDGE_CURVE('',#6917,#6917,#6004,.F.);
#8907=EDGE_CURVE('',#6917,#6918,#2003,.T.);
#8908=EDGE_CURVE('',#6918,#6919,#6005,.F.);
#8909=EDGE_CURVE('',#6919,#6918,#6006,.F.);
#8910=EDGE_CURVE('',#6920,#6920,#6007,.F.);
#8911=EDGE_CURVE('',#6921,#6921,#6008,.T.);
#8912=EDGE_CURVE('',#6922,#6922,#6009,.T.);
#8913=EDGE_CURVE('',#6923,#6924,#6010,.T.);
#8914=EDGE_CURVE('',#6924,#6923,#6011,.T.);
#8915=EDGE_CURVE('',#6924,#6925,#2004,.T.);
#8916=EDGE_CURVE('',#6925,#6925,#6012,.T.);
#8917=EDGE_CURVE('',#6926,#6927,#6013,.T.);
#8918=EDGE_CURVE('',#6927,#6926,#6014,.T.);
#8919=EDGE_CURVE('',#6927,#6928,#2005,.T.);
#8920=EDGE_CURVE('',#6928,#6928,#6015,.T.);
#8921=EDGE_CURVE('',#6929,#6929,#6016,.F.);
#8922=EDGE_CURVE('',#6929,#6930,#2006,.T.);
#8923=EDGE_CURVE('',#6930,#6931,#6017,.F.);
#8924=EDGE_CURVE('',#6931,#6930,#6018,.F.);
#8925=EDGE_CURVE('',#6932,#6932,#6019,.F.);
#8926=EDGE_CURVE('',#6932,#6933,#2007,.T.);
#8927=EDGE_CURVE('',#6933,#6934,#6020,.F.);
#8928=EDGE_CURVE('',#6934,#6933,#6021,.F.);
#8929=EDGE_CURVE('',#6935,#6936,#6022,.T.);
#8930=EDGE_CURVE('',#6936,#6935,#6023,.T.);
#8931=EDGE_CURVE('',#6936,#6937,#2008,.T.);
#8932=EDGE_CURVE('',#6937,#6937,#6024,.T.);
#8933=EDGE_CURVE('',#6938,#6939,#6025,.T.);
#8934=EDGE_CURVE('',#6939,#6938,#6026,.T.);
#8935=EDGE_CURVE('',#6939,#6940,#2009,.T.);
#8936=EDGE_CURVE('',#6940,#6940,#6027,.T.);
#8937=EDGE_CURVE('',#6941,#6941,#6028,.F.);
#8938=EDGE_CURVE('',#6941,#6942,#2010,.T.);
#8939=EDGE_CURVE('',#6942,#6943,#6029,.F.);
#8940=EDGE_CURVE('',#6943,#6942,#6030,.F.);
#8941=EDGE_CURVE('',#6944,#6945,#6031,.T.);
#8942=EDGE_CURVE('',#6945,#6944,#6032,.T.);
#8943=EDGE_CURVE('',#6945,#6946,#2011,.T.);
#8944=EDGE_CURVE('',#6946,#6946,#6033,.T.);
#8945=EDGE_CURVE('',#6947,#6947,#6034,.F.);
#8946=EDGE_CURVE('',#6947,#6948,#2012,.T.);
#8947=EDGE_CURVE('',#6948,#6949,#6035,.F.);
#8948=EDGE_CURVE('',#6949,#6948,#6036,.F.);
#8949=EDGE_CURVE('',#6950,#6951,#6037,.T.);
#8950=EDGE_CURVE('',#6951,#6950,#6038,.T.);
#8951=EDGE_CURVE('',#6951,#6952,#2013,.T.);
#8952=EDGE_CURVE('',#6952,#6952,#6039,.T.);
#8953=EDGE_CURVE('',#6953,#6953,#6040,.F.);
#8954=EDGE_CURVE('',#6953,#6954,#2014,.T.);
#8955=EDGE_CURVE('',#6954,#6955,#6041,.F.);
#8956=EDGE_CURVE('',#6955,#6954,#6042,.F.);
#8957=EDGE_CURVE('',#6956,#6957,#6043,.T.);
#8958=EDGE_CURVE('',#6957,#6956,#6044,.T.);
#8959=EDGE_CURVE('',#6957,#6958,#2015,.T.);
#8960=EDGE_CURVE('',#6958,#6958,#6045,.T.);
#8961=EDGE_CURVE('',#6959,#6959,#6046,.F.);
#8962=EDGE_CURVE('',#6959,#6960,#2016,.T.);
#8963=EDGE_CURVE('',#6960,#6961,#6047,.F.);
#8964=EDGE_CURVE('',#6961,#6960,#6048,.F.);
#8965=EDGE_CURVE('',#6901,#6962,#352,.F.);
#8966=EDGE_CURVE('',#6962,#6902,#353,.F.);
#8967=EDGE_CURVE('',#6899,#6897,#354,.T.);
#8968=EDGE_CURVE('',#6963,#6898,#355,.T.);
#8969=EDGE_CURVE('',#6896,#6963,#356,.T.);
#8970=EDGE_CURVE('',#6964,#6964,#6049,.T.);
#8971=EDGE_CURVE('',#6965,#6965,#6050,.F.);
#8972=EDGE_CURVE('',#6966,#6967,#357,.T.);
#8973=EDGE_CURVE('',#6967,#6968,#358,.T.);
#8974=EDGE_CURVE('',#6968,#6969,#359,.T.);
#8975=EDGE_CURVE('',#6969,#6966,#360,.T.);
#8976=EDGE_CURVE('',#6904,#6969,#361,.F.);
#8977=EDGE_CURVE('',#6966,#6903,#362,.F.);
#8978=EDGE_CURVE('',#6967,#6962,#363,.T.);
#8979=EDGE_CURVE('',#6905,#6968,#364,.T.);
#8980=EDGE_CURVE('',#6964,#6912,#6051,.T.);
#8981=EDGE_CURVE('',#6907,#6965,#6052,.T.);
#8982=EDGE_CURVE('',#6921,#6909,#6053,.T.);
#8983=EDGE_CURVE('',#6914,#6920,#6054,.T.);
#8984=EDGE_CURVE('',#6926,#6916,#6055,.T.);
#8985=EDGE_CURVE('',#6938,#6934,#6056,.T.);
#8986=EDGE_CURVE('',#6928,#6932,#6057,.T.);
#8987=EDGE_CURVE('',#6956,#6961,#6058,.T.);
#8988=EDGE_CURVE('',#6940,#6959,#6059,.T.);
#8989=EDGE_CURVE('',#6950,#6955,#6060,.T.);
#8990=EDGE_CURVE('',#6958,#6953,#6061,.T.);
#8991=EDGE_CURVE('',#6952,#6947,#6062,.T.);
#8992=EDGE_CURVE('',#6944,#6949,#6063,.T.);
#8993=EDGE_CURVE('',#6946,#6941,#6064,.T.);
#8994=EDGE_CURVE('',#6935,#6943,#6065,.T.);
#8995=EDGE_CURVE('',#6922,#6919,#6066,.T.);
#8996=EDGE_CURVE('',#6925,#6917,#6067,.T.);
#8997=EDGE_CURVE('',#6923,#6931,#6068,.T.);
#8998=EDGE_CURVE('',#6937,#6929,#6069,.T.);
#8999=EDGE_CURVE('',#6970,#6971,#6070,.T.);
#9000=EDGE_CURVE('',#6972,#6973,#365,.T.);
#9001=EDGE_CURVE('',#6972,#6974,#366,.T.);
#9002=EDGE_CURVE('',#6974,#6975,#367,.F.);
#9003=EDGE_CURVE('',#6975,#6976,#368,.T.);
#9004=EDGE_CURVE('',#6976,#6977,#369,.T.);
#9005=EDGE_CURVE('',#6977,#6978,#370,.T.);
#9006=EDGE_CURVE('',#6978,#6973,#6071,.F.);
#9007=EDGE_CURVE('',#6979,#6980,#371,.T.);
#9008=EDGE_CURVE('',#6979,#6981,#372,.F.);
#9009=EDGE_CURVE('',#6981,#6982,#373,.T.);
#9010=EDGE_CURVE('',#6982,#6983,#374,.F.);
#9011=EDGE_CURVE('',#6983,#6984,#375,.T.);
#9012=EDGE_CURVE('',#6984,#6985,#376,.F.);
#9013=EDGE_CURVE('',#6985,#6986,#377,.T.);
#9014=EDGE_CURVE('',#6986,#6987,#378,.T.);
#9015=EDGE_CURVE('',#6987,#6988,#379,.T.);
#9016=EDGE_CURVE('',#6988,#6989,#380,.T.);
#9017=EDGE_CURVE('',#6989,#6990,#381,.T.);
#9018=EDGE_CURVE('',#6990,#6991,#382,.T.);
#9019=EDGE_CURVE('',#6991,#6992,#383,.T.);
#9020=EDGE_CURVE('',#6992,#6980,#384,.T.);
#9021=EDGE_CURVE('',#6993,#6994,#385,.T.);
#9022=EDGE_CURVE('',#6993,#6995,#386,.T.);
#9023=EDGE_CURVE('',#6995,#6996,#387,.T.);
#9024=EDGE_CURVE('',#6996,#6997,#388,.T.);
#9025=EDGE_CURVE('',#6997,#6998,#389,.F.);
#9026=EDGE_CURVE('',#6998,#6999,#6072,.F.);
#9027=EDGE_CURVE('',#6999,#7000,#2017,.F.);
#9028=EDGE_CURVE('',#7000,#7001,#390,.F.);
#9029=EDGE_CURVE('',#7001,#7002,#391,.F.);
#9030=EDGE_CURVE('',#7002,#7003,#392,.F.);
#9031=EDGE_CURVE('',#7003,#7004,#393,.F.);
#9032=EDGE_CURVE('',#7004,#7005,#394,.T.);
#9033=EDGE_CURVE('',#7005,#7006,#395,.T.);
#9034=EDGE_CURVE('',#7006,#7007,#396,.T.);
#9035=EDGE_CURVE('',#7007,#7008,#397,.T.);
#9036=EDGE_CURVE('',#7008,#7009,#398,.T.);
#9037=EDGE_CURVE('',#7009,#7010,#399,.T.);
#9038=EDGE_CURVE('',#7010,#7011,#400,.T.);
#9039=EDGE_CURVE('',#7011,#7012,#2018,.F.);
#9040=EDGE_CURVE('',#7012,#7013,#401,.T.);
#9041=EDGE_CURVE('',#7013,#7014,#402,.T.);
#9042=EDGE_CURVE('',#7014,#7015,#403,.T.);
#9043=EDGE_CURVE('',#7015,#7016,#404,.T.);
#9044=EDGE_CURVE('',#7016,#7017,#405,.T.);
#9045=EDGE_CURVE('',#7017,#7018,#406,.T.);
#9046=EDGE_CURVE('',#7018,#7019,#407,.T.);
#9047=EDGE_CURVE('',#7019,#7020,#2019,.F.);
#9048=EDGE_CURVE('',#7020,#7021,#408,.T.);
#9049=EDGE_CURVE('',#7021,#7022,#409,.T.);
#9050=EDGE_CURVE('',#7022,#7023,#410,.T.);
#9051=EDGE_CURVE('',#7023,#7024,#411,.T.);
#9052=EDGE_CURVE('',#7024,#7025,#412,.T.);
#9053=EDGE_CURVE('',#7025,#7026,#413,.T.);
#9054=EDGE_CURVE('',#7026,#7027,#414,.T.);
#9055=EDGE_CURVE('',#7027,#7028,#415,.T.);
#9056=EDGE_CURVE('',#7028,#7029,#416,.T.);
#9057=EDGE_CURVE('',#7029,#7030,#417,.T.);
#9058=EDGE_CURVE('',#7030,#7031,#418,.T.);
#9059=EDGE_CURVE('',#7031,#7032,#419,.T.);
#9060=EDGE_CURVE('',#7032,#7033,#420,.T.);
#9061=EDGE_CURVE('',#7033,#7034,#421,.F.);
#9062=EDGE_CURVE('',#7034,#7035,#422,.F.);
#9063=EDGE_CURVE('',#7035,#7036,#423,.F.);
#9064=EDGE_CURVE('',#7036,#7037,#424,.F.);
#9065=EDGE_CURVE('',#7037,#7038,#425,.T.);
#9066=EDGE_CURVE('',#7038,#7039,#426,.T.);
#9067=EDGE_CURVE('',#7039,#7040,#427,.T.);
#9068=EDGE_CURVE('',#7040,#7041,#428,.T.);
#9069=EDGE_CURVE('',#7041,#7042,#429,.T.);
#9070=EDGE_CURVE('',#7042,#7043,#430,.T.);
#9071=EDGE_CURVE('',#7043,#7044,#431,.T.);
#9072=EDGE_CURVE('',#7044,#7045,#432,.T.);
#9073=EDGE_CURVE('',#7045,#7046,#433,.T.);
#9074=EDGE_CURVE('',#7046,#7047,#2020,.F.);
#9075=EDGE_CURVE('',#7047,#7048,#434,.T.);
#9076=EDGE_CURVE('',#7048,#7049,#435,.T.);
#9077=EDGE_CURVE('',#7049,#7050,#436,.T.);
#9078=EDGE_CURVE('',#7050,#7051,#437,.T.);
#9079=EDGE_CURVE('',#7051,#7052,#438,.T.);
#9080=EDGE_CURVE('',#7052,#7053,#2021,.T.);
#9081=EDGE_CURVE('',#7053,#7054,#439,.T.);
#9082=EDGE_CURVE('',#7054,#7055,#440,.T.);
#9083=EDGE_CURVE('',#7055,#7056,#441,.T.);
#9084=EDGE_CURVE('',#7056,#7057,#442,.T.);
#9085=EDGE_CURVE('',#7057,#7058,#443,.T.);
#9086=EDGE_CURVE('',#7058,#7059,#2022,.T.);
#9087=EDGE_CURVE('',#7059,#7060,#444,.T.);
#9088=EDGE_CURVE('',#7060,#7061,#445,.T.);
#9089=EDGE_CURVE('',#7061,#7062,#446,.T.);
#9090=EDGE_CURVE('',#7062,#7063,#447,.T.);
#9091=EDGE_CURVE('',#7063,#7064,#448,.T.);
#9092=EDGE_CURVE('',#7064,#7065,#2023,.T.);
#9093=EDGE_CURVE('',#7065,#7066,#449,.T.);
#9094=EDGE_CURVE('',#7066,#7067,#450,.T.);
#9095=EDGE_CURVE('',#7067,#7068,#451,.T.);
#9096=EDGE_CURVE('',#7068,#7069,#452,.T.);
#9097=EDGE_CURVE('',#7069,#7070,#453,.T.);
#9098=EDGE_CURVE('',#7070,#7071,#2024,.T.);
#9099=EDGE_CURVE('',#7071,#7072,#454,.T.);
#9100=EDGE_CURVE('',#7072,#7073,#455,.T.);
#9101=EDGE_CURVE('',#7073,#7074,#456,.T.);
#9102=EDGE_CURVE('',#7074,#7075,#457,.T.);
#9103=EDGE_CURVE('',#7075,#7076,#458,.T.);
#9104=EDGE_CURVE('',#7076,#7077,#2025,.T.);
#9105=EDGE_CURVE('',#7077,#7078,#459,.T.);
#9106=EDGE_CURVE('',#7078,#7079,#460,.T.);
#9107=EDGE_CURVE('',#7079,#7080,#461,.T.);
#9108=EDGE_CURVE('',#7080,#7081,#462,.T.);
#9109=EDGE_CURVE('',#7081,#7082,#463,.T.);
#9110=EDGE_CURVE('',#7082,#7083,#2026,.T.);
#9111=EDGE_CURVE('',#7083,#7084,#464,.F.);
#9112=EDGE_CURVE('',#7084,#7085,#465,.T.);
#9113=EDGE_CURVE('',#7085,#7086,#466,.T.);
#9114=EDGE_CURVE('',#7086,#7087,#467,.T.);
#9115=EDGE_CURVE('',#7087,#7088,#468,.T.);
#9116=EDGE_CURVE('',#7088,#7089,#2027,.T.);
#9117=EDGE_CURVE('',#7089,#7090,#469,.T.);
#9118=EDGE_CURVE('',#7090,#7091,#470,.T.);
#9119=EDGE_CURVE('',#7091,#7092,#471,.T.);
#9120=EDGE_CURVE('',#7092,#7093,#472,.T.);
#9121=EDGE_CURVE('',#7093,#7094,#473,.T.);
#9122=EDGE_CURVE('',#7094,#7095,#2028,.T.);
#9123=EDGE_CURVE('',#7095,#7096,#474,.T.);
#9124=EDGE_CURVE('',#7096,#7097,#475,.T.);
#9125=EDGE_CURVE('',#7097,#7098,#476,.T.);
#9126=EDGE_CURVE('',#7098,#7099,#477,.T.);
#9127=EDGE_CURVE('',#7099,#7100,#478,.T.);
#9128=EDGE_CURVE('',#7100,#7101,#2029,.T.);
#9129=EDGE_CURVE('',#7101,#7102,#479,.T.);
#9130=EDGE_CURVE('',#7102,#7103,#480,.T.);
#9131=EDGE_CURVE('',#7103,#7104,#481,.T.);
#9132=EDGE_CURVE('',#7104,#7105,#482,.T.);
#9133=EDGE_CURVE('',#7105,#7106,#483,.T.);
#9134=EDGE_CURVE('',#7106,#7107,#2030,.T.);
#9135=EDGE_CURVE('',#7107,#7108,#484,.T.);
#9136=EDGE_CURVE('',#7108,#7109,#485,.T.);
#9137=EDGE_CURVE('',#7109,#7110,#486,.T.);
#9138=EDGE_CURVE('',#7110,#7111,#487,.T.);
#9139=EDGE_CURVE('',#7111,#7112,#488,.T.);
#9140=EDGE_CURVE('',#7112,#7113,#2031,.T.);
#9141=EDGE_CURVE('',#7113,#7114,#489,.T.);
#9142=EDGE_CURVE('',#7114,#7115,#490,.T.);
#9143=EDGE_CURVE('',#7115,#7116,#491,.T.);
#9144=EDGE_CURVE('',#7116,#7117,#492,.F.);
#9145=EDGE_CURVE('',#7117,#7118,#493,.F.);
#9146=EDGE_CURVE('',#7118,#7119,#494,.T.);
#9147=EDGE_CURVE('',#7119,#7120,#495,.T.);
#9148=EDGE_CURVE('',#7120,#7121,#496,.T.);
#9149=EDGE_CURVE('',#7121,#7122,#497,.F.);
#9150=EDGE_CURVE('',#7122,#7123,#498,.F.);
#9151=EDGE_CURVE('',#7123,#7124,#499,.T.);
#9152=EDGE_CURVE('',#7124,#7125,#500,.T.);
#9153=EDGE_CURVE('',#7125,#7126,#501,.F.);
#9154=EDGE_CURVE('',#7126,#7127,#502,.F.);
#9155=EDGE_CURVE('',#7127,#7128,#503,.F.);
#9156=EDGE_CURVE('',#7128,#7129,#504,.F.);
#9157=EDGE_CURVE('',#7129,#7130,#505,.T.);
#9158=EDGE_CURVE('',#7130,#7131,#506,.F.);
#9159=EDGE_CURVE('',#7131,#6994,#507,.T.);
#9160=EDGE_CURVE('',#7132,#7133,#508,.T.);
#9161=EDGE_CURVE('',#7134,#7132,#509,.T.);
#9162=EDGE_CURVE('',#7134,#7135,#510,.T.);
#9163=EDGE_CURVE('',#7135,#7136,#511,.T.);
#9164=EDGE_CURVE('',#7137,#7136,#512,.T.);
#9165=EDGE_CURVE('',#7137,#7138,#513,.T.);
#9166=EDGE_CURVE('',#7139,#7138,#514,.T.);
#9167=EDGE_CURVE('',#7139,#7140,#515,.T.);
#9168=EDGE_CURVE('',#7140,#7141,#516,.T.);
#9169=EDGE_CURVE('',#7141,#7142,#517,.T.);
#9170=EDGE_CURVE('',#7142,#7143,#518,.T.);
#9171=EDGE_CURVE('',#7144,#7143,#519,.T.);
#9172=EDGE_CURVE('',#7145,#7144,#520,.T.);
#9173=EDGE_CURVE('',#7145,#7146,#521,.F.);
#9174=EDGE_CURVE('',#7146,#7147,#522,.T.);
#9175=EDGE_CURVE('',#7147,#7148,#523,.F.);
#9176=EDGE_CURVE('',#7149,#7148,#524,.T.);
#9177=EDGE_CURVE('',#7150,#7149,#525,.T.);
#9178=EDGE_CURVE('',#7150,#7151,#526,.T.);
#9179=EDGE_CURVE('',#7151,#7152,#527,.T.);
#9180=EDGE_CURVE('',#7153,#7152,#528,.T.);
#9181=EDGE_CURVE('',#7154,#7153,#529,.T.);
#9182=EDGE_CURVE('',#7155,#7154,#6073,.T.);
#9183=EDGE_CURVE('',#7156,#7155,#530,.T.);
#9184=EDGE_CURVE('',#7157,#7156,#6074,.T.);
#9185=EDGE_CURVE('',#7158,#7157,#531,.T.);
#9186=EDGE_CURVE('',#7159,#7158,#532,.T.);
#9187=EDGE_CURVE('',#7160,#7159,#533,.T.);
#9188=EDGE_CURVE('',#7161,#7160,#534,.T.);
#9189=EDGE_CURVE('',#7161,#7162,#535,.F.);
#9190=EDGE_CURVE('',#7162,#7163,#536,.F.);
#9191=EDGE_CURVE('',#7164,#7163,#537,.T.);
#9192=EDGE_CURVE('',#7165,#7164,#538,.T.);
#9193=EDGE_CURVE('',#7166,#7165,#539,.T.);
#9194=EDGE_CURVE('',#7166,#7167,#540,.F.);
#9195=EDGE_CURVE('',#7167,#7168,#541,.T.);
#9196=EDGE_CURVE('',#7133,#7168,#542,.T.);
#9197=EDGE_CURVE('',#7169,#7170,#543,.F.);
#9198=EDGE_CURVE('',#7171,#7170,#544,.T.);
#9199=EDGE_CURVE('',#7172,#7171,#545,.T.);
#9200=EDGE_CURVE('',#7169,#7172,#546,.T.);
#9201=EDGE_CURVE('',#7173,#7174,#547,.F.);
#9202=EDGE_CURVE('',#7174,#7175,#548,.F.);
#9203=EDGE_CURVE('',#7176,#7175,#549,.T.);
#9204=EDGE_CURVE('',#7176,#7173,#550,.F.);
#9205=EDGE_CURVE('',#7177,#7133,#551,.T.);
#9206=EDGE_CURVE('',#7138,#7177,#552,.T.);
#9207=EDGE_CURVE('',#7178,#7137,#553,.T.);
#9208=EDGE_CURVE('',#7132,#7178,#554,.T.);
#9209=EDGE_CURVE('',#7179,#7180,#555,.F.);
#9210=EDGE_CURVE('',#7181,#7179,#556,.F.);
#9211=EDGE_CURVE('',#7182,#7181,#557,.F.);
#9212=EDGE_CURVE('',#7180,#7182,#558,.F.);
#9213=EDGE_CURVE('',#6994,#7183,#559,.T.);
#9214=EDGE_CURVE('',#7183,#7184,#560,.F.);
#9215=EDGE_CURVE('',#7184,#7185,#561,.T.);
#9216=EDGE_CURVE('',#7185,#7186,#562,.F.);
#9217=EDGE_CURVE('',#7186,#7187,#563,.F.);
#9218=EDGE_CURVE('',#7187,#7188,#564,.F.);
#9219=EDGE_CURVE('',#7188,#7189,#565,.F.);
#9220=EDGE_CURVE('',#7189,#7190,#566,.T.);
#9221=EDGE_CURVE('',#7190,#7191,#567,.F.);
#9222=EDGE_CURVE('',#7191,#7192,#568,.T.);
#9223=EDGE_CURVE('',#7192,#7193,#569,.F.);
#9224=EDGE_CURVE('',#7193,#7124,#570,.T.);
#9225=EDGE_CURVE('',#7123,#7194,#571,.F.);
#9226=EDGE_CURVE('',#7194,#7195,#572,.T.);
#9227=EDGE_CURVE('',#7195,#7196,#573,.T.);
#9228=EDGE_CURVE('',#7196,#7197,#574,.F.);
#9229=EDGE_CURVE('',#7197,#7198,#575,.F.);
#9230=EDGE_CURVE('',#7198,#7116,#576,.F.);
#9231=EDGE_CURVE('',#7115,#7199,#577,.T.);
#9232=EDGE_CURVE('',#7199,#7200,#2032,.T.);
#9233=EDGE_CURVE('',#7200,#7110,#578,.T.);
#9234=EDGE_CURVE('',#7109,#7201,#579,.T.);
#9235=EDGE_CURVE('',#7201,#7202,#2033,.T.);
#9236=EDGE_CURVE('',#7202,#7104,#580,.T.);
#9237=EDGE_CURVE('',#7103,#7203,#581,.T.);
#9238=EDGE_CURVE('',#7203,#7204,#2034,.T.);
#9239=EDGE_CURVE('',#7204,#7098,#582,.T.);
#9240=EDGE_CURVE('',#7097,#7205,#583,.T.);
#9241=EDGE_CURVE('',#7205,#7206,#2035,.T.);
#9242=EDGE_CURVE('',#7206,#7092,#584,.T.);
#9243=EDGE_CURVE('',#7091,#7207,#585,.T.);
#9244=EDGE_CURVE('',#7207,#7208,#2036,.T.);
#9245=EDGE_CURVE('',#7208,#7086,#586,.T.);
#9246=EDGE_CURVE('',#7085,#7209,#587,.T.);
#9247=EDGE_CURVE('',#7209,#7210,#2037,.T.);
#9248=EDGE_CURVE('',#7210,#7080,#588,.T.);
#9249=EDGE_CURVE('',#7079,#7211,#589,.T.);
#9250=EDGE_CURVE('',#7211,#7212,#2038,.T.);
#9251=EDGE_CURVE('',#7212,#7074,#590,.T.);
#9252=EDGE_CURVE('',#7073,#7213,#591,.T.);
#9253=EDGE_CURVE('',#7213,#7214,#2039,.T.);
#9254=EDGE_CURVE('',#7214,#7068,#592,.T.);
#9255=EDGE_CURVE('',#7067,#7215,#593,.T.);
#9256=EDGE_CURVE('',#7215,#7216,#2040,.T.);
#9257=EDGE_CURVE('',#7216,#7062,#594,.T.);
#9258=EDGE_CURVE('',#7061,#7217,#595,.T.);
#9259=EDGE_CURVE('',#7217,#7218,#2041,.T.);
#9260=EDGE_CURVE('',#7218,#7056,#596,.T.);
#9261=EDGE_CURVE('',#7055,#7219,#597,.T.);
#9262=EDGE_CURVE('',#7219,#7220,#2042,.T.);
#9263=EDGE_CURVE('',#7220,#7050,#598,.T.);
#9264=EDGE_CURVE('',#7049,#7221,#599,.T.);
#9265=EDGE_CURVE('',#7221,#7222,#2043,.F.);
#9266=EDGE_CURVE('',#7222,#7223,#600,.T.);
#9267=EDGE_CURVE('',#7223,#7043,#601,.T.);
#9268=EDGE_CURVE('',#7042,#7224,#602,.T.);
#9269=EDGE_CURVE('',#7224,#7225,#603,.T.);
#9270=EDGE_CURVE('',#7225,#7226,#604,.T.);
#9271=EDGE_CURVE('',#7226,#7227,#605,.T.);
#9272=EDGE_CURVE('',#7227,#7032,#606,.T.);
#9273=EDGE_CURVE('',#7031,#7228,#607,.T.);
#9274=EDGE_CURVE('',#7228,#7229,#608,.T.);
#9275=EDGE_CURVE('',#7229,#7230,#609,.T.);
#9276=EDGE_CURVE('',#7230,#7231,#610,.T.);
#9277=EDGE_CURVE('',#7231,#7024,#611,.T.);
#9278=EDGE_CURVE('',#7023,#7232,#612,.T.);
#9279=EDGE_CURVE('',#7232,#7233,#613,.T.);
#9280=EDGE_CURVE('',#7233,#7234,#2044,.F.);
#9281=EDGE_CURVE('',#7234,#7235,#614,.T.);
#9282=EDGE_CURVE('',#7235,#7016,#615,.T.);
#9283=EDGE_CURVE('',#7015,#7236,#616,.T.);
#9284=EDGE_CURVE('',#7236,#7237,#617,.T.);
#9285=EDGE_CURVE('',#7237,#7238,#2045,.F.);
#9286=EDGE_CURVE('',#7238,#7239,#618,.T.);
#9287=EDGE_CURVE('',#7239,#7008,#619,.T.);
#9288=EDGE_CURVE('',#7007,#7240,#620,.T.);
#9289=EDGE_CURVE('',#7240,#7241,#621,.T.);
#9290=EDGE_CURVE('',#7241,#7242,#622,.F.);
#9291=EDGE_CURVE('',#7242,#7243,#623,.F.);
#9292=EDGE_CURVE('',#7243,#7244,#624,.F.);
#9293=EDGE_CURVE('',#7244,#7245,#625,.F.);
#9294=EDGE_CURVE('',#7245,#7246,#2046,.F.);
#9295=EDGE_CURVE('',#7246,#7247,#6075,.F.);
#9296=EDGE_CURVE('',#7247,#7248,#626,.F.);
#9297=EDGE_CURVE('',#7248,#7249,#627,.T.);
#9298=EDGE_CURVE('',#7249,#7250,#628,.T.);
#9299=EDGE_CURVE('',#7250,#7251,#629,.T.);
#9300=EDGE_CURVE('',#7251,#7252,#630,.T.);
#9301=EDGE_CURVE('',#7252,#7253,#631,.T.);
#9302=EDGE_CURVE('',#7253,#7254,#632,.T.);
#9303=EDGE_CURVE('',#7254,#7255,#633,.T.);
#9304=EDGE_CURVE('',#7255,#7256,#634,.T.);
#9305=EDGE_CURVE('',#7256,#7257,#635,.F.);
#9306=EDGE_CURVE('',#7257,#7258,#6076,.F.);
#9307=EDGE_CURVE('',#7258,#7259,#2047,.F.);
#9308=EDGE_CURVE('',#7259,#7260,#6077,.F.);
#9309=EDGE_CURVE('',#7260,#7261,#636,.F.);
#9310=EDGE_CURVE('',#7261,#7262,#637,.F.);
#9311=EDGE_CURVE('',#7262,#7263,#638,.F.);
#9312=EDGE_CURVE('',#7263,#7264,#639,.F.);
#9313=EDGE_CURVE('',#7264,#7265,#640,.T.);
#9314=EDGE_CURVE('',#7265,#7266,#641,.T.);
#9315=EDGE_CURVE('',#7266,#7267,#642,.T.);
#9316=EDGE_CURVE('',#7267,#7268,#643,.T.);
#9317=EDGE_CURVE('',#7268,#7269,#644,.F.);
#9318=EDGE_CURVE('',#7269,#7270,#645,.F.);
#9319=EDGE_CURVE('',#7270,#7271,#646,.F.);
#9320=EDGE_CURVE('',#7271,#7272,#2048,.F.);
#9321=EDGE_CURVE('',#7272,#7273,#6078,.F.);
#9322=EDGE_CURVE('',#7273,#7274,#647,.F.);
#9323=EDGE_CURVE('',#7274,#7275,#648,.T.);
#9324=EDGE_CURVE('',#7275,#7276,#649,.T.);
#9325=EDGE_CURVE('',#7276,#6993,#650,.T.);
#9326=EDGE_CURVE('',#7277,#7278,#2049,.T.);
#9327=EDGE_CURVE('',#7278,#7279,#651,.F.);
#9328=EDGE_CURVE('',#7279,#7280,#652,.T.);
#9329=EDGE_CURVE('',#7280,#7281,#2050,.T.);
#9330=EDGE_CURVE('',#7281,#7282,#653,.T.);
#9331=EDGE_CURVE('',#7282,#7277,#654,.T.);
#9332=EDGE_CURVE('',#7283,#7284,#2051,.T.);
#9333=EDGE_CURVE('',#7284,#7285,#655,.T.);
#9334=EDGE_CURVE('',#7285,#7286,#656,.T.);
#9335=EDGE_CURVE('',#7286,#7287,#2052,.T.);
#9336=EDGE_CURVE('',#7287,#7288,#657,.T.);
#9337=EDGE_CURVE('',#7288,#7283,#658,.T.);
#9338=EDGE_CURVE('',#7289,#7290,#2053,.T.);
#9339=EDGE_CURVE('',#7290,#7291,#659,.T.);
#9340=EDGE_CURVE('',#7291,#7292,#660,.T.);
#9341=EDGE_CURVE('',#7292,#7293,#2054,.T.);
#9342=EDGE_CURVE('',#7293,#7294,#661,.T.);
#9343=EDGE_CURVE('',#7294,#7289,#662,.T.);
#9344=EDGE_CURVE('',#7295,#7296,#2055,.T.);
#9345=EDGE_CURVE('',#7296,#7297,#663,.T.);
#9346=EDGE_CURVE('',#7297,#7298,#664,.T.);
#9347=EDGE_CURVE('',#7298,#7299,#2056,.T.);
#9348=EDGE_CURVE('',#7299,#7300,#665,.T.);
#9349=EDGE_CURVE('',#7300,#7295,#666,.T.);
#9350=EDGE_CURVE('',#7301,#7302,#2057,.T.);
#9351=EDGE_CURVE('',#7302,#7303,#667,.T.);
#9352=EDGE_CURVE('',#7303,#7304,#668,.T.);
#9353=EDGE_CURVE('',#7304,#7305,#2058,.T.);
#9354=EDGE_CURVE('',#7305,#7306,#669,.T.);
#9355=EDGE_CURVE('',#7306,#7301,#670,.T.);
#9356=EDGE_CURVE('',#7307,#7308,#2059,.T.);
#9357=EDGE_CURVE('',#7308,#7309,#671,.T.);
#9358=EDGE_CURVE('',#7309,#7310,#672,.T.);
#9359=EDGE_CURVE('',#7310,#7311,#2060,.T.);
#9360=EDGE_CURVE('',#7311,#7312,#673,.T.);
#9361=EDGE_CURVE('',#7312,#7307,#674,.T.);
#9362=EDGE_CURVE('',#7313,#7314,#2061,.F.);
#9363=EDGE_CURVE('',#7314,#7315,#675,.T.);
#9364=EDGE_CURVE('',#7315,#7316,#676,.T.);
#9365=EDGE_CURVE('',#7316,#7317,#677,.T.);
#9366=EDGE_CURVE('',#7317,#7318,#678,.T.);
#9367=EDGE_CURVE('',#7318,#7319,#2062,.F.);
#9368=EDGE_CURVE('',#7319,#7320,#679,.T.);
#9369=EDGE_CURVE('',#7320,#7321,#680,.T.);
#9370=EDGE_CURVE('',#7321,#7322,#681,.T.);
#9371=EDGE_CURVE('',#7322,#7313,#682,.T.);
#9372=EDGE_CURVE('',#7323,#7324,#2063,.T.);
#9373=EDGE_CURVE('',#7324,#7325,#683,.T.);
#9374=EDGE_CURVE('',#7325,#7326,#684,.T.);
#9375=EDGE_CURVE('',#7326,#7327,#2064,.T.);
#9376=EDGE_CURVE('',#7327,#7328,#685,.T.);
#9377=EDGE_CURVE('',#7328,#7323,#686,.T.);
#9378=EDGE_CURVE('',#7329,#7330,#2065,.T.);
#9379=EDGE_CURVE('',#7330,#7331,#687,.T.);
#9380=EDGE_CURVE('',#7331,#7332,#688,.T.);
#9381=EDGE_CURVE('',#7332,#7333,#2066,.T.);
#9382=EDGE_CURVE('',#7333,#7334,#689,.T.);
#9383=EDGE_CURVE('',#7334,#7329,#690,.T.);
#9384=EDGE_CURVE('',#7335,#7336,#2067,.T.);
#9385=EDGE_CURVE('',#7336,#7337,#691,.T.);
#9386=EDGE_CURVE('',#7337,#7338,#692,.T.);
#9387=EDGE_CURVE('',#7338,#7339,#2068,.T.);
#9388=EDGE_CURVE('',#7339,#7340,#693,.T.);
#9389=EDGE_CURVE('',#7340,#7335,#694,.T.);
#9390=EDGE_CURVE('',#7341,#7342,#2069,.T.);
#9391=EDGE_CURVE('',#7342,#7343,#695,.T.);
#9392=EDGE_CURVE('',#7343,#7344,#696,.T.);
#9393=EDGE_CURVE('',#7344,#7345,#2070,.T.);
#9394=EDGE_CURVE('',#7345,#7346,#697,.T.);
#9395=EDGE_CURVE('',#7346,#7341,#698,.T.);
#9396=EDGE_CURVE('',#7347,#7348,#2071,.T.);
#9397=EDGE_CURVE('',#7348,#7349,#699,.T.);
#9398=EDGE_CURVE('',#7349,#7350,#700,.T.);
#9399=EDGE_CURVE('',#7350,#7351,#2072,.T.);
#9400=EDGE_CURVE('',#7351,#7352,#701,.T.);
#9401=EDGE_CURVE('',#7352,#7347,#702,.T.);
#9402=EDGE_CURVE('',#7353,#7354,#2073,.F.);
#9403=EDGE_CURVE('',#7354,#7355,#703,.T.);
#9404=EDGE_CURVE('',#7355,#7356,#704,.T.);
#9405=EDGE_CURVE('',#7356,#7357,#705,.T.);
#9406=EDGE_CURVE('',#7357,#7358,#706,.T.);
#9407=EDGE_CURVE('',#7358,#7359,#2074,.F.);
#9408=EDGE_CURVE('',#7359,#7360,#707,.T.);
#9409=EDGE_CURVE('',#7360,#7361,#708,.T.);
#9410=EDGE_CURVE('',#7361,#7362,#709,.T.);
#9411=EDGE_CURVE('',#7362,#7353,#710,.T.);
#9412=EDGE_CURVE('',#7363,#7364,#711,.T.);
#9413=EDGE_CURVE('',#7364,#7365,#712,.T.);
#9414=EDGE_CURVE('',#7365,#7366,#713,.T.);
#9415=EDGE_CURVE('',#7366,#7367,#714,.T.);
#9416=EDGE_CURVE('',#7367,#7368,#715,.T.);
#9417=EDGE_CURVE('',#7368,#7369,#716,.T.);
#9418=EDGE_CURVE('',#7369,#7370,#717,.T.);
#9419=EDGE_CURVE('',#7370,#7371,#718,.T.);
#9420=EDGE_CURVE('',#7371,#7372,#719,.T.);
#9421=EDGE_CURVE('',#7372,#7363,#720,.T.);
#9422=EDGE_CURVE('',#7373,#7374,#721,.T.);
#9423=EDGE_CURVE('',#7374,#7375,#722,.T.);
#9424=EDGE_CURVE('',#7375,#7376,#723,.T.);
#9425=EDGE_CURVE('',#7376,#7377,#724,.T.);
#9426=EDGE_CURVE('',#7377,#7378,#725,.T.);
#9427=EDGE_CURVE('',#7378,#7379,#726,.T.);
#9428=EDGE_CURVE('',#7379,#7380,#727,.T.);
#9429=EDGE_CURVE('',#7380,#7381,#728,.T.);
#9430=EDGE_CURVE('',#7381,#7382,#729,.F.);
#9431=EDGE_CURVE('',#7382,#7383,#730,.F.);
#9432=EDGE_CURVE('',#7383,#7384,#731,.F.);
#9433=EDGE_CURVE('',#7384,#7373,#732,.F.);
#9434=EDGE_CURVE('',#7385,#7386,#2075,.F.);
#9435=EDGE_CURVE('',#7386,#7387,#733,.T.);
#9436=EDGE_CURVE('',#7387,#7388,#734,.T.);
#9437=EDGE_CURVE('',#7388,#7389,#2076,.F.);
#9438=EDGE_CURVE('',#7389,#7390,#735,.T.);
#9439=EDGE_CURVE('',#7390,#7391,#736,.T.);
#9440=EDGE_CURVE('',#7391,#7392,#737,.T.);
#9441=EDGE_CURVE('',#7392,#7385,#738,.T.);
#9442=EDGE_CURVE('',#7393,#7394,#739,.F.);
#9443=EDGE_CURVE('',#7394,#7395,#740,.T.);
#9444=EDGE_CURVE('',#7395,#7396,#741,.T.);
#9445=EDGE_CURVE('',#7396,#7397,#742,.F.);
#9446=EDGE_CURVE('',#7397,#7398,#743,.F.);
#9447=EDGE_CURVE('',#7398,#7399,#744,.F.);
#9448=EDGE_CURVE('',#7399,#7400,#745,.F.);
#9449=EDGE_CURVE('',#7400,#7401,#746,.T.);
#9450=EDGE_CURVE('',#7401,#7402,#747,.T.);
#9451=EDGE_CURVE('',#7402,#7403,#748,.T.);
#9452=EDGE_CURVE('',#7403,#7393,#749,.F.);
#9453=EDGE_CURVE('',#6980,#6986,#750,.T.);
#9454=EDGE_CURVE('',#6985,#6979,#751,.F.);
#9455=EDGE_CURVE('',#7169,#7179,#2077,.T.);
#9456=EDGE_CURVE('',#7181,#7172,#2078,.T.);
#9457=EDGE_CURVE('',#7175,#7404,#752,.T.);
#9458=EDGE_CURVE('',#7404,#7405,#753,.F.);
#9459=EDGE_CURVE('',#7176,#7405,#754,.F.);
#9460=EDGE_CURVE('',#7405,#7406,#755,.F.);
#9461=EDGE_CURVE('',#7173,#7406,#756,.F.);
#9462=EDGE_CURVE('',#7407,#7408,#757,.T.);
#9463=EDGE_CURVE('',#7408,#7409,#6079,.F.);
#9464=EDGE_CURVE('',#7409,#7410,#758,.T.);
#9465=EDGE_CURVE('',#7410,#7411,#759,.T.);
#9466=EDGE_CURVE('',#7411,#7407,#2079,.T.);
#9467=EDGE_CURVE('',#7412,#7413,#2080,.T.);
#9468=EDGE_CURVE('',#7413,#7414,#760,.T.);
#9469=EDGE_CURVE('',#7414,#7415,#761,.T.);
#9470=EDGE_CURVE('',#7415,#7416,#6080,.F.);
#9471=EDGE_CURVE('',#7416,#7412,#762,.T.);
#9472=EDGE_CURVE('',#7417,#7418,#2081,.T.);
#9473=EDGE_CURVE('',#7417,#7419,#763,.T.);
#9474=EDGE_CURVE('',#7419,#7420,#764,.T.);
#9475=EDGE_CURVE('',#7420,#7421,#765,.T.);
#9476=EDGE_CURVE('',#7421,#7418,#766,.T.);
#9477=EDGE_CURVE('',#7422,#7423,#767,.T.);
#9478=EDGE_CURVE('',#7423,#7424,#6081,.F.);
#9479=EDGE_CURVE('',#7424,#7425,#768,.T.);
#9480=EDGE_CURVE('',#7425,#7426,#769,.T.);
#9481=EDGE_CURVE('',#7422,#7426,#2082,.T.);
#9482=EDGE_CURVE('',#7427,#7404,#770,.F.);
#9483=EDGE_CURVE('',#7406,#7427,#771,.F.);
#9484=EDGE_CURVE('',#6973,#7428,#6082,.F.);
#9485=EDGE_CURVE('',#7428,#7429,#772,.T.);
#9486=EDGE_CURVE('',#7429,#7430,#773,.T.);
#9487=EDGE_CURVE('',#7430,#7431,#6083,.F.);
#9488=EDGE_CURVE('',#7431,#6977,#774,.T.);
#9489=EDGE_CURVE('',#6976,#7432,#6084,.F.);
#9490=EDGE_CURVE('',#7432,#7433,#775,.T.);
#9491=EDGE_CURVE('',#7433,#7434,#776,.F.);
#9492=EDGE_CURVE('',#7434,#7435,#777,.T.);
#9493=EDGE_CURVE('',#7435,#7436,#778,.F.);
#9494=EDGE_CURVE('',#7436,#7437,#779,.T.);
#9495=EDGE_CURVE('',#7437,#7438,#6085,.F.);
#9496=EDGE_CURVE('',#7438,#7439,#780,.T.);
#9497=EDGE_CURVE('',#7439,#7440,#781,.F.);
#9498=EDGE_CURVE('',#7440,#6972,#782,.T.);
#9499=EDGE_CURVE('',#7127,#7441,#783,.T.);
#9500=EDGE_CURVE('',#7441,#7442,#784,.T.);
#9501=EDGE_CURVE('',#7442,#7443,#785,.F.);
#9502=EDGE_CURVE('',#7443,#7444,#786,.T.);
#9503=EDGE_CURVE('',#7444,#7445,#787,.T.);
#9504=EDGE_CURVE('',#7445,#7446,#788,.T.);
#9505=EDGE_CURVE('',#7446,#7127,#789,.T.);
#9506=EDGE_CURVE('',#7411,#7447,#790,.T.);
#9507=EDGE_CURVE('',#7447,#7417,#791,.T.);
#9508=EDGE_CURVE('',#7418,#7448,#792,.T.);
#9509=EDGE_CURVE('',#7448,#7407,#793,.T.);
#9510=EDGE_CURVE('',#7426,#7449,#794,.T.);
#9511=EDGE_CURVE('',#7449,#7413,#795,.T.);
#9512=EDGE_CURVE('',#7412,#7450,#796,.T.);
#9513=EDGE_CURVE('',#7450,#7422,#797,.T.);
#9514=EDGE_CURVE('',#7187,#7451,#798,.T.);
#9515=EDGE_CURVE('',#7451,#7452,#799,.T.);
#9516=EDGE_CURVE('',#7452,#7453,#800,.F.);
#9517=EDGE_CURVE('',#7453,#7454,#801,.T.);
#9518=EDGE_CURVE('',#7454,#7455,#71,.T.);
#9519=EDGE_CURVE('',#7455,#7456,#802,.T.);
#9520=EDGE_CURVE('',#7456,#7187,#803,.T.);
#9521=EDGE_CURVE('',#7457,#7458,#2083,.T.);
#9522=EDGE_CURVE('',#7458,#7459,#804,.T.);
#9523=EDGE_CURVE('',#7459,#7460,#805,.T.);
#9524=EDGE_CURVE('',#7460,#7461,#806,.T.);
#9525=EDGE_CURVE('',#7461,#7462,#807,.T.);
#9526=EDGE_CURVE('',#7462,#7463,#2084,.T.);
#9527=EDGE_CURVE('',#7463,#7457,#808,.T.);
#9528=EDGE_CURVE('',#7462,#7464,#809,.T.);
#9529=EDGE_CURVE('',#7464,#7465,#810,.T.);
#9530=EDGE_CURVE('',#7465,#7466,#811,.T.);
#9531=EDGE_CURVE('',#7466,#7467,#812,.T.);
#9532=EDGE_CURVE('',#7467,#7468,#813,.T.);
#9533=EDGE_CURVE('',#7468,#7469,#2085,.T.);
#9534=EDGE_CURVE('',#7469,#7470,#814,.T.);
#9535=EDGE_CURVE('',#7470,#7471,#815,.T.);
#9536=EDGE_CURVE('',#7471,#7472,#816,.T.);
#9537=EDGE_CURVE('',#7472,#7473,#817,.T.);
#9538=EDGE_CURVE('',#7473,#7463,#818,.T.);
#9539=EDGE_CURVE('',#7474,#7475,#2086,.T.);
#9540=EDGE_CURVE('',#7475,#7476,#819,.T.);
#9541=EDGE_CURVE('',#7476,#7477,#820,.T.);
#9542=EDGE_CURVE('',#7477,#7478,#821,.T.);
#9543=EDGE_CURVE('',#7478,#7479,#822,.T.);
#9544=EDGE_CURVE('',#7479,#7458,#823,.T.);
#9545=EDGE_CURVE('',#7457,#7480,#824,.T.);
#9546=EDGE_CURVE('',#7480,#7481,#825,.T.);
#9547=EDGE_CURVE('',#7481,#7482,#826,.T.);
#9548=EDGE_CURVE('',#7482,#7483,#827,.T.);
#9549=EDGE_CURVE('',#7483,#7474,#828,.T.);
#9550=EDGE_CURVE('',#7468,#7484,#829,.T.);
#9551=EDGE_CURVE('',#7484,#7485,#830,.T.);
#9552=EDGE_CURVE('',#7485,#7486,#831,.T.);
#9553=EDGE_CURVE('',#7486,#7475,#832,.T.);
#9554=EDGE_CURVE('',#7474,#7469,#833,.T.);
#9555=EDGE_CURVE('',#7451,#7487,#834,.T.);
#9556=EDGE_CURVE('',#7487,#7488,#6086,.T.);
#9557=EDGE_CURVE('',#7488,#7452,#835,.T.);
#9558=EDGE_CURVE('',#7455,#7489,#836,.T.);
#9559=EDGE_CURVE('',#7489,#7490,#837,.T.);
#9560=EDGE_CURVE('',#7490,#7456,#838,.T.);
#9561=EDGE_CURVE('',#7491,#7492,#6087,.T.);
#9562=EDGE_CURVE('',#7492,#7446,#839,.T.);
#9563=EDGE_CURVE('',#7445,#7491,#840,.T.);
#9564=EDGE_CURVE('',#7441,#7493,#841,.T.);
#9565=EDGE_CURVE('',#7493,#7494,#6088,.T.);
#9566=EDGE_CURVE('',#7494,#7442,#842,.T.);
#9567=EDGE_CURVE('',#7407,#7434,#6089,.T.);
#9568=EDGE_CURVE('',#7435,#7418,#6090,.T.);
#9569=EDGE_CURVE('',#7436,#7421,#843,.F.);
#9570=EDGE_CURVE('',#7433,#7408,#6091,.F.);
#9571=EDGE_CURVE('',#7420,#7489,#844,.F.);
#9572=EDGE_CURVE('',#7437,#7454,#845,.T.);
#9573=EDGE_CURVE('',#7494,#7433,#6092,.F.);
#9574=EDGE_CURVE('',#7443,#7432,#846,.T.);
#9575=EDGE_CURVE('',#7438,#7453,#847,.F.);
#9576=EDGE_CURVE('',#7444,#6976,#848,.F.);
#9577=EDGE_CURVE('',#7488,#7439,#6093,.F.);
#9578=EDGE_CURVE('',#6975,#7491,#6094,.T.);
#9579=EDGE_CURVE('',#7439,#7423,#6095,.F.);
#9580=EDGE_CURVE('',#7440,#7422,#6096,.F.);
#9581=EDGE_CURVE('',#7416,#6975,#6097,.F.);
#9582=EDGE_CURVE('',#7412,#6974,#6098,.F.);
#9583=EDGE_CURVE('',#7457,#7428,#849,.T.);
#9584=EDGE_CURVE('',#7430,#7463,#850,.T.);
#9585=EDGE_CURVE('',#7431,#7469,#851,.F.);
#9586=EDGE_CURVE('',#7474,#6978,#852,.F.);
#9587=EDGE_CURVE('',#7491,#7416,#6099,.T.);
#9588=EDGE_CURVE('',#7415,#7492,#6100,.F.);
#9589=EDGE_CURVE('',#7130,#7415,#6101,.T.);
#9590=EDGE_CURVE('',#7131,#7413,#6102,.F.);
#9591=EDGE_CURVE('',#7183,#7426,#6103,.T.);
#9592=EDGE_CURVE('',#7424,#7184,#6104,.T.);
#9593=EDGE_CURVE('',#7193,#7493,#6105,.F.);
#9594=EDGE_CURVE('',#7125,#7441,#853,.T.);
#9595=EDGE_CURVE('',#7129,#7446,#854,.F.);
#9596=EDGE_CURVE('',#7130,#7492,#6106,.T.);
#9597=EDGE_CURVE('',#7451,#7185,#855,.F.);
#9598=EDGE_CURVE('',#7487,#7184,#6107,.T.);
#9599=EDGE_CURVE('',#7487,#7424,#6108,.T.);
#9600=EDGE_CURVE('',#7488,#7423,#6109,.T.);
#9601=EDGE_CURVE('',#7189,#7456,#856,.F.);
#9602=EDGE_CURVE('',#7190,#7490,#857,.T.);
#9603=EDGE_CURVE('',#7191,#7417,#6110,.F.);
#9604=EDGE_CURVE('',#7192,#7411,#6111,.T.);
#9605=EDGE_CURVE('',#7193,#7409,#6112,.F.);
#9606=EDGE_CURVE('',#7493,#7409,#6113,.T.);
#9607=EDGE_CURVE('',#7494,#7408,#6114,.T.);
#9608=EDGE_CURVE('',#6981,#7475,#6115,.F.);
#9609=EDGE_CURVE('',#7458,#6984,#6116,.F.);
#9610=EDGE_CURVE('',#7462,#6983,#6117,.T.);
#9611=EDGE_CURVE('',#6982,#7468,#6118,.T.);
#9612=EDGE_CURVE('',#7427,#7174,#858,.T.);
#9613=EDGE_CURVE('',#7140,#7495,#859,.T.);
#9614=EDGE_CURVE('',#7495,#7496,#860,.F.);
#9615=EDGE_CURVE('',#7496,#7497,#6119,.F.);
#9616=EDGE_CURVE('',#7497,#7498,#861,.T.);
#9617=EDGE_CURVE('',#7498,#7499,#6120,.F.);
#9618=EDGE_CURVE('',#7499,#7500,#862,.F.);
#9619=EDGE_CURVE('',#7500,#7141,#863,.F.);
#9620=EDGE_CURVE('',#7501,#7502,#864,.T.);
#9621=EDGE_CURVE('',#7502,#7503,#865,.T.);
#9622=EDGE_CURVE('',#7503,#7504,#866,.T.);
#9623=EDGE_CURVE('',#7504,#7505,#867,.T.);
#9624=EDGE_CURVE('',#7505,#7506,#868,.T.);
#9625=EDGE_CURVE('',#7506,#7501,#869,.T.);
#9626=EDGE_CURVE('',#7507,#7508,#870,.T.);
#9627=EDGE_CURVE('',#7508,#7509,#871,.T.);
#9628=EDGE_CURVE('',#7509,#7510,#872,.T.);
#9629=EDGE_CURVE('',#7510,#7511,#873,.T.);
#9630=EDGE_CURVE('',#7511,#7512,#874,.T.);
#9631=EDGE_CURVE('',#7512,#7507,#875,.T.);
#9632=EDGE_CURVE('',#7513,#7514,#876,.T.);
#9633=EDGE_CURVE('',#7514,#7515,#877,.T.);
#9634=EDGE_CURVE('',#7515,#7516,#878,.T.);
#9635=EDGE_CURVE('',#7516,#7517,#879,.T.);
#9636=EDGE_CURVE('',#7517,#7518,#880,.T.);
#9637=EDGE_CURVE('',#7518,#7513,#881,.T.);
#9638=EDGE_CURVE('',#7519,#7520,#882,.T.);
#9639=EDGE_CURVE('',#7520,#7521,#883,.T.);
#9640=EDGE_CURVE('',#7521,#7522,#884,.T.);
#9641=EDGE_CURVE('',#7522,#7523,#885,.T.);
#9642=EDGE_CURVE('',#7523,#7524,#886,.T.);
#9643=EDGE_CURVE('',#7524,#7519,#887,.T.);
#9644=EDGE_CURVE('',#7525,#7526,#888,.T.);
#9645=EDGE_CURVE('',#7526,#7527,#889,.T.);
#9646=EDGE_CURVE('',#7527,#7528,#890,.T.);
#9647=EDGE_CURVE('',#7528,#7529,#891,.T.);
#9648=EDGE_CURVE('',#7529,#7530,#892,.T.);
#9649=EDGE_CURVE('',#7530,#7525,#893,.T.);
#9650=EDGE_CURVE('',#7531,#7532,#894,.T.);
#9651=EDGE_CURVE('',#7532,#7533,#895,.T.);
#9652=EDGE_CURVE('',#7533,#7534,#896,.T.);
#9653=EDGE_CURVE('',#7534,#7535,#897,.T.);
#9654=EDGE_CURVE('',#7535,#7536,#898,.T.);
#9655=EDGE_CURVE('',#7536,#7531,#899,.T.);
#9656=EDGE_CURVE('',#7537,#7538,#900,.T.);
#9657=EDGE_CURVE('',#7538,#7539,#901,.T.);
#9658=EDGE_CURVE('',#7539,#7540,#902,.T.);
#9659=EDGE_CURVE('',#7540,#7541,#903,.T.);
#9660=EDGE_CURVE('',#7541,#7542,#904,.T.);
#9661=EDGE_CURVE('',#7542,#7537,#905,.T.);
#9662=EDGE_CURVE('',#7543,#7544,#906,.T.);
#9663=EDGE_CURVE('',#7544,#7545,#907,.T.);
#9664=EDGE_CURVE('',#7545,#7546,#908,.T.);
#9665=EDGE_CURVE('',#7546,#7547,#909,.T.);
#9666=EDGE_CURVE('',#7547,#7548,#910,.T.);
#9667=EDGE_CURVE('',#7548,#7543,#911,.T.);
#9668=EDGE_CURVE('',#7549,#7550,#912,.T.);
#9669=EDGE_CURVE('',#7550,#7551,#913,.T.);
#9670=EDGE_CURVE('',#7551,#7552,#914,.T.);
#9671=EDGE_CURVE('',#7552,#7553,#915,.T.);
#9672=EDGE_CURVE('',#7553,#7554,#916,.T.);
#9673=EDGE_CURVE('',#7554,#7549,#917,.T.);
#9674=EDGE_CURVE('',#7555,#7556,#918,.T.);
#9675=EDGE_CURVE('',#7556,#7557,#919,.T.);
#9676=EDGE_CURVE('',#7557,#7558,#920,.T.);
#9677=EDGE_CURVE('',#7558,#7559,#921,.T.);
#9678=EDGE_CURVE('',#7559,#7560,#922,.T.);
#9679=EDGE_CURVE('',#7560,#7555,#923,.T.);
#9680=EDGE_CURVE('',#7561,#7562,#924,.T.);
#9681=EDGE_CURVE('',#7562,#7563,#925,.T.);
#9682=EDGE_CURVE('',#7563,#7564,#926,.T.);
#9683=EDGE_CURVE('',#7564,#7565,#927,.T.);
#9684=EDGE_CURVE('',#7565,#7566,#928,.T.);
#9685=EDGE_CURVE('',#7566,#7561,#929,.T.);
#9686=EDGE_CURVE('',#7567,#7568,#930,.T.);
#9687=EDGE_CURVE('',#7568,#7569,#931,.T.);
#9688=EDGE_CURVE('',#7569,#7570,#932,.T.);
#9689=EDGE_CURVE('',#7570,#7571,#933,.T.);
#9690=EDGE_CURVE('',#7571,#7572,#934,.T.);
#9691=EDGE_CURVE('',#7572,#7567,#935,.T.);
#9692=EDGE_CURVE('',#7573,#7574,#936,.T.);
#9693=EDGE_CURVE('',#7574,#7575,#937,.T.);
#9694=EDGE_CURVE('',#7575,#7576,#938,.T.);
#9695=EDGE_CURVE('',#7576,#7577,#939,.T.);
#9696=EDGE_CURVE('',#7577,#7578,#940,.T.);
#9697=EDGE_CURVE('',#7578,#7573,#941,.T.);
#9698=EDGE_CURVE('',#7579,#7580,#942,.T.);
#9699=EDGE_CURVE('',#7580,#7581,#943,.T.);
#9700=EDGE_CURVE('',#7581,#7582,#944,.T.);
#9701=EDGE_CURVE('',#7582,#7583,#945,.T.);
#9702=EDGE_CURVE('',#7583,#7584,#946,.T.);
#9703=EDGE_CURVE('',#7584,#7579,#947,.T.);
#9704=EDGE_CURVE('',#7585,#7586,#948,.T.);
#9705=EDGE_CURVE('',#7586,#7587,#949,.T.);
#9706=EDGE_CURVE('',#7587,#7588,#950,.T.);
#9707=EDGE_CURVE('',#7588,#7589,#951,.T.);
#9708=EDGE_CURVE('',#7589,#7590,#952,.T.);
#9709=EDGE_CURVE('',#7590,#7585,#953,.T.);
#9710=EDGE_CURVE('',#7591,#7592,#954,.T.);
#9711=EDGE_CURVE('',#7592,#7593,#955,.T.);
#9712=EDGE_CURVE('',#7593,#7594,#956,.T.);
#9713=EDGE_CURVE('',#7594,#7595,#957,.T.);
#9714=EDGE_CURVE('',#7595,#7596,#958,.T.);
#9715=EDGE_CURVE('',#7596,#7591,#959,.T.);
#9716=EDGE_CURVE('',#7597,#7598,#960,.T.);
#9717=EDGE_CURVE('',#7598,#7599,#961,.T.);
#9718=EDGE_CURVE('',#7599,#7600,#962,.T.);
#9719=EDGE_CURVE('',#7600,#7601,#963,.T.);
#9720=EDGE_CURVE('',#7601,#7602,#964,.T.);
#9721=EDGE_CURVE('',#7602,#7597,#965,.T.);
#9722=EDGE_CURVE('',#7170,#7180,#966,.T.);
#9723=EDGE_CURVE('',#7171,#7182,#967,.F.);
#9724=EDGE_CURVE('',#7603,#7604,#968,.F.);
#9725=EDGE_CURVE('',#7605,#7603,#969,.F.);
#9726=EDGE_CURVE('',#7606,#7605,#970,.F.);
#9727=EDGE_CURVE('',#7607,#7606,#971,.F.);
#9728=EDGE_CURVE('',#7608,#7607,#972,.F.);
#9729=EDGE_CURVE('',#7604,#7608,#973,.F.);
#9730=EDGE_CURVE('',#7609,#7610,#974,.F.);
#9731=EDGE_CURVE('',#7611,#7609,#975,.F.);
#9732=EDGE_CURVE('',#7612,#7611,#976,.F.);
#9733=EDGE_CURVE('',#7613,#7612,#977,.F.);
#9734=EDGE_CURVE('',#7614,#7613,#978,.F.);
#9735=EDGE_CURVE('',#7610,#7614,#979,.F.);
#9736=EDGE_CURVE('',#7615,#7616,#980,.F.);
#9737=EDGE_CURVE('',#7617,#7615,#981,.F.);
#9738=EDGE_CURVE('',#7618,#7617,#982,.F.);
#9739=EDGE_CURVE('',#7619,#7618,#983,.F.);
#9740=EDGE_CURVE('',#7620,#7619,#984,.F.);
#9741=EDGE_CURVE('',#7616,#7620,#985,.F.);
#9742=EDGE_CURVE('',#7621,#7622,#986,.F.);
#9743=EDGE_CURVE('',#7623,#7621,#987,.F.);
#9744=EDGE_CURVE('',#7624,#7623,#988,.F.);
#9745=EDGE_CURVE('',#7625,#7624,#989,.F.);
#9746=EDGE_CURVE('',#7626,#7625,#990,.F.);
#9747=EDGE_CURVE('',#7622,#7626,#991,.F.);
#9748=EDGE_CURVE('',#7627,#7628,#992,.F.);
#9749=EDGE_CURVE('',#7629,#7627,#993,.F.);
#9750=EDGE_CURVE('',#7630,#7629,#994,.F.);
#9751=EDGE_CURVE('',#7631,#7630,#995,.F.);
#9752=EDGE_CURVE('',#7632,#7631,#996,.F.);
#9753=EDGE_CURVE('',#7628,#7632,#997,.F.);
#9754=EDGE_CURVE('',#7633,#7634,#998,.F.);
#9755=EDGE_CURVE('',#7635,#7633,#999,.F.);
#9756=EDGE_CURVE('',#7636,#7635,#1000,.F.);
#9757=EDGE_CURVE('',#7637,#7636,#1001,.F.);
#9758=EDGE_CURVE('',#7638,#7637,#1002,.F.);
#9759=EDGE_CURVE('',#7634,#7638,#1003,.F.);
#9760=EDGE_CURVE('',#7639,#7640,#1004,.F.);
#9761=EDGE_CURVE('',#7641,#7639,#1005,.F.);
#9762=EDGE_CURVE('',#7642,#7641,#1006,.F.);
#9763=EDGE_CURVE('',#7643,#7642,#1007,.F.);
#9764=EDGE_CURVE('',#7644,#7643,#1008,.F.);
#9765=EDGE_CURVE('',#7640,#7644,#1009,.F.);
#9766=EDGE_CURVE('',#7645,#7646,#1010,.F.);
#9767=EDGE_CURVE('',#7647,#7645,#1011,.F.);
#9768=EDGE_CURVE('',#7648,#7647,#1012,.F.);
#9769=EDGE_CURVE('',#7649,#7648,#1013,.F.);
#9770=EDGE_CURVE('',#7650,#7649,#1014,.F.);
#9771=EDGE_CURVE('',#7646,#7650,#1015,.F.);
#9772=EDGE_CURVE('',#7651,#7652,#1016,.F.);
#9773=EDGE_CURVE('',#7653,#7651,#1017,.F.);
#9774=EDGE_CURVE('',#7654,#7653,#1018,.F.);
#9775=EDGE_CURVE('',#7655,#7654,#1019,.F.);
#9776=EDGE_CURVE('',#7656,#7655,#1020,.F.);
#9777=EDGE_CURVE('',#7652,#7656,#1021,.F.);
#9778=EDGE_CURVE('',#7657,#7658,#1022,.F.);
#9779=EDGE_CURVE('',#7659,#7657,#1023,.F.);
#9780=EDGE_CURVE('',#7660,#7659,#1024,.F.);
#9781=EDGE_CURVE('',#7661,#7660,#1025,.F.);
#9782=EDGE_CURVE('',#7662,#7661,#1026,.F.);
#9783=EDGE_CURVE('',#7658,#7662,#1027,.F.);
#9784=EDGE_CURVE('',#7663,#7664,#1028,.F.);
#9785=EDGE_CURVE('',#7665,#7663,#1029,.F.);
#9786=EDGE_CURVE('',#7666,#7665,#1030,.F.);
#9787=EDGE_CURVE('',#7667,#7666,#1031,.F.);
#9788=EDGE_CURVE('',#7668,#7667,#1032,.F.);
#9789=EDGE_CURVE('',#7664,#7668,#1033,.F.);
#9790=EDGE_CURVE('',#7669,#7670,#1034,.F.);
#9791=EDGE_CURVE('',#7671,#7669,#1035,.F.);
#9792=EDGE_CURVE('',#7672,#7671,#1036,.F.);
#9793=EDGE_CURVE('',#7673,#7672,#1037,.F.);
#9794=EDGE_CURVE('',#7674,#7673,#1038,.F.);
#9795=EDGE_CURVE('',#7670,#7674,#1039,.F.);
#9796=EDGE_CURVE('',#7675,#7676,#1040,.F.);
#9797=EDGE_CURVE('',#7677,#7675,#1041,.F.);
#9798=EDGE_CURVE('',#7678,#7677,#1042,.F.);
#9799=EDGE_CURVE('',#7679,#7678,#1043,.F.);
#9800=EDGE_CURVE('',#7680,#7679,#1044,.F.);
#9801=EDGE_CURVE('',#7676,#7680,#1045,.F.);
#9802=EDGE_CURVE('',#7681,#7682,#1046,.F.);
#9803=EDGE_CURVE('',#7683,#7681,#1047,.F.);
#9804=EDGE_CURVE('',#7684,#7683,#1048,.F.);
#9805=EDGE_CURVE('',#7685,#7684,#1049,.F.);
#9806=EDGE_CURVE('',#7686,#7685,#1050,.F.);
#9807=EDGE_CURVE('',#7682,#7686,#1051,.F.);
#9808=EDGE_CURVE('',#7687,#7688,#1052,.F.);
#9809=EDGE_CURVE('',#7689,#7687,#1053,.F.);
#9810=EDGE_CURVE('',#7690,#7689,#1054,.F.);
#9811=EDGE_CURVE('',#7691,#7690,#1055,.F.);
#9812=EDGE_CURVE('',#7692,#7691,#1056,.F.);
#9813=EDGE_CURVE('',#7688,#7692,#1057,.F.);
#9814=EDGE_CURVE('',#7693,#7694,#1058,.F.);
#9815=EDGE_CURVE('',#7695,#7693,#1059,.F.);
#9816=EDGE_CURVE('',#7696,#7695,#1060,.F.);
#9817=EDGE_CURVE('',#7697,#7696,#1061,.F.);
#9818=EDGE_CURVE('',#7698,#7697,#1062,.F.);
#9819=EDGE_CURVE('',#7694,#7698,#1063,.F.);
#9820=EDGE_CURVE('',#7699,#7700,#1064,.F.);
#9821=EDGE_CURVE('',#7701,#7699,#1065,.F.);
#9822=EDGE_CURVE('',#7702,#7701,#1066,.F.);
#9823=EDGE_CURVE('',#7703,#7702,#1067,.F.);
#9824=EDGE_CURVE('',#7704,#7703,#1068,.F.);
#9825=EDGE_CURVE('',#7700,#7704,#1069,.F.);
#9826=EDGE_CURVE('',#7282,#7505,#1070,.F.);
#9827=EDGE_CURVE('',#7506,#7281,#1071,.T.);
#9828=EDGE_CURVE('',#7501,#7280,#1072,.T.);
#9829=EDGE_CURVE('',#7277,#7504,#1073,.T.);
#9830=EDGE_CURVE('',#7502,#7279,#1074,.T.);
#9831=EDGE_CURVE('',#7278,#7503,#1075,.F.);
#9832=EDGE_CURVE('',#7288,#7511,#1076,.F.);
#9833=EDGE_CURVE('',#7512,#7287,#1077,.T.);
#9834=EDGE_CURVE('',#7507,#7286,#1078,.T.);
#9835=EDGE_CURVE('',#7283,#7510,#1079,.T.);
#9836=EDGE_CURVE('',#7508,#7285,#1080,.T.);
#9837=EDGE_CURVE('',#7284,#7509,#1081,.F.);
#9838=EDGE_CURVE('',#7294,#7517,#1082,.F.);
#9839=EDGE_CURVE('',#7518,#7293,#1083,.T.);
#9840=EDGE_CURVE('',#7513,#7292,#1084,.T.);
#9841=EDGE_CURVE('',#7289,#7516,#1085,.T.);
#9842=EDGE_CURVE('',#7514,#7291,#1086,.T.);
#9843=EDGE_CURVE('',#7290,#7515,#1087,.F.);
#9844=EDGE_CURVE('',#7300,#7523,#1088,.F.);
#9845=EDGE_CURVE('',#7524,#7299,#1089,.T.);
#9846=EDGE_CURVE('',#7519,#7298,#1090,.T.);
#9847=EDGE_CURVE('',#7295,#7522,#1091,.T.);
#9848=EDGE_CURVE('',#7520,#7297,#1092,.T.);
#9849=EDGE_CURVE('',#7296,#7521,#1093,.F.);
#9850=EDGE_CURVE('',#7306,#7529,#1094,.F.);
#9851=EDGE_CURVE('',#7530,#7305,#1095,.T.);
#9852=EDGE_CURVE('',#7525,#7304,#1096,.T.);
#9853=EDGE_CURVE('',#7301,#7528,#1097,.T.);
#9854=EDGE_CURVE('',#7526,#7303,#1098,.T.);
#9855=EDGE_CURVE('',#7302,#7527,#1099,.F.);
#9856=EDGE_CURVE('',#7312,#7535,#1100,.F.);
#9857=EDGE_CURVE('',#7536,#7311,#1101,.T.);
#9858=EDGE_CURVE('',#7531,#7310,#1102,.T.);
#9859=EDGE_CURVE('',#7307,#7534,#1103,.T.);
#9860=EDGE_CURVE('',#7532,#7309,#1104,.T.);
#9861=EDGE_CURVE('',#7308,#7533,#1105,.F.);
#9862=EDGE_CURVE('',#7321,#7541,#1106,.F.);
#9863=EDGE_CURVE('',#7542,#7319,#1107,.T.);
#9864=EDGE_CURVE('',#7537,#7318,#1108,.T.);
#9865=EDGE_CURVE('',#7313,#7540,#1109,.T.);
#9866=EDGE_CURVE('',#7538,#7316,#1110,.T.);
#9867=EDGE_CURVE('',#7314,#7539,#1111,.F.);
#9868=EDGE_CURVE('',#7328,#7547,#1112,.F.);
#9869=EDGE_CURVE('',#7548,#7327,#1113,.T.);
#9870=EDGE_CURVE('',#7543,#7326,#1114,.T.);
#9871=EDGE_CURVE('',#7323,#7546,#1115,.T.);
#9872=EDGE_CURVE('',#7544,#7325,#1116,.T.);
#9873=EDGE_CURVE('',#7324,#7545,#1117,.F.);
#9874=EDGE_CURVE('',#7334,#7553,#1118,.F.);
#9875=EDGE_CURVE('',#7554,#7333,#1119,.T.);
#9876=EDGE_CURVE('',#7549,#7332,#1120,.T.);
#9877=EDGE_CURVE('',#7329,#7552,#1121,.T.);
#9878=EDGE_CURVE('',#7550,#7331,#1122,.T.);
#9879=EDGE_CURVE('',#7330,#7551,#1123,.F.);
#9880=EDGE_CURVE('',#7340,#7559,#1124,.F.);
#9881=EDGE_CURVE('',#7560,#7339,#1125,.T.);
#9882=EDGE_CURVE('',#7555,#7338,#1126,.T.);
#9883=EDGE_CURVE('',#7335,#7558,#1127,.T.);
#9884=EDGE_CURVE('',#7556,#7337,#1128,.T.);
#9885=EDGE_CURVE('',#7336,#7557,#1129,.F.);
#9886=EDGE_CURVE('',#7346,#7565,#1130,.F.);
#9887=EDGE_CURVE('',#7566,#7345,#1131,.T.);
#9888=EDGE_CURVE('',#7561,#7344,#1132,.T.);
#9889=EDGE_CURVE('',#7341,#7564,#1133,.T.);
#9890=EDGE_CURVE('',#7562,#7343,#1134,.T.);
#9891=EDGE_CURVE('',#7342,#7563,#1135,.F.);
#9892=EDGE_CURVE('',#7352,#7571,#1136,.F.);
#9893=EDGE_CURVE('',#7572,#7351,#1137,.T.);
#9894=EDGE_CURVE('',#7567,#7350,#1138,.T.);
#9895=EDGE_CURVE('',#7347,#7570,#1139,.T.);
#9896=EDGE_CURVE('',#7568,#7349,#1140,.T.);
#9897=EDGE_CURVE('',#7348,#7569,#1141,.F.);
#9898=EDGE_CURVE('',#7361,#7577,#1142,.F.);
#9899=EDGE_CURVE('',#7578,#7359,#1143,.T.);
#9900=EDGE_CURVE('',#7573,#7358,#1144,.T.);
#9901=EDGE_CURVE('',#7353,#7576,#1145,.T.);
#9902=EDGE_CURVE('',#7574,#7356,#1146,.T.);
#9903=EDGE_CURVE('',#7354,#7575,#1147,.F.);
#9904=EDGE_CURVE('',#7371,#7583,#1148,.F.);
#9905=EDGE_CURVE('',#7584,#7369,#1149,.T.);
#9906=EDGE_CURVE('',#7579,#7368,#1150,.T.);
#9907=EDGE_CURVE('',#7363,#7582,#1151,.F.);
#9908=EDGE_CURVE('',#7580,#7366,#1152,.T.);
#9909=EDGE_CURVE('',#7364,#7581,#1153,.F.);
#9910=EDGE_CURVE('',#7381,#7589,#1154,.T.);
#9911=EDGE_CURVE('',#7590,#7380,#1155,.T.);
#9912=EDGE_CURVE('',#7585,#7379,#1156,.T.);
#9913=EDGE_CURVE('',#7373,#7588,#1157,.F.);
#9914=EDGE_CURVE('',#7586,#7377,#1158,.T.);
#9915=EDGE_CURVE('',#7375,#7587,#1159,.F.);
#9916=EDGE_CURVE('',#7391,#7595,#1160,.F.);
#9917=EDGE_CURVE('',#7596,#7389,#1161,.T.);
#9918=EDGE_CURVE('',#7591,#7388,#1162,.F.);
#9919=EDGE_CURVE('',#7385,#7594,#1163,.T.);
#9920=EDGE_CURVE('',#7592,#7387,#1164,.T.);
#9921=EDGE_CURVE('',#7386,#7593,#1165,.F.);
#9922=EDGE_CURVE('',#7403,#7601,#1166,.T.);
#9923=EDGE_CURVE('',#7602,#7401,#1167,.T.);
#9924=EDGE_CURVE('',#7597,#7400,#1168,.T.);
#9925=EDGE_CURVE('',#7393,#7600,#1169,.F.);
#9926=EDGE_CURVE('',#7598,#7396,#1170,.F.);
#9927=EDGE_CURVE('',#7394,#7599,#1171,.F.);
#9928=EDGE_CURVE('',#7209,#7604,#1172,.T.);
#9929=EDGE_CURVE('',#7603,#7084,#1173,.T.);
#9930=EDGE_CURVE('',#7605,#7083,#1174,.T.);
#9931=EDGE_CURVE('',#7210,#7608,#1175,.F.);
#9932=EDGE_CURVE('',#7606,#7082,#1176,.T.);
#9933=EDGE_CURVE('',#7081,#7607,#1177,.F.);
#9934=EDGE_CURVE('',#7211,#7610,#1178,.T.);
#9935=EDGE_CURVE('',#7609,#7078,#1179,.T.);
#9936=EDGE_CURVE('',#7611,#7077,#1180,.T.);
#9937=EDGE_CURVE('',#7212,#7614,#1181,.F.);
#9938=EDGE_CURVE('',#7612,#7076,#1182,.T.);
#9939=EDGE_CURVE('',#7075,#7613,#1183,.F.);
#9940=EDGE_CURVE('',#7213,#7616,#1184,.T.);
#9941=EDGE_CURVE('',#7615,#7072,#1185,.T.);
#9942=EDGE_CURVE('',#7617,#7071,#1186,.T.);
#9943=EDGE_CURVE('',#7214,#7620,#1187,.F.);
#9944=EDGE_CURVE('',#7618,#7070,#1188,.T.);
#9945=EDGE_CURVE('',#7069,#7619,#1189,.F.);
#9946=EDGE_CURVE('',#7215,#7622,#1190,.T.);
#9947=EDGE_CURVE('',#7621,#7066,#1191,.T.);
#9948=EDGE_CURVE('',#7623,#7065,#1192,.T.);
#9949=EDGE_CURVE('',#7216,#7626,#1193,.F.);
#9950=EDGE_CURVE('',#7624,#7064,#1194,.T.);
#9951=EDGE_CURVE('',#7063,#7625,#1195,.F.);
#9952=EDGE_CURVE('',#7199,#7628,#1196,.T.);
#9953=EDGE_CURVE('',#7627,#7114,#1197,.T.);
#9954=EDGE_CURVE('',#7629,#7113,#1198,.T.);
#9955=EDGE_CURVE('',#7200,#7632,#1199,.F.);
#9956=EDGE_CURVE('',#7630,#7112,#1200,.T.);
#9957=EDGE_CURVE('',#7111,#7631,#1201,.F.);
#9958=EDGE_CURVE('',#7219,#7634,#1202,.T.);
#9959=EDGE_CURVE('',#7633,#7054,#1203,.T.);
#9960=EDGE_CURVE('',#7635,#7053,#1204,.T.);
#9961=EDGE_CURVE('',#7220,#7638,#1205,.F.);
#9962=EDGE_CURVE('',#7636,#7052,#1206,.T.);
#9963=EDGE_CURVE('',#7051,#7637,#1207,.F.);
#9964=EDGE_CURVE('',#7237,#7640,#1208,.T.);
#9965=EDGE_CURVE('',#7639,#7014,#1209,.T.);
#9966=EDGE_CURVE('',#7641,#7012,#1210,.T.);
#9967=EDGE_CURVE('',#7238,#7644,#1211,.F.);
#9968=EDGE_CURVE('',#7642,#7011,#1212,.F.);
#9969=EDGE_CURVE('',#7009,#7643,#1213,.F.);
#9970=EDGE_CURVE('',#7217,#7646,#1214,.T.);
#9971=EDGE_CURVE('',#7645,#7060,#1215,.T.);
#9972=EDGE_CURVE('',#7647,#7059,#1216,.T.);
#9973=EDGE_CURVE('',#7218,#7650,#1217,.F.);
#9974=EDGE_CURVE('',#7648,#7058,#1218,.T.);
#9975=EDGE_CURVE('',#7057,#7649,#1219,.F.);
#9976=EDGE_CURVE('',#7207,#7652,#1220,.T.);
#9977=EDGE_CURVE('',#7651,#7090,#1221,.T.);
#9978=EDGE_CURVE('',#7653,#7089,#1222,.T.);
#9979=EDGE_CURVE('',#7208,#7656,#1223,.F.);
#9980=EDGE_CURVE('',#7654,#7088,#1224,.T.);
#9981=EDGE_CURVE('',#7087,#7655,#1225,.F.);
#9982=EDGE_CURVE('',#7205,#7658,#1226,.T.);
#9983=EDGE_CURVE('',#7657,#7096,#1227,.T.);
#9984=EDGE_CURVE('',#7659,#7095,#1228,.T.);
#9985=EDGE_CURVE('',#7206,#7662,#1229,.F.);
#9986=EDGE_CURVE('',#7660,#7094,#1230,.T.);
#9987=EDGE_CURVE('',#7093,#7661,#1231,.F.);
#9988=EDGE_CURVE('',#7203,#7664,#1232,.T.);
#9989=EDGE_CURVE('',#7663,#7102,#1233,.T.);
#9990=EDGE_CURVE('',#7665,#7101,#1234,.T.);
#9991=EDGE_CURVE('',#7204,#7668,#1235,.F.);
#9992=EDGE_CURVE('',#7666,#7100,#1236,.T.);
#9993=EDGE_CURVE('',#7099,#7667,#1237,.F.);
#9994=EDGE_CURVE('',#7201,#7670,#1238,.T.);
#9995=EDGE_CURVE('',#7669,#7108,#1239,.T.);
#9996=EDGE_CURVE('',#7671,#7107,#1240,.T.);
#9997=EDGE_CURVE('',#7202,#7674,#1241,.F.);
#9998=EDGE_CURVE('',#7672,#7106,#1242,.T.);
#9999=EDGE_CURVE('',#7105,#7673,#1243,.F.);
#10000=EDGE_CURVE('',#7233,#7676,#1244,.T.);
#10001=EDGE_CURVE('',#7675,#7022,#1245,.T.);
#10002=EDGE_CURVE('',#7677,#7020,#1246,.T.);
#10003=EDGE_CURVE('',#7234,#7680,#1247,.F.);
#10004=EDGE_CURVE('',#7678,#7019,#1248,.T.);
#10005=EDGE_CURVE('',#7017,#7679,#1249,.F.);
#10006=EDGE_CURVE('',#7229,#7682,#1250,.F.);
#10007=EDGE_CURVE('',#7681,#7030,#1251,.T.);
#10008=EDGE_CURVE('',#7683,#7028,#1252,.T.);
#10009=EDGE_CURVE('',#7230,#7686,#1253,.F.);
#10010=EDGE_CURVE('',#7684,#7027,#1254,.T.);
#10011=EDGE_CURVE('',#7025,#7685,#1255,.F.);
#10012=EDGE_CURVE('',#7225,#7688,#1256,.F.);
#10013=EDGE_CURVE('',#7687,#7041,#1257,.T.);
#10014=EDGE_CURVE('',#7689,#7039,#1258,.T.);
#10015=EDGE_CURVE('',#7227,#7692,#1259,.F.);
#10016=EDGE_CURVE('',#7690,#7037,#1260,.T.);
#10017=EDGE_CURVE('',#7033,#7691,#1261,.T.);
#10018=EDGE_CURVE('',#7221,#7694,#1262,.T.);
#10019=EDGE_CURVE('',#7693,#7048,#1263,.T.);
#10020=EDGE_CURVE('',#7695,#7047,#1264,.T.);
#10021=EDGE_CURVE('',#7222,#7698,#1265,.F.);
#10022=EDGE_CURVE('',#7696,#7046,#1266,.F.);
#10023=EDGE_CURVE('',#7044,#7697,#1267,.F.);
#10024=EDGE_CURVE('',#7121,#7700,#1268,.T.);
#10025=EDGE_CURVE('',#7699,#7119,#1269,.T.);
#10026=EDGE_CURVE('',#7701,#7118,#1270,.T.);
#10027=EDGE_CURVE('',#7122,#7704,#1271,.F.);
#10028=EDGE_CURVE('',#7702,#7196,#1272,.F.);
#10029=EDGE_CURVE('',#7194,#7703,#1273,.F.);
#10030=EDGE_CURVE('',#7262,#7144,#1274,.F.);
#10031=EDGE_CURVE('',#7145,#7260,#1275,.F.);
#10032=EDGE_CURVE('',#7146,#7259,#1276,.T.);
#10033=EDGE_CURVE('',#7264,#7143,#1277,.F.);
#10034=EDGE_CURVE('',#7147,#7258,#1278,.F.);
#10035=EDGE_CURVE('',#7266,#7142,#1279,.F.);
#10036=EDGE_CURVE('',#7148,#7257,#1280,.F.);
#10037=EDGE_CURVE('',#7268,#7141,#1281,.T.);
#10038=EDGE_CURVE('',#7149,#7256,#1282,.F.);
#10039=EDGE_CURVE('',#7269,#7500,#1283,.F.);
#10040=EDGE_CURVE('',#7150,#7253,#1284,.T.);
#10041=EDGE_CURVE('',#7270,#7499,#1285,.F.);
#10042=EDGE_CURVE('',#7151,#7252,#1286,.T.);
#10043=EDGE_CURVE('',#7271,#7498,#1287,.T.);
#10044=EDGE_CURVE('',#7152,#7251,#1288,.T.);
#10045=EDGE_CURVE('',#7272,#7497,#1289,.F.);
#10046=EDGE_CURVE('',#7153,#7248,#1290,.T.);
#10047=EDGE_CURVE('',#7273,#7496,#1291,.F.);
#10048=EDGE_CURVE('',#7154,#7247,#1292,.F.);
#10049=EDGE_CURVE('',#7274,#7495,#1293,.F.);
#10050=EDGE_CURVE('',#7155,#7246,#1294,.T.);
#10051=EDGE_CURVE('',#7275,#7139,#1295,.F.);
#10052=EDGE_CURVE('',#7156,#7245,#1296,.F.);
#10053=EDGE_CURVE('',#7276,#7177,#1297,.F.);
#10054=EDGE_CURVE('',#7157,#7244,#1298,.F.);
#10055=EDGE_CURVE('',#6995,#7168,#1299,.F.);
#10056=EDGE_CURVE('',#7158,#7243,#1300,.F.);
#10057=EDGE_CURVE('',#6997,#7167,#1301,.T.);
#10058=EDGE_CURVE('',#7159,#7241,#1302,.F.);
#10059=EDGE_CURVE('',#6998,#7166,#1303,.F.);
#10060=EDGE_CURVE('',#7160,#7006,#1304,.T.);
#10061=EDGE_CURVE('',#6999,#7165,#1305,.T.);
#10062=EDGE_CURVE('',#7161,#7004,#1306,.T.);
#10063=EDGE_CURVE('',#7000,#7164,#1307,.F.);
#10064=EDGE_CURVE('',#7162,#7003,#1308,.F.);
#10065=EDGE_CURVE('',#7001,#7163,#1309,.F.);
#10066=EDGE_CURVE('',#6986,#7178,#1310,.F.);
#10067=EDGE_CURVE('',#7134,#6992,#1311,.T.);
#10068=EDGE_CURVE('',#7135,#6989,#1312,.T.);
#10069=EDGE_CURVE('',#6988,#7136,#1313,.F.);
#10070=EDGE_CURVE('',#7705,#7706,#1514,.T.);
#10071=EDGE_CURVE('',#7707,#7705,#1314,.T.);
#10072=EDGE_CURVE('',#7707,#7708,#1515,.T.);
#10073=EDGE_CURVE('',#7709,#7708,#1315,.T.);
#10074=EDGE_CURVE('',#7706,#7709,#1316,.T.);
#10075=EDGE_CURVE('',#7710,#7711,#1516,.T.);
#10076=EDGE_CURVE('',#7712,#7710,#1317,.T.);
#10077=EDGE_CURVE('',#7713,#7712,#1318,.T.);
#10078=EDGE_CURVE('',#7714,#7713,#1319,.T.);
#10079=EDGE_CURVE('',#7715,#7714,#1320,.T.);
#10080=EDGE_CURVE('',#7716,#7715,#1321,.T.);
#10081=EDGE_CURVE('',#7717,#7716,#1322,.T.);
#10082=EDGE_CURVE('',#7717,#7718,#1517,.T.);
#10083=EDGE_CURVE('',#7711,#7718,#1323,.T.);
#10084=EDGE_CURVE('',#7719,#7720,#1518,.T.);
#10085=EDGE_CURVE('',#7719,#7721,#1324,.T.);
#10086=EDGE_CURVE('',#7722,#7721,#6121,.T.);
#10087=EDGE_CURVE('',#7722,#7723,#1325,.F.);
#10088=EDGE_CURVE('',#7724,#7723,#1326,.T.);
#10089=EDGE_CURVE('',#7724,#7725,#1327,.F.);
#10090=EDGE_CURVE('',#7726,#7725,#1328,.T.);
#10091=EDGE_CURVE('',#7727,#7726,#6122,.T.);
#10092=EDGE_CURVE('',#7727,#7728,#1519,.T.);
#10093=EDGE_CURVE('',#7729,#7728,#1329,.T.);
#10094=EDGE_CURVE('',#7730,#7729,#1330,.T.);
#10095=EDGE_CURVE('',#7731,#7730,#1331,.T.);
#10096=EDGE_CURVE('',#7732,#7731,#1332,.T.);
#10097=EDGE_CURVE('',#7733,#7732,#1333,.T.);
#10098=EDGE_CURVE('',#7720,#7733,#1334,.T.);
#10099=EDGE_CURVE('',#7734,#7734,#6123,.T.);
#10100=EDGE_CURVE('',#7735,#7736,#6124,.F.);
#10101=EDGE_CURVE('',#7736,#7737,#6125,.T.);
#10102=EDGE_CURVE('',#7737,#7738,#6126,.F.);
#10103=EDGE_CURVE('',#7738,#7739,#6127,.T.);
#10104=EDGE_CURVE('',#7739,#7740,#6128,.F.);
#10105=EDGE_CURVE('',#7740,#7741,#6129,.T.);
#10106=EDGE_CURVE('',#7741,#7742,#6130,.F.);
#10107=EDGE_CURVE('',#7742,#7735,#6131,.T.);
#10108=EDGE_CURVE('',#7743,#7743,#6132,.F.);
#10109=EDGE_CURVE('',#7743,#7734,#2087,.T.);
#10110=EDGE_CURVE('',#7744,#7744,#6133,.T.);
#10111=EDGE_CURVE('',#7745,#7746,#6134,.F.);
#10112=EDGE_CURVE('',#7746,#7747,#6135,.T.);
#10113=EDGE_CURVE('',#7747,#7748,#6136,.F.);
#10114=EDGE_CURVE('',#7748,#7749,#6137,.T.);
#10115=EDGE_CURVE('',#7749,#7750,#6138,.F.);
#10116=EDGE_CURVE('',#7750,#7751,#6139,.T.);
#10117=EDGE_CURVE('',#7751,#7752,#6140,.F.);
#10118=EDGE_CURVE('',#7752,#7745,#6141,.T.);
#10119=EDGE_CURVE('',#7753,#7753,#6142,.T.);
#10120=EDGE_CURVE('',#7751,#7742,#2088,.T.);
#10121=EDGE_CURVE('',#7741,#7752,#2089,.F.);
#10122=EDGE_CURVE('',#7739,#7746,#2090,.F.);
#10123=EDGE_CURVE('',#7745,#7740,#2091,.T.);
#10124=EDGE_CURVE('',#7718,#7711,#1335,.T.);
#10125=EDGE_CURVE('',#7749,#7736,#2092,.T.);
#10126=EDGE_CURVE('',#7735,#7750,#2093,.F.);
#10127=EDGE_CURVE('',#7747,#7738,#2094,.T.);
#10128=EDGE_CURVE('',#7737,#7748,#2095,.F.);
#10129=EDGE_CURVE('',#7753,#7754,#2096,.T.);
#10130=EDGE_CURVE('',#7754,#7755,#6143,.F.);
#10131=EDGE_CURVE('',#7755,#7754,#6144,.F.);
#10132=EDGE_CURVE('',#7756,#7756,#6145,.T.);
#10133=EDGE_CURVE('',#7757,#7757,#6146,.F.);
#10134=EDGE_CURVE('',#7756,#7755,#6147,.T.);
#10135=EDGE_CURVE('',#7758,#7758,#6148,.F.);
#10136=EDGE_CURVE('',#7758,#7759,#2097,.T.);
#10137=EDGE_CURVE('',#7759,#7759,#6149,.T.);
#10138=EDGE_CURVE('',#7760,#7760,#6150,.T.);
#10139=EDGE_CURVE('',#7714,#7709,#2098,.T.);
#10140=EDGE_CURVE('',#7708,#7706,#1336,.T.);
#10141=EDGE_CURVE('',#7710,#7717,#1337,.T.);
#10142=EDGE_CURVE('',#7761,#7762,#6151,.T.);
#10143=EDGE_CURVE('',#7762,#7724,#2099,.T.);
#10144=EDGE_CURVE('',#7763,#7719,#1338,.T.);
#10145=EDGE_CURVE('',#7763,#7727,#6152,.T.);
#10146=EDGE_CURVE('',#7762,#7761,#6153,.T.);
#10147=EDGE_CURVE('',#7764,#7707,#1339,.T.);
#10148=EDGE_CURVE('',#7705,#7764,#1340,.T.);
#10149=EDGE_CURVE('',#7765,#7766,#1341,.T.);
#10150=EDGE_CURVE('',#7766,#7767,#1342,.T.);
#10151=EDGE_CURVE('',#7767,#7768,#1343,.T.);
#10152=EDGE_CURVE('',#7768,#7769,#1344,.T.);
#10153=EDGE_CURVE('',#7769,#7770,#1345,.T.);
#10154=EDGE_CURVE('',#7770,#7765,#1346,.T.);
#10155=EDGE_CURVE('',#7771,#7771,#6154,.T.);
#10156=EDGE_CURVE('',#7731,#7771,#2100,.T.);
#10157=EDGE_CURVE('',#7728,#7720,#1347,.T.);
#10158=EDGE_CURVE('',#7768,#7762,#6155,.T.);
#10159=EDGE_CURVE('',#7760,#7758,#6156,.T.);
#10160=EDGE_CURVE('',#7759,#7757,#6157,.T.);
#10161=EDGE_CURVE('',#7744,#7743,#6158,.T.);
#10162=EDGE_CURVE('',#7772,#7773,#2101,.F.);
#10163=EDGE_CURVE('',#7773,#7774,#2102,.F.);
#10164=EDGE_CURVE('',#7774,#7775,#2103,.F.);
#10165=EDGE_CURVE('',#7775,#7776,#2104,.F.);
#10166=EDGE_CURVE('',#7776,#7777,#2105,.F.);
#10167=EDGE_CURVE('',#7777,#7778,#2106,.F.);
#10168=EDGE_CURVE('',#7778,#7779,#2107,.F.);
#10169=EDGE_CURVE('',#7779,#7780,#2108,.F.);
#10170=EDGE_CURVE('',#7780,#7781,#2109,.F.);
#10171=EDGE_CURVE('',#7782,#7781,#6159,.T.);
#10172=EDGE_CURVE('',#7782,#7783,#6160,.T.);
#10173=EDGE_CURVE('',#7784,#7783,#6161,.T.);
#10174=EDGE_CURVE('',#7784,#7785,#2110,.F.);
#10175=EDGE_CURVE('',#7785,#7786,#2111,.F.);
#10176=EDGE_CURVE('',#7786,#7787,#2112,.F.);
#10177=EDGE_CURVE('',#7787,#7788,#2113,.F.);
#10178=EDGE_CURVE('',#7788,#7772,#2114,.F.);
#10179=EDGE_CURVE('',#7789,#7789,#6162,.F.);
#10180=EDGE_CURVE('',#7790,#7791,#2115,.T.);
#10181=EDGE_CURVE('',#7791,#7792,#2116,.T.);
#10182=EDGE_CURVE('',#7792,#7793,#2117,.T.);
#10183=EDGE_CURVE('',#7793,#7794,#2118,.T.);
#10184=EDGE_CURVE('',#7794,#7795,#2119,.T.);
#10185=EDGE_CURVE('',#7795,#7796,#2120,.T.);
#10186=EDGE_CURVE('',#7796,#7797,#2121,.T.);
#10187=EDGE_CURVE('',#7797,#7798,#2122,.T.);
#10188=EDGE_CURVE('',#7798,#7799,#2123,.T.);
#10189=EDGE_CURVE('',#7799,#7800,#2124,.T.);
#10190=EDGE_CURVE('',#7800,#7801,#2125,.T.);
#10191=EDGE_CURVE('',#7801,#7802,#2126,.T.);
#10192=EDGE_CURVE('',#7802,#7803,#2127,.T.);
#10193=EDGE_CURVE('',#7803,#7804,#2128,.T.);
#10194=EDGE_CURVE('',#7805,#7804,#6163,.T.);
#10195=EDGE_CURVE('',#7805,#7806,#6164,.T.);
#10196=EDGE_CURVE('',#7790,#7806,#6165,.T.);
#10197=EDGE_CURVE('',#7807,#7807,#6166,.F.);
#10198=EDGE_CURVE('',#7808,#7809,#2129,.T.);
#10199=EDGE_CURVE('',#7809,#7810,#2130,.F.);
#10200=EDGE_CURVE('',#7811,#7810,#2131,.T.);
#10201=EDGE_CURVE('',#7811,#7808,#2132,.T.);
#10202=EDGE_CURVE('',#7812,#7813,#2133,.T.);
#10203=EDGE_CURVE('',#7813,#7809,#2134,.F.);
#10204=EDGE_CURVE('',#7808,#7812,#2135,.T.);
#10205=EDGE_CURVE('',#7814,#7815,#2136,.T.);
#10206=EDGE_CURVE('',#7815,#7813,#2137,.F.);
#10207=EDGE_CURVE('',#7812,#7814,#2138,.T.);
#10208=EDGE_CURVE('',#7816,#7817,#2139,.T.);
#10209=EDGE_CURVE('',#7817,#7815,#2140,.F.);
#10210=EDGE_CURVE('',#7814,#7816,#2141,.T.);
#10211=EDGE_CURVE('',#7818,#7819,#2142,.T.);
#10212=EDGE_CURVE('',#7819,#7817,#2143,.F.);
#10213=EDGE_CURVE('',#7816,#7818,#2144,.T.);
#10214=EDGE_CURVE('',#7820,#7821,#2145,.T.);
#10215=EDGE_CURVE('',#7821,#7819,#2146,.F.);
#10216=EDGE_CURVE('',#7818,#7820,#2147,.T.);
#10217=EDGE_CURVE('',#7822,#7823,#2148,.T.);
#10218=EDGE_CURVE('',#7823,#7821,#2149,.F.);
#10219=EDGE_CURVE('',#7820,#7822,#2150,.T.);
#10220=EDGE_CURVE('',#7824,#7825,#2151,.T.);
#10221=EDGE_CURVE('',#7825,#7823,#2152,.F.);
#10222=EDGE_CURVE('',#7822,#7824,#2153,.T.);
#10223=EDGE_CURVE('',#7826,#7827,#2154,.F.);
#10224=EDGE_CURVE('',#7827,#7825,#2155,.F.);
#10225=EDGE_CURVE('',#7824,#7826,#2156,.T.);
#10226=EDGE_CURVE('',#7828,#7829,#2157,.T.);
#10227=EDGE_CURVE('',#7829,#7830,#6167,.F.);
#10228=EDGE_CURVE('',#7830,#7831,#2158,.F.);
#10229=EDGE_CURVE('',#7831,#7828,#6168,.F.);
#10230=EDGE_CURVE('',#7832,#7833,#2159,.T.);
#10231=EDGE_CURVE('',#7833,#7834,#2160,.F.);
#10232=EDGE_CURVE('',#7834,#7835,#2161,.T.);
#10233=EDGE_CURVE('',#7835,#7832,#2162,.T.);
#10234=EDGE_CURVE('',#7836,#7837,#2163,.T.);
#10235=EDGE_CURVE('',#7837,#7833,#2164,.F.);
#10236=EDGE_CURVE('',#7832,#7836,#2165,.T.);
#10237=EDGE_CURVE('',#7838,#7839,#2166,.T.);
#10238=EDGE_CURVE('',#7839,#7837,#2167,.F.);
#10239=EDGE_CURVE('',#7836,#7838,#2168,.T.);
#10240=EDGE_CURVE('',#7840,#7841,#2169,.T.);
#10241=EDGE_CURVE('',#7841,#7839,#2170,.F.);
#10242=EDGE_CURVE('',#7838,#7840,#2171,.T.);
#10243=EDGE_CURVE('',#7810,#7841,#2172,.F.);
#10244=EDGE_CURVE('',#7840,#7811,#2173,.T.);
#10245=EDGE_CURVE('',#7842,#7843,#6169,.T.);
#10246=EDGE_CURVE('',#7843,#7842,#6170,.T.);
#10247=EDGE_CURVE('',#7842,#7844,#2174,.T.);
#10248=EDGE_CURVE('',#7844,#7844,#6171,.T.);
#10249=EDGE_CURVE('',#7774,#7812,#72,.F.);
#10250=EDGE_CURVE('',#7814,#7773,#73,.T.);
#10251=EDGE_CURVE('',#7816,#7772,#74,.T.);
#10252=EDGE_CURVE('',#7799,#7817,#75,.T.);
#10253=EDGE_CURVE('',#7815,#7798,#76,.F.);
#10254=EDGE_CURVE('',#7813,#7797,#77,.F.);
#10255=EDGE_CURVE('',#7775,#7808,#78,.F.);
#10256=EDGE_CURVE('',#7818,#7788,#79,.T.);
#10257=EDGE_CURVE('',#7800,#7819,#80,.T.);
#10258=EDGE_CURVE('',#7809,#7796,#81,.F.);
#10259=EDGE_CURVE('',#7776,#7811,#82,.F.);
#10260=EDGE_CURVE('',#7820,#7787,#83,.T.);
#10261=EDGE_CURVE('',#7801,#7821,#84,.T.);
#10262=EDGE_CURVE('',#7810,#7795,#85,.F.);
#10263=EDGE_CURVE('',#7777,#7840,#86,.F.);
#10264=EDGE_CURVE('',#7822,#7786,#87,.T.);
#10265=EDGE_CURVE('',#7802,#7823,#88,.T.);
#10266=EDGE_CURVE('',#7841,#7794,#89,.F.);
#10267=EDGE_CURVE('',#7778,#7838,#90,.F.);
#10268=EDGE_CURVE('',#7824,#7785,#91,.T.);
#10269=EDGE_CURVE('',#7803,#7825,#92,.T.);
#10270=EDGE_CURVE('',#7839,#7793,#93,.F.);
#10271=EDGE_CURVE('',#7779,#7836,#94,.F.);
#10272=EDGE_CURVE('',#7826,#7784,#6172,.T.);
#10273=EDGE_CURVE('',#7827,#7830,#6173,.F.);
#10274=EDGE_CURVE('',#7831,#7826,#6174,.F.);
#10275=EDGE_CURVE('',#7804,#7827,#6175,.T.);
#10276=EDGE_CURVE('',#7837,#7792,#95,.F.);
#10277=EDGE_CURVE('',#7780,#7832,#96,.F.);
#10278=EDGE_CURVE('',#7831,#7783,#6176,.F.);
#10279=EDGE_CURVE('',#7805,#7830,#6177,.F.);
#10280=EDGE_CURVE('',#7833,#7791,#97,.F.);
#10281=EDGE_CURVE('',#7781,#7835,#6178,.T.);
#10282=EDGE_CURVE('',#7828,#7782,#6179,.T.);
#10283=EDGE_CURVE('',#7806,#7829,#6180,.T.);
#10284=EDGE_CURVE('',#7834,#7790,#6181,.T.);
#10285=EDGE_CURVE('',#7828,#7835,#6182,.T.);
#10286=EDGE_CURVE('',#7834,#7829,#6183,.T.);
#10287=EDGE_CURVE('',#7844,#7807,#6184,.T.);
#10288=EDGE_CURVE('',#7843,#7789,#6185,.T.);
#10289=EDGE_CURVE('',#7845,#7846,#2175,.F.);
#10290=EDGE_CURVE('',#7846,#7847,#6186,.F.);
#10291=EDGE_CURVE('',#7847,#7848,#2176,.T.);
#10292=EDGE_CURVE('',#7848,#7845,#6187,.F.);
#10293=EDGE_CURVE('',#7849,#7850,#2177,.F.);
#10294=EDGE_CURVE('',#7850,#7851,#2178,.F.);
#10295=EDGE_CURVE('',#7851,#7852,#2179,.F.);
#10296=EDGE_CURVE('',#7852,#7849,#2180,.T.);
#10297=EDGE_CURVE('',#7853,#7854,#2181,.T.);
#10298=EDGE_CURVE('',#7853,#7855,#2182,.F.);
#10299=EDGE_CURVE('',#7855,#7856,#2183,.T.);
#10300=EDGE_CURVE('',#7856,#7854,#2184,.T.);
#10301=EDGE_CURVE('',#7857,#7858,#2185,.T.);
#10302=EDGE_CURVE('',#7857,#7853,#2186,.F.);
#10303=EDGE_CURVE('',#7854,#7858,#2187,.T.);
#10304=EDGE_CURVE('',#7859,#7860,#2188,.T.);
#10305=EDGE_CURVE('',#7859,#7857,#2189,.F.);
#10306=EDGE_CURVE('',#7858,#7860,#2190,.T.);
#10307=EDGE_CURVE('',#7861,#7862,#2191,.T.);
#10308=EDGE_CURVE('',#7861,#7859,#2192,.F.);
#10309=EDGE_CURVE('',#7860,#7862,#2193,.T.);
#10310=EDGE_CURVE('',#7863,#7864,#2194,.T.);
#10311=EDGE_CURVE('',#7863,#7861,#2195,.F.);
#10312=EDGE_CURVE('',#7862,#7864,#2196,.T.);
#10313=EDGE_CURVE('',#7865,#7866,#2197,.T.);
#10314=EDGE_CURVE('',#7865,#7863,#2198,.F.);
#10315=EDGE_CURVE('',#7864,#7866,#2199,.T.);
#10316=EDGE_CURVE('',#7867,#7868,#2200,.T.);
#10317=EDGE_CURVE('',#7867,#7865,#2201,.F.);
#10318=EDGE_CURVE('',#7866,#7868,#2202,.T.);
#10319=EDGE_CURVE('',#7869,#7870,#2203,.T.);
#10320=EDGE_CURVE('',#7869,#7867,#2204,.F.);
#10321=EDGE_CURVE('',#7868,#7870,#2205,.T.);
#10322=EDGE_CURVE('',#7871,#7872,#2206,.T.);
#10323=EDGE_CURVE('',#7871,#7869,#2207,.F.);
#10324=EDGE_CURVE('',#7870,#7872,#2208,.T.);
#10325=EDGE_CURVE('',#7873,#7874,#2209,.T.);
#10326=EDGE_CURVE('',#7873,#7871,#2210,.F.);
#10327=EDGE_CURVE('',#7872,#7874,#2211,.T.);
#10328=EDGE_CURVE('',#7875,#7876,#2212,.T.);
#10329=EDGE_CURVE('',#7875,#7873,#2213,.F.);
#10330=EDGE_CURVE('',#7874,#7876,#2214,.T.);
#10331=EDGE_CURVE('',#7877,#7878,#2215,.F.);
#10332=EDGE_CURVE('',#7878,#7875,#2216,.F.);
#10333=EDGE_CURVE('',#7876,#7877,#2217,.T.);
#10334=EDGE_CURVE('',#7879,#7880,#2218,.T.);
#10335=EDGE_CURVE('',#7880,#7881,#2219,.F.);
#10336=EDGE_CURVE('',#7881,#7882,#2220,.T.);
#10337=EDGE_CURVE('',#7882,#7879,#2221,.T.);
#10338=EDGE_CURVE('',#7883,#7884,#2222,.F.);
#10339=EDGE_CURVE('',#7884,#7885,#2223,.F.);
#10340=EDGE_CURVE('',#7885,#7886,#2224,.F.);
#10341=EDGE_CURVE('',#7887,#7886,#6188,.T.);
#10342=EDGE_CURVE('',#7887,#7888,#6189,.T.);
#10343=EDGE_CURVE('',#7889,#7888,#6190,.T.);
#10344=EDGE_CURVE('',#7889,#7890,#2225,.F.);
#10345=EDGE_CURVE('',#7891,#7890,#6191,.T.);
#10346=EDGE_CURVE('',#7891,#7892,#2226,.F.);
#10347=EDGE_CURVE('',#7892,#7893,#2227,.F.);
#10348=EDGE_CURVE('',#7893,#7894,#2228,.F.);
#10349=EDGE_CURVE('',#7894,#7895,#2229,.F.);
#10350=EDGE_CURVE('',#7895,#7896,#2230,.F.);
#10351=EDGE_CURVE('',#7896,#7897,#2231,.F.);
#10352=EDGE_CURVE('',#7897,#7898,#2232,.F.);
#10353=EDGE_CURVE('',#7898,#7899,#2233,.F.);
#10354=EDGE_CURVE('',#7899,#7900,#2234,.F.);
#10355=EDGE_CURVE('',#7900,#7883,#2235,.F.);
#10356=EDGE_CURVE('',#7901,#7901,#6192,.F.);
#10357=EDGE_CURVE('',#7902,#7903,#2236,.T.);
#10358=EDGE_CURVE('',#7903,#7904,#2237,.T.);
#10359=EDGE_CURVE('',#7904,#7905,#2238,.T.);
#10360=EDGE_CURVE('',#7906,#7905,#6193,.T.);
#10361=EDGE_CURVE('',#7906,#7907,#2239,.T.);
#10362=EDGE_CURVE('',#7908,#7907,#6194,.T.);
#10363=EDGE_CURVE('',#7908,#7909,#6195,.T.);
#10364=EDGE_CURVE('',#7910,#7909,#6196,.T.);
#10365=EDGE_CURVE('',#7910,#7911,#2240,.T.);
#10366=EDGE_CURVE('',#7911,#7912,#2241,.T.);
#10367=EDGE_CURVE('',#7912,#7913,#2242,.T.);
#10368=EDGE_CURVE('',#7913,#7914,#2243,.T.);
#10369=EDGE_CURVE('',#7914,#7915,#2244,.T.);
#10370=EDGE_CURVE('',#7915,#7916,#2245,.T.);
#10371=EDGE_CURVE('',#7916,#7917,#2246,.T.);
#10372=EDGE_CURVE('',#7917,#7918,#2247,.T.);
#10373=EDGE_CURVE('',#7918,#7919,#2248,.T.);
#10374=EDGE_CURVE('',#7919,#7902,#2249,.T.);
#10375=EDGE_CURVE('',#7920,#7920,#6197,.F.);
#10376=EDGE_CURVE('',#7921,#7922,#6198,.T.);
#10377=EDGE_CURVE('',#7922,#7921,#6199,.T.);
#10378=EDGE_CURVE('',#7921,#7923,#2250,.T.);
#10379=EDGE_CURVE('',#7923,#7923,#6200,.T.);
#10380=EDGE_CURVE('',#7917,#7865,#98,.F.);
#10381=EDGE_CURVE('',#7863,#7916,#99,.T.);
#10382=EDGE_CURVE('',#7861,#7915,#100,.T.);
#10383=EDGE_CURVE('',#7899,#7862,#101,.T.);
#10384=EDGE_CURVE('',#7864,#7898,#102,.F.);
#10385=EDGE_CURVE('',#7866,#7897,#103,.F.);
#10386=EDGE_CURVE('',#7918,#7867,#104,.F.);
#10387=EDGE_CURVE('',#7859,#7914,#105,.T.);
#10388=EDGE_CURVE('',#7900,#7860,#106,.T.);
#10389=EDGE_CURVE('',#7868,#7896,#107,.F.);
#10390=EDGE_CURVE('',#7919,#7869,#108,.F.);
#10391=EDGE_CURVE('',#7857,#7913,#109,.T.);
#10392=EDGE_CURVE('',#7883,#7858,#110,.T.);
#10393=EDGE_CURVE('',#7870,#7895,#111,.F.);
#10394=EDGE_CURVE('',#7902,#7871,#112,.F.);
#10395=EDGE_CURVE('',#7853,#7912,#113,.T.);
#10396=EDGE_CURVE('',#7884,#7854,#114,.T.);
#10397=EDGE_CURVE('',#7872,#7894,#115,.F.);
#10398=EDGE_CURVE('',#7903,#7873,#116,.F.);
#10399=EDGE_CURVE('',#7855,#7911,#6201,.T.);
#10400=EDGE_CURVE('',#7856,#7849,#6202,.T.);
#10401=EDGE_CURVE('',#7850,#7855,#6203,.T.);
#10402=EDGE_CURVE('',#7885,#7856,#6204,.T.);
#10403=EDGE_CURVE('',#7874,#7893,#117,.F.);
#10404=EDGE_CURVE('',#7904,#7875,#118,.F.);
#10405=EDGE_CURVE('',#7850,#7911,#6205,.F.);
#10406=EDGE_CURVE('',#7885,#7849,#6206,.F.);
#10407=EDGE_CURVE('',#7876,#7892,#119,.F.);
#10408=EDGE_CURVE('',#7905,#7878,#6207,.T.);
#10409=EDGE_CURVE('',#7851,#7910,#6208,.T.);
#10410=EDGE_CURVE('',#7852,#7845,#6209,.F.);
#10411=EDGE_CURVE('',#7846,#7851,#6210,.F.);
#10412=EDGE_CURVE('',#7886,#7852,#6211,.T.);
#10413=EDGE_CURVE('',#7877,#7891,#6212,.T.);
#10414=EDGE_CURVE('',#7878,#7881,#6213,.F.);
#10415=EDGE_CURVE('',#7882,#7877,#6214,.F.);
#10416=EDGE_CURVE('',#7906,#7881,#6215,.F.);
#10417=EDGE_CURVE('',#7846,#7909,#6216,.F.);
#10418=EDGE_CURVE('',#7887,#7845,#6217,.F.);
#10419=EDGE_CURVE('',#7882,#7890,#6218,.F.);
#10420=EDGE_CURVE('',#7907,#7880,#6219,.T.);
#10421=EDGE_CURVE('',#7847,#7908,#6220,.T.);
#10422=EDGE_CURVE('',#7888,#7848,#6221,.T.);
#10423=EDGE_CURVE('',#7879,#7889,#6222,.T.);
#10424=EDGE_CURVE('',#7847,#7880,#6223,.T.);
#10425=EDGE_CURVE('',#7879,#7848,#6224,.T.);
#10426=EDGE_CURVE('',#7923,#7920,#6225,.T.);
#10427=EDGE_CURVE('',#7922,#7901,#6226,.T.);
#10428=EDGE_CURVE('',#7924,#7924,#6227,.F.);
#10429=EDGE_CURVE('',#7924,#7925,#2251,.T.);
#10430=EDGE_CURVE('',#7925,#7925,#6228,.F.);
#10431=EDGE_CURVE('',#7926,#7927,#6229,.T.);
#10432=EDGE_CURVE('',#7928,#7926,#2252,.T.);
#10433=EDGE_CURVE('',#7928,#7929,#6230,.T.);
#10434=EDGE_CURVE('',#7929,#7927,#2253,.T.);
#10435=EDGE_CURVE('',#7930,#7926,#2254,.T.);
#10436=EDGE_CURVE('',#7931,#7930,#2255,.T.);
#10437=EDGE_CURVE('',#7931,#7928,#2256,.T.);
#10438=EDGE_CURVE('',#7932,#7930,#6231,.T.);
#10439=EDGE_CURVE('',#7933,#7932,#2257,.T.);
#10440=EDGE_CURVE('',#7933,#7931,#6232,.T.);
#10441=EDGE_CURVE('',#7927,#7932,#2258,.T.);
#10442=EDGE_CURVE('',#7929,#7933,#2259,.T.);
#10443=EDGE_CURVE('',#7934,#7934,#6233,.F.);
#10444=EDGE_CURVE('',#7935,#7935,#6234,.T.);
#10445=EDGE_CURVE('',#7936,#7937,#6235,.T.);
#10446=EDGE_CURVE('',#7937,#7936,#6236,.T.);
#10447=EDGE_CURVE('',#7936,#7938,#2260,.T.);
#10448=EDGE_CURVE('',#7938,#7938,#6237,.T.);
#10449=EDGE_CURVE('',#7939,#7939,#6238,.F.);
#10450=EDGE_CURVE('',#7940,#7940,#6239,.T.);
#10451=EDGE_CURVE('',#7940,#7935,#2261,.T.);
#10452=EDGE_CURVE('',#7938,#7939,#6240,.T.);
#10453=EDGE_CURVE('',#7937,#7934,#6241,.T.);
#10454=EDGE_CURVE('',#7941,#7942,#6242,.F.);
#10455=EDGE_CURVE('',#7943,#7941,#6243,.F.);
#10456=EDGE_CURVE('',#7944,#7943,#6244,.F.);
#10457=EDGE_CURVE('',#7945,#7944,#6245,.F.);
#10458=EDGE_CURVE('',#7946,#7945,#6246,.F.);
#10459=EDGE_CURVE('',#7947,#7946,#6247,.F.);
#10460=EDGE_CURVE('',#7948,#7947,#6248,.F.);
#10461=EDGE_CURVE('',#7949,#7948,#6249,.F.);
#10462=EDGE_CURVE('',#7950,#7949,#6250,.F.);
#10463=EDGE_CURVE('',#7951,#7950,#6251,.F.);
#10464=EDGE_CURVE('',#7952,#7951,#6252,.F.);
#10465=EDGE_CURVE('',#7953,#7952,#6253,.F.);
#10466=EDGE_CURVE('',#7953,#7954,#6254,.T.);
#10467=EDGE_CURVE('',#7954,#7955,#6255,.T.);
#10468=EDGE_CURVE('',#7955,#7954,#6256,.T.);
#10469=EDGE_CURVE('',#7956,#7953,#6257,.F.);
#10470=EDGE_CURVE('',#7957,#7956,#6258,.F.);
#10471=EDGE_CURVE('',#7958,#7957,#6259,.F.);
#10472=EDGE_CURVE('',#7959,#7958,#6260,.F.);
#10473=EDGE_CURVE('',#7960,#7959,#6261,.F.);
#10474=EDGE_CURVE('',#7961,#7960,#6262,.F.);
#10475=EDGE_CURVE('',#7962,#7961,#6263,.F.);
#10476=EDGE_CURVE('',#7963,#7962,#6264,.F.);
#10477=EDGE_CURVE('',#7942,#7963,#6265,.F.);
#10478=EDGE_CURVE('',#7964,#7964,#6266,.T.);
#10479=EDGE_CURVE('',#7965,#7965,#6267,.T.);
#10480=EDGE_CURVE('',#7955,#7964,#2262,.T.);
#10481=EDGE_CURVE('',#7966,#7966,#6268,.F.);
#10482=EDGE_CURVE('',#7967,#7967,#6269,.F.);
#10483=EDGE_CURVE('',#7967,#7968,#2263,.T.);
#10484=EDGE_CURVE('',#7968,#7968,#6270,.T.);
#10485=EDGE_CURVE('',#7968,#7966,#2264,.T.);
#10486=EDGE_CURVE('',#7969,#7942,#2265,.T.);
#10487=EDGE_CURVE('',#7969,#7970,#2266,.F.);
#10488=EDGE_CURVE('',#7970,#7941,#2267,.T.);
#10489=EDGE_CURVE('',#7970,#7971,#2268,.F.);
#10490=EDGE_CURVE('',#7971,#7943,#2269,.T.);
#10491=EDGE_CURVE('',#7971,#7972,#2270,.F.);
#10492=EDGE_CURVE('',#7972,#7944,#2271,.T.);
#10493=EDGE_CURVE('',#7972,#7973,#2272,.F.);
#10494=EDGE_CURVE('',#7973,#7945,#2273,.T.);
#10495=EDGE_CURVE('',#7973,#7974,#2274,.F.);
#10496=EDGE_CURVE('',#7974,#7946,#2275,.T.);
#10497=EDGE_CURVE('',#7974,#7975,#2276,.F.);
#10498=EDGE_CURVE('',#7975,#7947,#2277,.T.);
#10499=EDGE_CURVE('',#7975,#7976,#2278,.F.);
#10500=EDGE_CURVE('',#7976,#7948,#2279,.T.);
#10501=EDGE_CURVE('',#7976,#7977,#2280,.F.);
#10502=EDGE_CURVE('',#7977,#7949,#2281,.T.);
#10503=EDGE_CURVE('',#7977,#7978,#2282,.F.);
#10504=EDGE_CURVE('',#7978,#7950,#2283,.T.);
#10505=EDGE_CURVE('',#7978,#7979,#2284,.F.);
#10506=EDGE_CURVE('',#7979,#7951,#2285,.T.);
#10507=EDGE_CURVE('',#7979,#7980,#2286,.F.);
#10508=EDGE_CURVE('',#7980,#7952,#2287,.T.);
#10509=EDGE_CURVE('',#7980,#7981,#2288,.F.);
#10510=EDGE_CURVE('',#7981,#7956,#2289,.T.);
#10511=EDGE_CURVE('',#7981,#7982,#2290,.F.);
#10512=EDGE_CURVE('',#7982,#7957,#2291,.T.);
#10513=EDGE_CURVE('',#7982,#7983,#2292,.F.);
#10514=EDGE_CURVE('',#7983,#7958,#2293,.T.);
#10515=EDGE_CURVE('',#7983,#7984,#2294,.F.);
#10516=EDGE_CURVE('',#7984,#7959,#2295,.T.);
#10517=EDGE_CURVE('',#7984,#7985,#2296,.F.);
#10518=EDGE_CURVE('',#7985,#7960,#2297,.T.);
#10519=EDGE_CURVE('',#7985,#7986,#2298,.F.);
#10520=EDGE_CURVE('',#7986,#7961,#2299,.T.);
#10521=EDGE_CURVE('',#7986,#7987,#2300,.F.);
#10522=EDGE_CURVE('',#7987,#7962,#2301,.T.);
#10523=EDGE_CURVE('',#7987,#7988,#2302,.F.);
#10524=EDGE_CURVE('',#7988,#7963,#2303,.T.);
#10525=EDGE_CURVE('',#7988,#7969,#2304,.F.);
#10526=EDGE_CURVE('',#7965,#7967,#6271,.T.);
#10527=EDGE_CURVE('',#7989,#7990,#2305,.T.);
#10528=EDGE_CURVE('',#7990,#7991,#6272,.T.);
#10529=EDGE_CURVE('',#7992,#7991,#2306,.T.);
#10530=EDGE_CURVE('',#7992,#7989,#6273,.F.);
#10531=EDGE_CURVE('',#7991,#7990,#6274,.T.);
#10532=EDGE_CURVE('',#7989,#7992,#6275,.F.);
#10533=EDGE_CURVE('',#7993,#7994,#6276,.T.);
#10534=EDGE_CURVE('',#7994,#7993,#6277,.T.);
#10535=EDGE_CURVE('',#7995,#7995,#6278,.F.);
#10536=EDGE_CURVE('',#7996,#7996,#6279,.F.);
#10537=EDGE_CURVE('',#7997,#7997,#6280,.F.);
#10538=EDGE_CURVE('',#7998,#7998,#6281,.F.);
#10539=EDGE_CURVE('',#7999,#8000,#6282,.F.);
#10540=EDGE_CURVE('',#8000,#7999,#6283,.F.);
#10541=EDGE_CURVE('',#8001,#8001,#6284,.T.);
#10542=EDGE_CURVE('',#8002,#8002,#6285,.T.);
#10543=EDGE_CURVE('',#8003,#8003,#6286,.T.);
#10544=EDGE_CURVE('',#8004,#8004,#6287,.T.);
#10545=EDGE_CURVE('',#8005,#8006,#6288,.T.);
#10546=EDGE_CURVE('',#8006,#8005,#6289,.T.);
#10547=EDGE_CURVE('',#8005,#8007,#2307,.T.);
#10548=EDGE_CURVE('',#8007,#8008,#6290,.F.);
#10549=EDGE_CURVE('',#8008,#8007,#6291,.F.);
#10550=EDGE_CURVE('',#8009,#8010,#6292,.T.);
#10551=EDGE_CURVE('',#8010,#8009,#6293,.T.);
#10552=EDGE_CURVE('',#8009,#8011,#2308,.T.);
#10553=EDGE_CURVE('',#8011,#8012,#6294,.F.);
#10554=EDGE_CURVE('',#8012,#8011,#6295,.F.);
#10555=EDGE_CURVE('',#8013,#8014,#6296,.T.);
#10556=EDGE_CURVE('',#8014,#8013,#6297,.T.);
#10557=EDGE_CURVE('',#8013,#8015,#2309,.T.);
#10558=EDGE_CURVE('',#8015,#8016,#6298,.F.);
#10559=EDGE_CURVE('',#8016,#8015,#6299,.F.);
#10560=EDGE_CURVE('',#8017,#8018,#6300,.T.);
#10561=EDGE_CURVE('',#8018,#8017,#6301,.T.);
#10562=EDGE_CURVE('',#8017,#8019,#2310,.T.);
#10563=EDGE_CURVE('',#8019,#8020,#6302,.F.);
#10564=EDGE_CURVE('',#8020,#8019,#6303,.F.);
#10565=EDGE_CURVE('',#8000,#7990,#1348,.F.);
#10566=EDGE_CURVE('',#7991,#7999,#1349,.T.);
#10567=EDGE_CURVE('',#8001,#8008,#6304,.T.);
#10568=EDGE_CURVE('',#8002,#8012,#6305,.T.);
#10569=EDGE_CURVE('',#8003,#8016,#6306,.T.);
#10570=EDGE_CURVE('',#8004,#8020,#6307,.T.);
#10571=EDGE_CURVE('',#7989,#7993,#1350,.T.);
#10572=EDGE_CURVE('',#7994,#7992,#1351,.F.);
#10573=EDGE_CURVE('',#8006,#7995,#6308,.T.);
#10574=EDGE_CURVE('',#8010,#7996,#6309,.T.);
#10575=EDGE_CURVE('',#8014,#7997,#6310,.T.);
#10576=EDGE_CURVE('',#8018,#7998,#6311,.T.);
#10577=EDGE_CURVE('',#8021,#8022,#2311,.T.);
#10578=EDGE_CURVE('',#8022,#8023,#6312,.T.);
#10579=EDGE_CURVE('',#8023,#8024,#2312,.T.);
#10580=EDGE_CURVE('',#8024,#8021,#6313,.T.);
#10581=EDGE_CURVE('',#8025,#8026,#2313,.T.);
#10582=EDGE_CURVE('',#8026,#8027,#2314,.F.);
#10583=EDGE_CURVE('',#8027,#8028,#2315,.F.);
#10584=EDGE_CURVE('',#8028,#8025,#2316,.T.);
#10585=EDGE_CURVE('',#8029,#8030,#2317,.T.);
#10586=EDGE_CURVE('',#8030,#8031,#2318,.T.);
#10587=EDGE_CURVE('',#8032,#8031,#2319,.T.);
#10588=EDGE_CURVE('',#8032,#8029,#2320,.F.);
#10589=EDGE_CURVE('',#8031,#8033,#6314,.F.);
#10590=EDGE_CURVE('',#8034,#8033,#2321,.T.);
#10591=EDGE_CURVE('',#8034,#8032,#6315,.T.);
#10592=EDGE_CURVE('',#8033,#8035,#2322,.T.);
#10593=EDGE_CURVE('',#8035,#8036,#2323,.F.);
#10594=EDGE_CURVE('',#8036,#8034,#2324,.F.);
#10595=EDGE_CURVE('',#8037,#8038,#2325,.F.);
#10596=EDGE_CURVE('',#8038,#8039,#2326,.T.);
#10597=EDGE_CURVE('',#8039,#8040,#2327,.T.);
#10598=EDGE_CURVE('',#8040,#8037,#2328,.F.);
#10599=EDGE_CURVE('',#8041,#8042,#2329,.T.);
#10600=EDGE_CURVE('',#8042,#8043,#6316,.T.);
#10601=EDGE_CURVE('',#8044,#8043,#2330,.F.);
#10602=EDGE_CURVE('',#8044,#8041,#6317,.T.);
#10603=EDGE_CURVE('',#8043,#8022,#6318,.F.);
#10604=EDGE_CURVE('',#8021,#8044,#6319,.T.);
#10605=EDGE_CURVE('',#8045,#8046,#1352,.T.);
#10606=EDGE_CURVE('',#8046,#8047,#1353,.T.);
#10607=EDGE_CURVE('',#8047,#8048,#6320,.F.);
#10608=EDGE_CURVE('',#8048,#8049,#120,.T.);
#10609=EDGE_CURVE('',#8049,#8050,#121,.T.);
#10610=EDGE_CURVE('',#8050,#8051,#2331,.T.);
#10611=EDGE_CURVE('',#8051,#8052,#2332,.T.);
#10612=EDGE_CURVE('',#8052,#8053,#6321,.F.);
#10613=EDGE_CURVE('',#8053,#8054,#2333,.T.);
#10614=EDGE_CURVE('',#8054,#8045,#2334,.T.);
#10615=EDGE_CURVE('',#8055,#8055,#6322,.T.);
#10616=EDGE_CURVE('',#8056,#8057,#2335,.F.);
#10617=EDGE_CURVE('',#8057,#8058,#2336,.F.);
#10618=EDGE_CURVE('',#8058,#8059,#1354,.T.);
#10619=EDGE_CURVE('',#8059,#8060,#1355,.T.);
#10620=EDGE_CURVE('',#8060,#8061,#6323,.T.);
#10621=EDGE_CURVE('',#8061,#8062,#122,.T.);
#10622=EDGE_CURVE('',#8062,#8063,#123,.T.);
#10623=EDGE_CURVE('',#8063,#8064,#2337,.F.);
#10624=EDGE_CURVE('',#8064,#8065,#2338,.F.);
#10625=EDGE_CURVE('',#8065,#8056,#6324,.T.);
#10626=EDGE_CURVE('',#8066,#8066,#6325,.F.);
#10627=EDGE_CURVE('',#8067,#8068,#6326,.T.);
#10628=EDGE_CURVE('',#8068,#8067,#6327,.T.);
#10629=EDGE_CURVE('',#8067,#8069,#2339,.T.);
#10630=EDGE_CURVE('',#8069,#8070,#6328,.F.);
#10631=EDGE_CURVE('',#8070,#8069,#6329,.F.);
#10632=EDGE_CURVE('',#8045,#8037,#6330,.T.);
#10633=EDGE_CURVE('',#8038,#8054,#6331,.T.);
#10634=EDGE_CURVE('',#8045,#8041,#1356,.F.);
#10635=EDGE_CURVE('',#8041,#8037,#6332,.F.);
#10636=EDGE_CURVE('',#8038,#8036,#6333,.F.);
#10637=EDGE_CURVE('',#8036,#8054,#6334,.F.);
#10638=EDGE_CURVE('',#8042,#8040,#6335,.T.);
#10639=EDGE_CURVE('',#8047,#8044,#1357,.F.);
#10640=EDGE_CURVE('',#8034,#8053,#6336,.T.);
#10641=EDGE_CURVE('',#8039,#8035,#6337,.T.);
#10642=EDGE_CURVE('',#8040,#8063,#6338,.T.);
#10643=EDGE_CURVE('',#8064,#8039,#6339,.T.);
#10644=EDGE_CURVE('',#8042,#8063,#1358,.F.);
#10645=EDGE_CURVE('',#8048,#8021,#6340,.F.);
#10646=EDGE_CURVE('',#8032,#8052,#6341,.T.);
#10647=EDGE_CURVE('',#8064,#8035,#6342,.F.);
#10648=EDGE_CURVE('',#8043,#8061,#1359,.F.);
#10649=EDGE_CURVE('',#8050,#8024,#1360,.T.);
#10650=EDGE_CURVE('',#8051,#8027,#6343,.T.);
#10651=EDGE_CURVE('',#8071,#8050,#6344,.T.);
#10652=EDGE_CURVE('',#8028,#8071,#6345,.T.);
#10653=EDGE_CURVE('',#8029,#8051,#6346,.T.);
#10654=EDGE_CURVE('',#8065,#8033,#6347,.T.);
#10655=EDGE_CURVE('',#8022,#8060,#6348,.F.);
#10656=EDGE_CURVE('',#8072,#8071,#6349,.T.);
#10657=EDGE_CURVE('',#8028,#8024,#6350,.F.);
#10658=EDGE_CURVE('',#8029,#8027,#6351,.F.);
#10659=EDGE_CURVE('',#8056,#8031,#6352,.T.);
#10660=EDGE_CURVE('',#8023,#8058,#1361,.T.);
#10661=EDGE_CURVE('',#8025,#8023,#6353,.T.);
#10662=EDGE_CURVE('',#8030,#8026,#6354,.T.);
#10663=EDGE_CURVE('',#8057,#8030,#6355,.T.);
#10664=EDGE_CURVE('',#8025,#8058,#6356,.F.);
#10665=EDGE_CURVE('',#8057,#8026,#6357,.F.);
#10666=EDGE_CURVE('',#8068,#8066,#6358,.T.);
#10667=EDGE_CURVE('',#8055,#8070,#6359,.T.);
#10668=EDGE_CURVE('',#8073,#8074,#1520,.T.);
#10669=EDGE_CURVE('',#8075,#8073,#1362,.T.);
#10670=EDGE_CURVE('',#8075,#8076,#1521,.T.);
#10671=EDGE_CURVE('',#8077,#8076,#1363,.T.);
#10672=EDGE_CURVE('',#8078,#8077,#1364,.T.);
#10673=EDGE_CURVE('',#8079,#8078,#1365,.T.);
#10674=EDGE_CURVE('',#8080,#8079,#1366,.T.);
#10675=EDGE_CURVE('',#8081,#8080,#1367,.T.);
#10676=EDGE_CURVE('',#8082,#8081,#1368,.T.);
#10677=EDGE_CURVE('',#8074,#8082,#1369,.T.);
#10678=EDGE_CURVE('',#8083,#8084,#1522,.T.);
#10679=EDGE_CURVE('',#8085,#8083,#1370,.T.);
#10680=EDGE_CURVE('',#8085,#8086,#1523,.T.);
#10681=EDGE_CURVE('',#8087,#8086,#1371,.T.);
#10682=EDGE_CURVE('',#8088,#8087,#1372,.T.);
#10683=EDGE_CURVE('',#8089,#8088,#1373,.T.);
#10684=EDGE_CURVE('',#8090,#8089,#1374,.T.);
#10685=EDGE_CURVE('',#8091,#8090,#1375,.T.);
#10686=EDGE_CURVE('',#8092,#8091,#1376,.T.);
#10687=EDGE_CURVE('',#8084,#8092,#1377,.T.);
#10688=EDGE_CURVE('',#8093,#8094,#1524,.T.);
#10689=EDGE_CURVE('',#8095,#8093,#1378,.T.);
#10690=EDGE_CURVE('',#8095,#8096,#1525,.T.);
#10691=EDGE_CURVE('',#8097,#8096,#1379,.T.);
#10692=EDGE_CURVE('',#8098,#8097,#1380,.T.);
#10693=EDGE_CURVE('',#8099,#8098,#1381,.T.);
#10694=EDGE_CURVE('',#8100,#8099,#1382,.T.);
#10695=EDGE_CURVE('',#8101,#8100,#1383,.T.);
#10696=EDGE_CURVE('',#8102,#8101,#1384,.T.);
#10697=EDGE_CURVE('',#8094,#8102,#1385,.T.);
#10698=EDGE_CURVE('',#8103,#8104,#1526,.T.);
#10699=EDGE_CURVE('',#8105,#8103,#1386,.T.);
#10700=EDGE_CURVE('',#8105,#8106,#1527,.T.);
#10701=EDGE_CURVE('',#8107,#8106,#1387,.T.);
#10702=EDGE_CURVE('',#8108,#8107,#1388,.T.);
#10703=EDGE_CURVE('',#8109,#8108,#1389,.T.);
#10704=EDGE_CURVE('',#8110,#8109,#1390,.T.);
#10705=EDGE_CURVE('',#8111,#8110,#1391,.T.);
#10706=EDGE_CURVE('',#8112,#8111,#1392,.T.);
#10707=EDGE_CURVE('',#8104,#8112,#1393,.T.);
#10708=EDGE_CURVE('',#8113,#8114,#1528,.T.);
#10709=EDGE_CURVE('',#8115,#8113,#1394,.T.);
#10710=EDGE_CURVE('',#8115,#8116,#1529,.T.);
#10711=EDGE_CURVE('',#8117,#8116,#1395,.T.);
#10712=EDGE_CURVE('',#8118,#8117,#1396,.T.);
#10713=EDGE_CURVE('',#8119,#8118,#1397,.T.);
#10714=EDGE_CURVE('',#8120,#8119,#1398,.T.);
#10715=EDGE_CURVE('',#8121,#8120,#1399,.T.);
#10716=EDGE_CURVE('',#8122,#8121,#1400,.T.);
#10717=EDGE_CURVE('',#8114,#8122,#1401,.T.);
#10718=EDGE_CURVE('',#8123,#8124,#1402,.T.);
#10719=EDGE_CURVE('',#8123,#8125,#2340,.T.);
#10720=EDGE_CURVE('',#8125,#8126,#6360,.F.);
#10721=EDGE_CURVE('',#8126,#8127,#2341,.F.);
#10722=EDGE_CURVE('',#8127,#8128,#6361,.T.);
#10723=EDGE_CURVE('',#8128,#8124,#6362,.T.);
#10724=EDGE_CURVE('',#8129,#8129,#6363,.F.);
#10725=EDGE_CURVE('',#8129,#8130,#2342,.T.);
#10726=EDGE_CURVE('',#8130,#8130,#6364,.T.);
#10727=EDGE_CURVE('',#8131,#8132,#6365,.T.);
#10728=EDGE_CURVE('',#8132,#8133,#2343,.F.);
#10729=EDGE_CURVE('',#8133,#8134,#6366,.F.);
#10730=EDGE_CURVE('',#8134,#8131,#2344,.T.);
#10731=EDGE_CURVE('',#8135,#8136,#2345,.F.);
#10732=EDGE_CURVE('',#8136,#8137,#6367,.T.);
#10733=EDGE_CURVE('',#8137,#8138,#2346,.T.);
#10734=EDGE_CURVE('',#8138,#8135,#6368,.F.);
#10735=EDGE_CURVE('',#8139,#8140,#6369,.F.);
#10736=EDGE_CURVE('',#8140,#8141,#6370,.T.);
#10737=EDGE_CURVE('',#8142,#8141,#6371,.T.);
#10738=EDGE_CURVE('',#8142,#8143,#6372,.F.);
#10739=EDGE_CURVE('',#8144,#8143,#6373,.F.);
#10740=EDGE_CURVE('',#8144,#8145,#6374,.F.);
#10741=EDGE_CURVE('',#8145,#8146,#6375,.F.);
#10742=EDGE_CURVE('',#8146,#8147,#6376,.F.);
#10743=EDGE_CURVE('',#8148,#8147,#6377,.F.);
#10744=EDGE_CURVE('',#8148,#8139,#6378,.F.);
#10745=EDGE_CURVE('',#8149,#8149,#6379,.T.);
#10746=EDGE_CURVE('',#8150,#8150,#6380,.T.);
#10747=EDGE_CURVE('',#8151,#8151,#6381,.T.);
#10748=EDGE_CURVE('',#8152,#8152,#6382,.T.);
#10749=EDGE_CURVE('',#8141,#8153,#1403,.T.);
#10750=EDGE_CURVE('',#8153,#8154,#2347,.T.);
#10751=EDGE_CURVE('',#8154,#8155,#6383,.F.);
#10752=EDGE_CURVE('',#8155,#8156,#2348,.F.);
#10753=EDGE_CURVE('',#8156,#8142,#1404,.T.);
#10754=EDGE_CURVE('',#8157,#8158,#6384,.F.);
#10755=EDGE_CURVE('',#8158,#8159,#2349,.F.);
#10756=EDGE_CURVE('',#8159,#8160,#6385,.T.);
#10757=EDGE_CURVE('',#8160,#8157,#2350,.T.);
#10758=EDGE_CURVE('',#8161,#8162,#1405,.F.);
#10759=EDGE_CURVE('',#8163,#8161,#6386,.F.);
#10760=EDGE_CURVE('',#8164,#8163,#6387,.F.);
#10761=EDGE_CURVE('',#8165,#8164,#1406,.F.);
#10762=EDGE_CURVE('',#8166,#8165,#6388,.T.);
#10763=EDGE_CURVE('',#8166,#8167,#2351,.T.);
#10764=EDGE_CURVE('',#8167,#8168,#6389,.F.);
#10765=EDGE_CURVE('',#8168,#8167,#6390,.F.);
#10766=EDGE_CURVE('',#8162,#8166,#6391,.T.);
#10767=EDGE_CURVE('',#8113,#8115,#1407,.T.);
#10768=EDGE_CURVE('',#8103,#8105,#1408,.T.);
#10769=EDGE_CURVE('',#8093,#8095,#1409,.T.);
#10770=EDGE_CURVE('',#8083,#8085,#1410,.T.);
#10771=EDGE_CURVE('',#8073,#8075,#1411,.T.);
#10772=EDGE_CURVE('',#8169,#8170,#2352,.T.);
#10773=EDGE_CURVE('',#8170,#8171,#6392,.T.);
#10774=EDGE_CURVE('',#8172,#8171,#2353,.T.);
#10775=EDGE_CURVE('',#8172,#8169,#6393,.F.);
#10776=EDGE_CURVE('',#8173,#8174,#2354,.T.);
#10777=EDGE_CURVE('',#8174,#8170,#2355,.F.);
#10778=EDGE_CURVE('',#8169,#8173,#2356,.T.);
#10779=EDGE_CURVE('',#8175,#8176,#2357,.T.);
#10780=EDGE_CURVE('',#8176,#8177,#6394,.T.);
#10781=EDGE_CURVE('',#8178,#8177,#2358,.T.);
#10782=EDGE_CURVE('',#8178,#8175,#6395,.F.);
#10783=EDGE_CURVE('',#8177,#8179,#2359,.T.);
#10784=EDGE_CURVE('',#8180,#8179,#2360,.T.);
#10785=EDGE_CURVE('',#8180,#8178,#2361,.F.);
#10786=EDGE_CURVE('',#8179,#8174,#6396,.T.);
#10787=EDGE_CURVE('',#8173,#8180,#6397,.F.);
#10788=EDGE_CURVE('',#8181,#8182,#2362,.F.);
#10789=EDGE_CURVE('',#8182,#8183,#6398,.F.);
#10790=EDGE_CURVE('',#8183,#8184,#2363,.F.);
#10791=EDGE_CURVE('',#8184,#8185,#2364,.T.);
#10792=EDGE_CURVE('',#8185,#8186,#6399,.T.);
#10793=EDGE_CURVE('',#8186,#8187,#2365,.T.);
#10794=EDGE_CURVE('',#8187,#8188,#6400,.T.);
#10795=EDGE_CURVE('',#8188,#8189,#2366,.F.);
#10796=EDGE_CURVE('',#8189,#8190,#6401,.T.);
#10797=EDGE_CURVE('',#8190,#8181,#2367,.T.);
#10798=EDGE_CURVE('',#8191,#8191,#6402,.T.);
#10799=EDGE_CURVE('',#8192,#8192,#6403,.T.);
#10800=EDGE_CURVE('',#8193,#8193,#6404,.F.);
#10801=EDGE_CURVE('',#8194,#8195,#1412,.T.);
#10802=EDGE_CURVE('',#8195,#8196,#1413,.T.);
#10803=EDGE_CURVE('',#8196,#8197,#2368,.F.);
#10804=EDGE_CURVE('',#8197,#8198,#6405,.F.);
#10805=EDGE_CURVE('',#8198,#8199,#2369,.T.);
#10806=EDGE_CURVE('',#8199,#8200,#6406,.F.);
#10807=EDGE_CURVE('',#8200,#8201,#2370,.F.);
#10808=EDGE_CURVE('',#8201,#8202,#6407,.F.);
#10809=EDGE_CURVE('',#8202,#8203,#2371,.F.);
#10810=EDGE_CURVE('',#8203,#8204,#1414,.T.);
#10811=EDGE_CURVE('',#8204,#8205,#1415,.T.);
#10812=EDGE_CURVE('',#8205,#8194,#1416,.T.);
#10813=EDGE_CURVE('',#8206,#8207,#6408,.T.);
#10814=EDGE_CURVE('',#8207,#8206,#6409,.T.);
#10815=EDGE_CURVE('',#8208,#8209,#2372,.T.);
#10816=EDGE_CURVE('',#8209,#8210,#6410,.F.);
#10817=EDGE_CURVE('',#8211,#8210,#2373,.T.);
#10818=EDGE_CURVE('',#8211,#8208,#6411,.T.);
#10819=EDGE_CURVE('',#8210,#8209,#6412,.F.);
#10820=EDGE_CURVE('',#8208,#8211,#6413,.T.);
#10821=EDGE_CURVE('',#8212,#8213,#6414,.T.);
#10822=EDGE_CURVE('',#8213,#8214,#6415,.T.);
#10823=EDGE_CURVE('',#8214,#8215,#6416,.T.);
#10824=EDGE_CURVE('',#8216,#8215,#6417,.F.);
#10825=EDGE_CURVE('',#8216,#8217,#6418,.T.);
#10826=EDGE_CURVE('',#8217,#8218,#6419,.F.);
#10827=EDGE_CURVE('',#8135,#8218,#6420,.T.);
#10828=EDGE_CURVE('',#8219,#8138,#6421,.T.);
#10829=EDGE_CURVE('',#8219,#8220,#6422,.F.);
#10830=EDGE_CURVE('',#8220,#8221,#6423,.T.);
#10831=EDGE_CURVE('',#8212,#8221,#6424,.F.);
#10832=EDGE_CURVE('',#8222,#8222,#6425,.F.);
#10833=EDGE_CURVE('',#8223,#8223,#6426,.T.);
#10834=EDGE_CURVE('',#8224,#8225,#6427,.T.);
#10835=EDGE_CURVE('',#8225,#8224,#6428,.T.);
#10836=EDGE_CURVE('',#8224,#8226,#2374,.T.);
#10837=EDGE_CURVE('',#8226,#8227,#6429,.F.);
#10838=EDGE_CURVE('',#8227,#8226,#6430,.F.);
#10839=EDGE_CURVE('',#8228,#8229,#2375,.F.);
#10840=EDGE_CURVE('',#8229,#8230,#1417,.T.);
#10841=EDGE_CURVE('',#8230,#8231,#1418,.T.);
#10842=EDGE_CURVE('',#8231,#8232,#2376,.T.);
#10843=EDGE_CURVE('',#8232,#8233,#1419,.T.);
#10844=EDGE_CURVE('',#8233,#8176,#2377,.T.);
#10845=EDGE_CURVE('',#8175,#8234,#2378,.F.);
#10846=EDGE_CURVE('',#8234,#8235,#2379,.F.);
#10847=EDGE_CURVE('',#8228,#8235,#124,.F.);
#10848=EDGE_CURVE('',#8171,#8236,#2380,.T.);
#10849=EDGE_CURVE('',#8236,#8237,#1420,.T.);
#10850=EDGE_CURVE('',#8237,#8238,#2381,.T.);
#10851=EDGE_CURVE('',#8238,#8239,#1421,.T.);
#10852=EDGE_CURVE('',#8239,#8240,#1422,.T.);
#10853=EDGE_CURVE('',#8240,#8241,#1423,.T.);
#10854=EDGE_CURVE('',#8241,#8242,#2382,.F.);
#10855=EDGE_CURVE('',#8243,#8242,#125,.F.);
#10856=EDGE_CURVE('',#8243,#8244,#2383,.T.);
#10857=EDGE_CURVE('',#8244,#8172,#2384,.F.);
#10858=EDGE_CURVE('',#8164,#8245,#1424,.F.);
#10859=EDGE_CURVE('',#8245,#8246,#1425,.T.);
#10860=EDGE_CURVE('',#8246,#8247,#1426,.T.);
#10861=EDGE_CURVE('',#8247,#8248,#1427,.T.);
#10862=EDGE_CURVE('',#8248,#8165,#1428,.F.);
#10863=EDGE_CURVE('',#8249,#8250,#1429,.T.);
#10864=EDGE_CURVE('',#8250,#8161,#1430,.F.);
#10865=EDGE_CURVE('',#8162,#8251,#1431,.F.);
#10866=EDGE_CURVE('',#8251,#8252,#1432,.T.);
#10867=EDGE_CURVE('',#8252,#8249,#1433,.T.);
#10868=EDGE_CURVE('',#8253,#8254,#1434,.F.);
#10869=EDGE_CURVE('',#8254,#8255,#2385,.F.);
#10870=EDGE_CURVE('',#8255,#8256,#1435,.T.);
#10871=EDGE_CURVE('',#8256,#8257,#1436,.T.);
#10872=EDGE_CURVE('',#8257,#8164,#1437,.F.);
#10873=EDGE_CURVE('',#8163,#8253,#1438,.T.);
#10874=EDGE_CURVE('',#8258,#8259,#2386,.F.);
#10875=EDGE_CURVE('',#8259,#8260,#1439,.F.);
#10876=EDGE_CURVE('',#8260,#8261,#1440,.T.);
#10877=EDGE_CURVE('',#8261,#8162,#1441,.F.);
#10878=EDGE_CURVE('',#8165,#8262,#1442,.F.);
#10879=EDGE_CURVE('',#8262,#8263,#1443,.T.);
#10880=EDGE_CURVE('',#8263,#8258,#1444,.T.);
#10881=EDGE_CURVE('',#8264,#8265,#1445,.T.);
#10882=EDGE_CURVE('',#8265,#8253,#1446,.F.);
#10883=EDGE_CURVE('',#8161,#8264,#1447,.F.);
#10884=EDGE_CURVE('',#8266,#8266,#6431,.T.);
#10885=EDGE_CURVE('',#8076,#8074,#1448,.T.);
#10886=EDGE_CURVE('',#8086,#8084,#1449,.T.);
#10887=EDGE_CURVE('',#8096,#8094,#1450,.T.);
#10888=EDGE_CURVE('',#8106,#8104,#1451,.T.);
#10889=EDGE_CURVE('',#8116,#8114,#1452,.T.);
#10890=EDGE_CURVE('',#8267,#8268,#6432,.F.);
#10891=EDGE_CURVE('',#8268,#8269,#2387,.T.);
#10892=EDGE_CURVE('',#8269,#8270,#6433,.T.);
#10893=EDGE_CURVE('',#8270,#8267,#2388,.F.);
#10894=EDGE_CURVE('',#8218,#8271,#2389,.F.);
#10895=EDGE_CURVE('',#8271,#8136,#6434,.T.);
#10896=EDGE_CURVE('',#8137,#8272,#6435,.T.);
#10897=EDGE_CURVE('',#8272,#8219,#2390,.T.);
#10898=EDGE_CURVE('',#8273,#8274,#1453,.T.);
#10899=EDGE_CURVE('',#8274,#8275,#1454,.T.);
#10900=EDGE_CURVE('',#8275,#8276,#1455,.T.);
#10901=EDGE_CURVE('',#8276,#8277,#1456,.T.);
#10902=EDGE_CURVE('',#8277,#8278,#1457,.T.);
#10903=EDGE_CURVE('',#8278,#8279,#1458,.T.);
#10904=EDGE_CURVE('',#8279,#8280,#2391,.T.);
#10905=EDGE_CURVE('',#8280,#8281,#2392,.F.);
#10906=EDGE_CURVE('',#8281,#8282,#6436,.T.);
#10907=EDGE_CURVE('',#8282,#8283,#2393,.F.);
#10908=EDGE_CURVE('',#8283,#8284,#2394,.T.);
#10909=EDGE_CURVE('',#8284,#8273,#1459,.T.);
#10910=EDGE_CURVE('',#8285,#8285,#6437,.F.);
#10911=EDGE_CURVE('',#8286,#8286,#6438,.T.);
#10912=EDGE_CURVE('',#8287,#8287,#6439,.T.);
#10913=EDGE_CURVE('',#8288,#8289,#2395,.T.);
#10914=EDGE_CURVE('',#8289,#8290,#6440,.T.);
#10915=EDGE_CURVE('',#8291,#8290,#2396,.T.);
#10916=EDGE_CURVE('',#8291,#8288,#6441,.F.);
#10917=EDGE_CURVE('',#8292,#8293,#2397,.T.);
#10918=EDGE_CURVE('',#8293,#8289,#2398,.T.);
#10919=EDGE_CURVE('',#8288,#8292,#2399,.T.);
#10920=EDGE_CURVE('',#8290,#8294,#2400,.T.);
#10921=EDGE_CURVE('',#8294,#8295,#2401,.F.);
#10922=EDGE_CURVE('',#8295,#8291,#2402,.T.);
#10923=EDGE_CURVE('',#8296,#8247,#6442,.F.);
#10924=EDGE_CURVE('',#8296,#8297,#1460,.T.);
#10925=EDGE_CURVE('',#8297,#8298,#1461,.T.);
#10926=EDGE_CURVE('',#8298,#8248,#1462,.T.);
#10927=EDGE_CURVE('',#8299,#8246,#6443,.F.);
#10928=EDGE_CURVE('',#8299,#8296,#1463,.F.);
#10929=EDGE_CURVE('',#8245,#8300,#1464,.T.);
#10930=EDGE_CURVE('',#8300,#8301,#1465,.T.);
#10931=EDGE_CURVE('',#8301,#8299,#1466,.T.);
#10932=EDGE_CURVE('',#8251,#8302,#1467,.T.);
#10933=EDGE_CURVE('',#8302,#8303,#1468,.F.);
#10934=EDGE_CURVE('',#8303,#8304,#1469,.F.);
#10935=EDGE_CURVE('',#8304,#8305,#1470,.F.);
#10936=EDGE_CURVE('',#8252,#8305,#6444,.F.);
#10937=EDGE_CURVE('',#8305,#8306,#1471,.F.);
#10938=EDGE_CURVE('',#8249,#8306,#6445,.T.);
#10939=EDGE_CURVE('',#8306,#8307,#1472,.F.);
#10940=EDGE_CURVE('',#8307,#8308,#1473,.F.);
#10941=EDGE_CURVE('',#8308,#8309,#1474,.F.);
#10942=EDGE_CURVE('',#8309,#8250,#1475,.T.);
#10943=EDGE_CURVE('',#8309,#8310,#1476,.T.);
#10944=EDGE_CURVE('',#8310,#8311,#1477,.T.);
#10945=EDGE_CURVE('',#8311,#8265,#1478,.T.);
#10946=EDGE_CURVE('',#8250,#8264,#1479,.T.);
#10947=EDGE_CURVE('',#8255,#8312,#1480,.T.);
#10948=EDGE_CURVE('',#8312,#8313,#1481,.T.);
#10949=EDGE_CURVE('',#8313,#8300,#1482,.T.);
#10950=EDGE_CURVE('',#8257,#8245,#1483,.T.);
#10951=EDGE_CURVE('',#8298,#8314,#1484,.T.);
#10952=EDGE_CURVE('',#8314,#8315,#1485,.T.);
#10953=EDGE_CURVE('',#8315,#8258,#1486,.T.);
#10954=EDGE_CURVE('',#8248,#8262,#1487,.T.);
#10955=EDGE_CURVE('',#8251,#8261,#1488,.F.);
#10956=EDGE_CURVE('',#8260,#8316,#1489,.T.);
#10957=EDGE_CURVE('',#8316,#8317,#1490,.T.);
#10958=EDGE_CURVE('',#8317,#8302,#1491,.T.);
#10959=EDGE_CURVE('',#8214,#8158,#6446,.T.);
#10960=EDGE_CURVE('',#8215,#8157,#6447,.T.);
#10961=EDGE_CURVE('',#8268,#8157,#6448,.F.);
#10962=EDGE_CURVE('',#8216,#8268,#6449,.F.);
#10963=EDGE_CURVE('',#8160,#8269,#6450,.F.);
#10964=EDGE_CURVE('',#8217,#8267,#1492,.T.);
#10965=EDGE_CURVE('',#8269,#8139,#6451,.F.);
#10966=EDGE_CURVE('',#8270,#8148,#6452,.T.);
#10967=EDGE_CURVE('',#8271,#8270,#6453,.T.);
#10968=EDGE_CURVE('',#8271,#8147,#6454,.F.);
#10969=EDGE_CURVE('',#8136,#8146,#1493,.T.);
#10970=EDGE_CURVE('',#8137,#8145,#1494,.T.);
#10971=EDGE_CURVE('',#8272,#8144,#6455,.T.);
#10972=EDGE_CURVE('',#8131,#8143,#6456,.F.);
#10973=EDGE_CURVE('',#8272,#8131,#6457,.F.);
#10974=EDGE_CURVE('',#8132,#8156,#126,.F.);
#10975=EDGE_CURVE('',#8220,#8134,#1495,.T.);
#10976=EDGE_CURVE('',#8133,#8155,#6458,.T.);
#10977=EDGE_CURVE('',#8221,#8133,#6459,.T.);
#10978=EDGE_CURVE('',#8212,#8155,#6460,.F.);
#10979=EDGE_CURVE('',#8154,#8213,#6461,.F.);
#10980=EDGE_CURVE('',#8317,#8279,#1496,.F.);
#10981=EDGE_CURVE('',#8302,#8278,#6462,.T.);
#10982=EDGE_CURVE('',#8175,#8185,#6463,.T.);
#10983=EDGE_CURVE('',#8186,#8178,#6464,.T.);
#10984=EDGE_CURVE('',#8279,#8318,#1497,.T.);
#10985=EDGE_CURVE('',#8318,#8229,#1498,.T.);
#10986=EDGE_CURVE('',#8280,#8228,#6465,.T.);
#10987=EDGE_CURVE('',#8305,#8276,#6466,.F.);
#10988=EDGE_CURVE('',#8187,#8180,#6467,.T.);
#10989=EDGE_CURVE('',#8234,#8184,#6468,.T.);
#10990=EDGE_CURVE('',#8235,#8292,#6469,.T.);
#10991=EDGE_CURVE('',#8293,#8234,#6470,.T.);
#10992=EDGE_CURVE('',#8280,#8292,#127,.T.);
#10993=EDGE_CURVE('',#8306,#8275,#6471,.F.);
#10994=EDGE_CURVE('',#8188,#8173,#6472,.T.);
#10995=EDGE_CURVE('',#8293,#8184,#6473,.F.);
#10996=EDGE_CURVE('',#8281,#8288,#6474,.T.);
#10997=EDGE_CURVE('',#8309,#8273,#6475,.F.);
#10998=EDGE_CURVE('',#8189,#8169,#6476,.T.);
#10999=EDGE_CURVE('',#8289,#8183,#6477,.T.);
#11000=EDGE_CURVE('',#8282,#8291,#6478,.T.);
#11001=EDGE_CURVE('',#8284,#8310,#1499,.F.);
#11002=EDGE_CURVE('',#8190,#8172,#6479,.T.);
#11003=EDGE_CURVE('',#8290,#8182,#6480,.T.);
#11004=EDGE_CURVE('',#8283,#8295,#128,.F.);
#11005=EDGE_CURVE('',#8241,#8319,#1500,.T.);
#11006=EDGE_CURVE('',#8319,#8284,#1501,.T.);
#11007=EDGE_CURVE('',#8242,#8283,#6481,.T.);
#11008=EDGE_CURVE('',#8181,#8244,#6482,.T.);
#11009=EDGE_CURVE('',#8294,#8181,#6483,.T.);
#11010=EDGE_CURVE('',#8243,#8295,#6484,.F.);
#11011=EDGE_CURVE('',#8294,#8244,#6485,.F.);
#11012=EDGE_CURVE('',#8124,#8127,#6486,.T.);
#11013=EDGE_CURVE('',#8128,#8222,#6487,.T.);
#11014=EDGE_CURVE('',#8223,#8227,#6488,.T.);
#11015=EDGE_CURVE('',#8203,#8314,#1502,.F.);
#11016=EDGE_CURVE('',#8204,#8298,#6489,.T.);
#11017=EDGE_CURVE('',#8233,#8320,#1503,.T.);
#11018=EDGE_CURVE('',#8320,#8203,#1504,.T.);
#11019=EDGE_CURVE('',#8176,#8202,#6490,.T.);
#11020=EDGE_CURVE('',#8205,#8296,#6491,.T.);
#11021=EDGE_CURVE('',#8177,#8201,#6492,.T.);
#11022=EDGE_CURVE('',#8194,#8299,#6493,.F.);
#11023=EDGE_CURVE('',#8179,#8200,#6494,.T.);
#11024=EDGE_CURVE('',#8195,#8300,#6495,.T.);
#11025=EDGE_CURVE('',#8174,#8199,#6496,.T.);
#11026=EDGE_CURVE('',#8313,#8196,#1505,.F.);
#11027=EDGE_CURVE('',#8170,#8198,#6497,.T.);
#11028=EDGE_CURVE('',#8196,#8321,#1506,.T.);
#11029=EDGE_CURVE('',#8321,#8236,#1507,.T.);
#11030=EDGE_CURVE('',#8197,#8171,#6498,.T.);
#11031=EDGE_CURVE('',#8210,#8206,#1508,.T.);
#11032=EDGE_CURVE('',#8207,#8209,#1509,.F.);
#11033=EDGE_CURVE('',#8225,#8193,#6499,.T.);
#11034=EDGE_CURVE('',#8130,#8285,#6500,.T.);
#11035=EDGE_CURVE('',#8139,#8160,#6501,.T.);
#11036=EDGE_CURVE('',#8214,#8125,#6502,.T.);
#11037=EDGE_CURVE('',#8126,#8213,#6503,.T.);
#11038=EDGE_CURVE('',#8158,#8125,#6504,.T.);
#11039=EDGE_CURVE('',#8126,#8154,#6505,.T.);
#11040=EDGE_CURVE('',#8159,#8123,#6506,.T.);
#11041=EDGE_CURVE('',#8140,#8159,#1510,.T.);
#11042=EDGE_CURVE('',#8127,#8153,#1511,.F.);
#11043=EDGE_CURVE('',#8140,#8124,#6507,.F.);
#11044=EDGE_CURVE('',#8314,#8320,#129,.F.);
#11045=EDGE_CURVE('',#8315,#8233,#6508,.T.);
#11046=EDGE_CURVE('',#8258,#8232,#6509,.T.);
#11047=EDGE_CURVE('',#8259,#8231,#6510,.F.);
#11048=EDGE_CURVE('',#8260,#8230,#6511,.F.);
#11049=EDGE_CURVE('',#8316,#8229,#6512,.T.);
#11050=EDGE_CURVE('',#8317,#8318,#6513,.T.);
#11051=EDGE_CURVE('',#8310,#8319,#6514,.F.);
#11052=EDGE_CURVE('',#8311,#8241,#6515,.T.);
#11053=EDGE_CURVE('',#8265,#8240,#6516,.T.);
#11054=EDGE_CURVE('',#8253,#8239,#6517,.F.);
#11055=EDGE_CURVE('',#8254,#8238,#6518,.F.);
#11056=EDGE_CURVE('',#8255,#8237,#6519,.F.);
#11057=EDGE_CURVE('',#8312,#8236,#6520,.T.);
#11058=EDGE_CURVE('',#8313,#8321,#130,.T.);
#11059=EDGE_CURVE('',#8287,#8152,#2403,.T.);
#11060=EDGE_CURVE('',#8286,#8151,#2404,.T.);
#11061=EDGE_CURVE('',#8192,#8150,#2405,.T.);
#11062=EDGE_CURVE('',#8191,#8149,#2406,.T.);
#11063=EDGE_CURVE('',#8266,#8168,#6521,.T.);
#11064=EDGE_CURVE('',#8322,#8322,#6522,.T.);
#11065=EDGE_CURVE('',#8323,#8322,#6523,.T.);
#11066=EDGE_CURVE('',#8324,#8324,#6524,.T.);
#11067=EDGE_CURVE('',#8325,#8325,#6525,.T.);
#11068=EDGE_CURVE('',#8325,#8324,#2407,.T.);
#11069=ORIENTED_EDGE('',*,*,#8326,.F.);
#11070=ORIENTED_EDGE('',*,*,#8327,.F.);
#11071=ORIENTED_EDGE('',*,*,#8328,.F.);
#11072=ORIENTED_EDGE('',*,*,#8329,.F.);
#11073=ORIENTED_EDGE('',*,*,#8330,.F.);
#11074=ORIENTED_EDGE('',*,*,#8331,.F.);
#11075=ORIENTED_EDGE('',*,*,#8332,.F.);
#11076=ORIENTED_EDGE('',*,*,#8333,.F.);
#11077=ORIENTED_EDGE('',*,*,#8334,.F.);
#11078=ORIENTED_EDGE('',*,*,#8335,.F.);
#11079=ORIENTED_EDGE('',*,*,#8336,.F.);
#11080=ORIENTED_EDGE('',*,*,#8337,.F.);
#11081=ORIENTED_EDGE('',*,*,#8338,.F.);
#11082=ORIENTED_EDGE('',*,*,#8339,.F.);
#11083=ORIENTED_EDGE('',*,*,#8340,.F.);
#11084=ORIENTED_EDGE('',*,*,#8341,.F.);
#11085=ORIENTED_EDGE('',*,*,#8342,.F.);
#11086=ORIENTED_EDGE('',*,*,#8343,.F.);
#11087=ORIENTED_EDGE('',*,*,#8344,.F.);
#11088=ORIENTED_EDGE('',*,*,#8345,.F.);
#11089=ORIENTED_EDGE('',*,*,#8346,.F.);
#11090=ORIENTED_EDGE('',*,*,#8347,.F.);
#11091=ORIENTED_EDGE('',*,*,#8348,.F.);
#11092=ORIENTED_EDGE('',*,*,#8349,.F.);
#11093=ORIENTED_EDGE('',*,*,#8350,.F.);
#11094=ORIENTED_EDGE('',*,*,#8351,.F.);
#11095=ORIENTED_EDGE('',*,*,#8352,.F.);
#11096=ORIENTED_EDGE('',*,*,#8353,.F.);
#11097=ORIENTED_EDGE('',*,*,#8354,.F.);
#11098=ORIENTED_EDGE('',*,*,#8355,.F.);
#11099=ORIENTED_EDGE('',*,*,#8356,.F.);
#11100=ORIENTED_EDGE('',*,*,#8357,.F.);
#11101=ORIENTED_EDGE('',*,*,#8358,.F.);
#11102=ORIENTED_EDGE('',*,*,#8359,.F.);
#11103=ORIENTED_EDGE('',*,*,#8360,.F.);
#11104=ORIENTED_EDGE('',*,*,#8361,.F.);
#11105=ORIENTED_EDGE('',*,*,#8362,.F.);
#11106=ORIENTED_EDGE('',*,*,#8363,.F.);
#11107=ORIENTED_EDGE('',*,*,#8364,.F.);
#11108=ORIENTED_EDGE('',*,*,#8365,.F.);
#11109=ORIENTED_EDGE('',*,*,#8366,.F.);
#11110=ORIENTED_EDGE('',*,*,#8367,.F.);
#11111=ORIENTED_EDGE('',*,*,#8368,.F.);
#11112=ORIENTED_EDGE('',*,*,#8369,.F.);
#11113=ORIENTED_EDGE('',*,*,#8370,.F.);
#11114=ORIENTED_EDGE('',*,*,#8371,.F.);
#11115=ORIENTED_EDGE('',*,*,#8372,.F.);
#11116=ORIENTED_EDGE('',*,*,#8373,.F.);
#11117=ORIENTED_EDGE('',*,*,#8374,.F.);
#11118=ORIENTED_EDGE('',*,*,#8375,.F.);
#11119=ORIENTED_EDGE('',*,*,#8376,.F.);
#11120=ORIENTED_EDGE('',*,*,#8377,.F.);
#11121=ORIENTED_EDGE('',*,*,#8378,.F.);
#11122=ORIENTED_EDGE('',*,*,#8379,.F.);
#11123=ORIENTED_EDGE('',*,*,#8380,.F.);
#11124=ORIENTED_EDGE('',*,*,#8381,.F.);
#11125=ORIENTED_EDGE('',*,*,#8382,.F.);
#11126=ORIENTED_EDGE('',*,*,#8383,.F.);
#11127=ORIENTED_EDGE('',*,*,#8384,.F.);
#11128=ORIENTED_EDGE('',*,*,#8385,.F.);
#11129=ORIENTED_EDGE('',*,*,#8386,.F.);
#11130=ORIENTED_EDGE('',*,*,#8387,.F.);
#11131=ORIENTED_EDGE('',*,*,#8388,.F.);
#11132=ORIENTED_EDGE('',*,*,#8389,.F.);
#11133=ORIENTED_EDGE('',*,*,#8390,.F.);
#11134=ORIENTED_EDGE('',*,*,#8391,.F.);
#11135=ORIENTED_EDGE('',*,*,#8392,.F.);
#11136=ORIENTED_EDGE('',*,*,#8393,.F.);
#11137=ORIENTED_EDGE('',*,*,#8394,.F.);
#11138=ORIENTED_EDGE('',*,*,#8395,.F.);
#11139=ORIENTED_EDGE('',*,*,#8396,.F.);
#11140=ORIENTED_EDGE('',*,*,#8397,.F.);
#11141=ORIENTED_EDGE('',*,*,#8398,.F.);
#11142=ORIENTED_EDGE('',*,*,#8399,.F.);
#11143=ORIENTED_EDGE('',*,*,#8400,.F.);
#11144=ORIENTED_EDGE('',*,*,#8401,.F.);
#11145=ORIENTED_EDGE('',*,*,#8402,.F.);
#11146=ORIENTED_EDGE('',*,*,#8403,.F.);
#11147=ORIENTED_EDGE('',*,*,#8404,.F.);
#11148=ORIENTED_EDGE('',*,*,#8405,.F.);
#11149=ORIENTED_EDGE('',*,*,#8406,.F.);
#11150=ORIENTED_EDGE('',*,*,#8407,.F.);
#11151=ORIENTED_EDGE('',*,*,#8408,.F.);
#11152=ORIENTED_EDGE('',*,*,#8409,.F.);
#11153=ORIENTED_EDGE('',*,*,#8410,.F.);
#11154=ORIENTED_EDGE('',*,*,#8411,.F.);
#11155=ORIENTED_EDGE('',*,*,#8412,.F.);
#11156=ORIENTED_EDGE('',*,*,#8413,.F.);
#11157=ORIENTED_EDGE('',*,*,#8414,.F.);
#11158=ORIENTED_EDGE('',*,*,#8415,.F.);
#11159=ORIENTED_EDGE('',*,*,#8416,.F.);
#11160=ORIENTED_EDGE('',*,*,#8417,.F.);
#11161=ORIENTED_EDGE('',*,*,#8418,.F.);
#11162=ORIENTED_EDGE('',*,*,#8419,.F.);
#11163=ORIENTED_EDGE('',*,*,#8420,.F.);
#11164=ORIENTED_EDGE('',*,*,#8421,.F.);
#11165=ORIENTED_EDGE('',*,*,#8422,.F.);
#11166=ORIENTED_EDGE('',*,*,#8423,.F.);
#11167=ORIENTED_EDGE('',*,*,#8424,.F.);
#11168=ORIENTED_EDGE('',*,*,#8425,.F.);
#11169=ORIENTED_EDGE('',*,*,#8426,.F.);
#11170=ORIENTED_EDGE('',*,*,#8427,.F.);
#11171=ORIENTED_EDGE('',*,*,#8428,.F.);
#11172=ORIENTED_EDGE('',*,*,#8429,.F.);
#11173=ORIENTED_EDGE('',*,*,#8430,.F.);
#11174=ORIENTED_EDGE('',*,*,#8431,.F.);
#11175=ORIENTED_EDGE('',*,*,#8432,.F.);
#11176=ORIENTED_EDGE('',*,*,#8433,.F.);
#11177=ORIENTED_EDGE('',*,*,#8434,.F.);
#11178=ORIENTED_EDGE('',*,*,#8435,.F.);
#11179=ORIENTED_EDGE('',*,*,#8436,.F.);
#11180=ORIENTED_EDGE('',*,*,#8437,.F.);
#11181=ORIENTED_EDGE('',*,*,#8438,.F.);
#11182=ORIENTED_EDGE('',*,*,#8439,.F.);
#11183=ORIENTED_EDGE('',*,*,#8440,.F.);
#11184=ORIENTED_EDGE('',*,*,#8441,.F.);
#11185=ORIENTED_EDGE('',*,*,#8442,.F.);
#11186=ORIENTED_EDGE('',*,*,#8443,.F.);
#11187=ORIENTED_EDGE('',*,*,#8444,.F.);
#11188=ORIENTED_EDGE('',*,*,#8445,.F.);
#11189=ORIENTED_EDGE('',*,*,#8446,.F.);
#11190=ORIENTED_EDGE('',*,*,#8447,.F.);
#11191=ORIENTED_EDGE('',*,*,#8448,.F.);
#11192=ORIENTED_EDGE('',*,*,#8449,.F.);
#11193=ORIENTED_EDGE('',*,*,#8450,.F.);
#11194=ORIENTED_EDGE('',*,*,#8451,.F.);
#11195=ORIENTED_EDGE('',*,*,#8452,.F.);
#11196=ORIENTED_EDGE('',*,*,#8453,.F.);
#11197=ORIENTED_EDGE('',*,*,#8454,.F.);
#11198=ORIENTED_EDGE('',*,*,#8455,.F.);
#11199=ORIENTED_EDGE('',*,*,#8456,.F.);
#11200=ORIENTED_EDGE('',*,*,#8457,.F.);
#11201=ORIENTED_EDGE('',*,*,#8458,.F.);
#11202=ORIENTED_EDGE('',*,*,#8459,.F.);
#11203=ORIENTED_EDGE('',*,*,#8460,.F.);
#11204=ORIENTED_EDGE('',*,*,#8461,.F.);
#11205=ORIENTED_EDGE('',*,*,#8462,.F.);
#11206=ORIENTED_EDGE('',*,*,#8463,.F.);
#11207=ORIENTED_EDGE('',*,*,#8464,.F.);
#11208=ORIENTED_EDGE('',*,*,#8465,.F.);
#11209=ORIENTED_EDGE('',*,*,#8466,.F.);
#11210=ORIENTED_EDGE('',*,*,#8467,.F.);
#11211=ORIENTED_EDGE('',*,*,#8468,.F.);
#11212=ORIENTED_EDGE('',*,*,#8469,.F.);
#11213=ORIENTED_EDGE('',*,*,#8470,.F.);
#11214=ORIENTED_EDGE('',*,*,#8471,.F.);
#11215=ORIENTED_EDGE('',*,*,#8472,.F.);
#11216=ORIENTED_EDGE('',*,*,#8473,.F.);
#11217=ORIENTED_EDGE('',*,*,#8474,.F.);
#11218=ORIENTED_EDGE('',*,*,#8475,.F.);
#11219=ORIENTED_EDGE('',*,*,#8476,.F.);
#11220=ORIENTED_EDGE('',*,*,#8477,.F.);
#11221=ORIENTED_EDGE('',*,*,#8478,.F.);
#11222=ORIENTED_EDGE('',*,*,#8479,.F.);
#11223=ORIENTED_EDGE('',*,*,#8480,.F.);
#11224=ORIENTED_EDGE('',*,*,#8481,.F.);
#11225=ORIENTED_EDGE('',*,*,#8482,.F.);
#11226=ORIENTED_EDGE('',*,*,#8483,.F.);
#11227=ORIENTED_EDGE('',*,*,#8484,.F.);
#11228=ORIENTED_EDGE('',*,*,#8485,.F.);
#11229=ORIENTED_EDGE('',*,*,#8486,.F.);
#11230=ORIENTED_EDGE('',*,*,#8487,.F.);
#11231=ORIENTED_EDGE('',*,*,#8488,.F.);
#11232=ORIENTED_EDGE('',*,*,#8489,.F.);
#11233=ORIENTED_EDGE('',*,*,#8490,.F.);
#11234=ORIENTED_EDGE('',*,*,#8491,.F.);
#11235=ORIENTED_EDGE('',*,*,#8492,.F.);
#11236=ORIENTED_EDGE('',*,*,#8493,.F.);
#11237=ORIENTED_EDGE('',*,*,#8494,.F.);
#11238=ORIENTED_EDGE('',*,*,#8495,.F.);
#11239=ORIENTED_EDGE('',*,*,#8496,.F.);
#11240=ORIENTED_EDGE('',*,*,#8497,.F.);
#11241=ORIENTED_EDGE('',*,*,#8498,.F.);
#11242=ORIENTED_EDGE('',*,*,#8499,.F.);
#11243=ORIENTED_EDGE('',*,*,#8500,.F.);
#11244=ORIENTED_EDGE('',*,*,#8501,.F.);
#11245=ORIENTED_EDGE('',*,*,#8502,.F.);
#11246=ORIENTED_EDGE('',*,*,#8503,.F.);
#11247=ORIENTED_EDGE('',*,*,#8504,.F.);
#11248=ORIENTED_EDGE('',*,*,#8505,.F.);
#11249=ORIENTED_EDGE('',*,*,#8506,.F.);
#11250=ORIENTED_EDGE('',*,*,#8507,.F.);
#11251=ORIENTED_EDGE('',*,*,#8508,.F.);
#11252=ORIENTED_EDGE('',*,*,#8509,.F.);
#11253=ORIENTED_EDGE('',*,*,#8510,.F.);
#11254=ORIENTED_EDGE('',*,*,#8511,.F.);
#11255=ORIENTED_EDGE('',*,*,#8509,.T.);
#11256=ORIENTED_EDGE('',*,*,#8512,.F.);
#11257=ORIENTED_EDGE('',*,*,#8513,.F.);
#11258=ORIENTED_EDGE('',*,*,#8514,.F.);
#11259=ORIENTED_EDGE('',*,*,#8515,.F.);
#11260=ORIENTED_EDGE('',*,*,#8516,.F.);
#11261=ORIENTED_EDGE('',*,*,#8329,.T.);
#11262=ORIENTED_EDGE('',*,*,#8517,.F.);
#11263=ORIENTED_EDGE('',*,*,#8505,.T.);
#11264=ORIENTED_EDGE('',*,*,#8518,.F.);
#11265=ORIENTED_EDGE('',*,*,#8519,.F.);
#11266=ORIENTED_EDGE('',*,*,#8520,.F.);
#11267=ORIENTED_EDGE('',*,*,#8501,.T.);
#11268=ORIENTED_EDGE('',*,*,#8521,.F.);
#11269=ORIENTED_EDGE('',*,*,#8522,.F.);
#11270=ORIENTED_EDGE('',*,*,#8523,.F.);
#11271=ORIENTED_EDGE('',*,*,#8489,.T.);
#11272=ORIENTED_EDGE('',*,*,#8524,.F.);
#11273=ORIENTED_EDGE('',*,*,#8525,.F.);
#11274=ORIENTED_EDGE('',*,*,#8526,.F.);
#11275=ORIENTED_EDGE('',*,*,#8527,.F.);
#11276=ORIENTED_EDGE('',*,*,#8528,.F.);
#11277=ORIENTED_EDGE('',*,*,#8493,.T.);
#11278=ORIENTED_EDGE('',*,*,#8529,.F.);
#11279=ORIENTED_EDGE('',*,*,#8530,.F.);
#11280=ORIENTED_EDGE('',*,*,#8531,.F.);
#11281=ORIENTED_EDGE('',*,*,#8497,.T.);
#11282=ORIENTED_EDGE('',*,*,#8532,.F.);
#11283=ORIENTED_EDGE('',*,*,#8477,.T.);
#11284=ORIENTED_EDGE('',*,*,#8533,.F.);
#11285=ORIENTED_EDGE('',*,*,#8534,.F.);
#11286=ORIENTED_EDGE('',*,*,#8535,.F.);
#11287=ORIENTED_EDGE('',*,*,#8536,.F.);
#11288=ORIENTED_EDGE('',*,*,#8537,.F.);
#11289=ORIENTED_EDGE('',*,*,#8481,.T.);
#11290=ORIENTED_EDGE('',*,*,#8538,.F.);
#11291=ORIENTED_EDGE('',*,*,#8485,.T.);
#11292=ORIENTED_EDGE('',*,*,#8539,.F.);
#11293=ORIENTED_EDGE('',*,*,#8540,.F.);
#11294=ORIENTED_EDGE('',*,*,#8541,.F.);
#11295=ORIENTED_EDGE('',*,*,#8473,.T.);
#11296=ORIENTED_EDGE('',*,*,#8542,.F.);
#11297=ORIENTED_EDGE('',*,*,#8543,.F.);
#11298=ORIENTED_EDGE('',*,*,#8544,.F.);
#11299=ORIENTED_EDGE('',*,*,#8469,.T.);
#11300=ORIENTED_EDGE('',*,*,#8545,.F.);
#11301=ORIENTED_EDGE('',*,*,#8546,.F.);
#11302=ORIENTED_EDGE('',*,*,#8547,.F.);
#11303=ORIENTED_EDGE('',*,*,#8369,.T.);
#11304=ORIENTED_EDGE('',*,*,#8548,.F.);
#11305=ORIENTED_EDGE('',*,*,#8549,.F.);
#11306=ORIENTED_EDGE('',*,*,#8550,.F.);
#11307=ORIENTED_EDGE('',*,*,#8551,.F.);
#11308=ORIENTED_EDGE('',*,*,#8552,.F.);
#11309=ORIENTED_EDGE('',*,*,#8373,.T.);
#11310=ORIENTED_EDGE('',*,*,#8553,.F.);
#11311=ORIENTED_EDGE('',*,*,#8365,.T.);
#11312=ORIENTED_EDGE('',*,*,#8554,.F.);
#11313=ORIENTED_EDGE('',*,*,#8555,.F.);
#11314=ORIENTED_EDGE('',*,*,#8556,.F.);
#11315=ORIENTED_EDGE('',*,*,#8361,.T.);
#11316=ORIENTED_EDGE('',*,*,#8557,.F.);
#11317=ORIENTED_EDGE('',*,*,#8558,.F.);
#11318=ORIENTED_EDGE('',*,*,#8559,.F.);
#11319=ORIENTED_EDGE('',*,*,#8349,.T.);
#11320=ORIENTED_EDGE('',*,*,#8560,.F.);
#11321=ORIENTED_EDGE('',*,*,#8561,.F.);
#11322=ORIENTED_EDGE('',*,*,#8562,.F.);
#11323=ORIENTED_EDGE('',*,*,#8563,.F.);
#11324=ORIENTED_EDGE('',*,*,#8564,.F.);
#11325=ORIENTED_EDGE('',*,*,#8353,.T.);
#11326=ORIENTED_EDGE('',*,*,#8565,.F.);
#11327=ORIENTED_EDGE('',*,*,#8566,.F.);
#11328=ORIENTED_EDGE('',*,*,#8567,.F.);
#11329=ORIENTED_EDGE('',*,*,#8357,.T.);
#11330=ORIENTED_EDGE('',*,*,#8568,.F.);
#11331=ORIENTED_EDGE('',*,*,#8337,.T.);
#11332=ORIENTED_EDGE('',*,*,#8569,.F.);
#11333=ORIENTED_EDGE('',*,*,#8570,.F.);
#11334=ORIENTED_EDGE('',*,*,#8571,.F.);
#11335=ORIENTED_EDGE('',*,*,#8572,.F.);
#11336=ORIENTED_EDGE('',*,*,#8573,.F.);
#11337=ORIENTED_EDGE('',*,*,#8341,.T.);
#11338=ORIENTED_EDGE('',*,*,#8574,.F.);
#11339=ORIENTED_EDGE('',*,*,#8345,.T.);
#11340=ORIENTED_EDGE('',*,*,#8575,.F.);
#11341=ORIENTED_EDGE('',*,*,#8576,.F.);
#11342=ORIENTED_EDGE('',*,*,#8577,.F.);
#11343=ORIENTED_EDGE('',*,*,#8333,.T.);
#11344=ORIENTED_EDGE('',*,*,#8578,.F.);
#11345=ORIENTED_EDGE('',*,*,#8579,.F.);
#11346=ORIENTED_EDGE('',*,*,#8580,.F.);
#11347=ORIENTED_EDGE('',*,*,#8413,.T.);
#11348=ORIENTED_EDGE('',*,*,#8581,.F.);
#11349=ORIENTED_EDGE('',*,*,#8582,.F.);
#11350=ORIENTED_EDGE('',*,*,#8583,.F.);
#11351=ORIENTED_EDGE('',*,*,#8584,.F.);
#11352=ORIENTED_EDGE('',*,*,#8585,.F.);
#11353=ORIENTED_EDGE('',*,*,#8417,.T.);
#11354=ORIENTED_EDGE('',*,*,#8586,.F.);
#11355=ORIENTED_EDGE('',*,*,#8409,.T.);
#11356=ORIENTED_EDGE('',*,*,#8587,.F.);
#11357=ORIENTED_EDGE('',*,*,#8588,.F.);
#11358=ORIENTED_EDGE('',*,*,#8589,.F.);
#11359=ORIENTED_EDGE('',*,*,#8405,.T.);
#11360=ORIENTED_EDGE('',*,*,#8590,.F.);
#11361=ORIENTED_EDGE('',*,*,#8591,.F.);
#11362=ORIENTED_EDGE('',*,*,#8592,.F.);
#11363=ORIENTED_EDGE('',*,*,#8393,.T.);
#11364=ORIENTED_EDGE('',*,*,#8593,.F.);
#11365=ORIENTED_EDGE('',*,*,#8594,.F.);
#11366=ORIENTED_EDGE('',*,*,#8595,.F.);
#11367=ORIENTED_EDGE('',*,*,#8596,.F.);
#11368=ORIENTED_EDGE('',*,*,#8597,.F.);
#11369=ORIENTED_EDGE('',*,*,#8397,.T.);
#11370=ORIENTED_EDGE('',*,*,#8598,.F.);
#11371=ORIENTED_EDGE('',*,*,#8401,.T.);
#11372=ORIENTED_EDGE('',*,*,#8599,.F.);
#11373=ORIENTED_EDGE('',*,*,#8600,.F.);
#11374=ORIENTED_EDGE('',*,*,#8601,.F.);
#11375=ORIENTED_EDGE('',*,*,#8385,.T.);
#11376=ORIENTED_EDGE('',*,*,#8602,.F.);
#11377=ORIENTED_EDGE('',*,*,#8603,.F.);
#11378=ORIENTED_EDGE('',*,*,#8604,.F.);
#11379=ORIENTED_EDGE('',*,*,#8605,.F.);
#11380=ORIENTED_EDGE('',*,*,#8606,.F.);
#11381=ORIENTED_EDGE('',*,*,#8389,.T.);
#11382=ORIENTED_EDGE('',*,*,#8607,.F.);
#11383=ORIENTED_EDGE('',*,*,#8381,.T.);
#11384=ORIENTED_EDGE('',*,*,#8608,.F.);
#11385=ORIENTED_EDGE('',*,*,#8609,.F.);
#11386=ORIENTED_EDGE('',*,*,#8610,.F.);
#11387=ORIENTED_EDGE('',*,*,#8377,.T.);
#11388=ORIENTED_EDGE('',*,*,#8611,.F.);
#11389=ORIENTED_EDGE('',*,*,#8612,.F.);
#11390=ORIENTED_EDGE('',*,*,#8613,.F.);
#11391=ORIENTED_EDGE('',*,*,#8457,.T.);
#11392=ORIENTED_EDGE('',*,*,#8614,.F.);
#11393=ORIENTED_EDGE('',*,*,#8615,.F.);
#11394=ORIENTED_EDGE('',*,*,#8616,.F.);
#11395=ORIENTED_EDGE('',*,*,#8617,.F.);
#11396=ORIENTED_EDGE('',*,*,#8618,.F.);
#11397=ORIENTED_EDGE('',*,*,#8461,.T.);
#11398=ORIENTED_EDGE('',*,*,#8619,.F.);
#11399=ORIENTED_EDGE('',*,*,#8453,.T.);
#11400=ORIENTED_EDGE('',*,*,#8620,.F.);
#11401=ORIENTED_EDGE('',*,*,#8621,.F.);
#11402=ORIENTED_EDGE('',*,*,#8622,.F.);
#11403=ORIENTED_EDGE('',*,*,#8449,.T.);
#11404=ORIENTED_EDGE('',*,*,#8623,.F.);
#11405=ORIENTED_EDGE('',*,*,#8624,.F.);
#11406=ORIENTED_EDGE('',*,*,#8625,.F.);
#11407=ORIENTED_EDGE('',*,*,#8437,.T.);
#11408=ORIENTED_EDGE('',*,*,#8626,.F.);
#11409=ORIENTED_EDGE('',*,*,#8627,.F.);
#11410=ORIENTED_EDGE('',*,*,#8628,.F.);
#11411=ORIENTED_EDGE('',*,*,#8629,.F.);
#11412=ORIENTED_EDGE('',*,*,#8630,.F.);
#11413=ORIENTED_EDGE('',*,*,#8441,.T.);
#11414=ORIENTED_EDGE('',*,*,#8631,.F.);
#11415=ORIENTED_EDGE('',*,*,#8445,.T.);
#11416=ORIENTED_EDGE('',*,*,#8632,.F.);
#11417=ORIENTED_EDGE('',*,*,#8633,.F.);
#11418=ORIENTED_EDGE('',*,*,#8634,.F.);
#11419=ORIENTED_EDGE('',*,*,#8429,.T.);
#11420=ORIENTED_EDGE('',*,*,#8635,.F.);
#11421=ORIENTED_EDGE('',*,*,#8636,.F.);
#11422=ORIENTED_EDGE('',*,*,#8637,.F.);
#11423=ORIENTED_EDGE('',*,*,#8638,.F.);
#11424=ORIENTED_EDGE('',*,*,#8639,.F.);
#11425=ORIENTED_EDGE('',*,*,#8433,.T.);
#11426=ORIENTED_EDGE('',*,*,#8640,.F.);
#11427=ORIENTED_EDGE('',*,*,#8425,.T.);
#11428=ORIENTED_EDGE('',*,*,#8641,.F.);
#11429=ORIENTED_EDGE('',*,*,#8642,.F.);
#11430=ORIENTED_EDGE('',*,*,#8643,.F.);
#11431=ORIENTED_EDGE('',*,*,#8421,.T.);
#11432=ORIENTED_EDGE('',*,*,#8644,.F.);
#11433=ORIENTED_EDGE('',*,*,#8645,.F.);
#11434=ORIENTED_EDGE('',*,*,#8646,.T.);
#11435=ORIENTED_EDGE('',*,*,#8513,.T.);
#11436=ORIENTED_EDGE('',*,*,#8647,.F.);
#11437=ORIENTED_EDGE('',*,*,#8648,.T.);
#11438=ORIENTED_EDGE('',*,*,#8649,.T.);
#11439=ORIENTED_EDGE('',*,*,#8519,.T.);
#11440=ORIENTED_EDGE('',*,*,#8650,.F.);
#11441=ORIENTED_EDGE('',*,*,#8651,.T.);
#11442=ORIENTED_EDGE('',*,*,#8652,.T.);
#11443=ORIENTED_EDGE('',*,*,#8522,.T.);
#11444=ORIENTED_EDGE('',*,*,#8653,.F.);
#11445=ORIENTED_EDGE('',*,*,#8654,.T.);
#11446=ORIENTED_EDGE('',*,*,#8655,.T.);
#11447=ORIENTED_EDGE('',*,*,#8530,.T.);
#11448=ORIENTED_EDGE('',*,*,#8656,.F.);
#11449=ORIENTED_EDGE('',*,*,#8657,.T.);
#11450=ORIENTED_EDGE('',*,*,#8658,.T.);
#11451=ORIENTED_EDGE('',*,*,#8527,.T.);
#11452=ORIENTED_EDGE('',*,*,#8659,.F.);
#11453=ORIENTED_EDGE('',*,*,#8660,.T.);
#11454=ORIENTED_EDGE('',*,*,#8661,.T.);
#11455=ORIENTED_EDGE('',*,*,#8525,.T.);
#11456=ORIENTED_EDGE('',*,*,#8662,.F.);
#11457=ORIENTED_EDGE('',*,*,#8663,.T.);
#11458=ORIENTED_EDGE('',*,*,#8664,.T.);
#11459=ORIENTED_EDGE('',*,*,#8540,.T.);
#11460=ORIENTED_EDGE('',*,*,#8665,.F.);
#11461=ORIENTED_EDGE('',*,*,#8666,.T.);
#11462=ORIENTED_EDGE('',*,*,#8667,.T.);
#11463=ORIENTED_EDGE('',*,*,#8536,.T.);
#11464=ORIENTED_EDGE('',*,*,#8668,.F.);
#11465=ORIENTED_EDGE('',*,*,#8669,.T.);
#11466=ORIENTED_EDGE('',*,*,#8670,.T.);
#11467=ORIENTED_EDGE('',*,*,#8534,.T.);
#11468=ORIENTED_EDGE('',*,*,#8671,.F.);
#11469=ORIENTED_EDGE('',*,*,#8672,.T.);
#11470=ORIENTED_EDGE('',*,*,#8673,.T.);
#11471=ORIENTED_EDGE('',*,*,#8543,.T.);
#11472=ORIENTED_EDGE('',*,*,#8674,.F.);
#11473=ORIENTED_EDGE('',*,*,#8675,.T.);
#11474=ORIENTED_EDGE('',*,*,#8676,.T.);
#11475=ORIENTED_EDGE('',*,*,#8546,.T.);
#11476=ORIENTED_EDGE('',*,*,#8677,.F.);
#11477=ORIENTED_EDGE('',*,*,#8678,.T.);
#11478=ORIENTED_EDGE('',*,*,#8679,.T.);
#11479=ORIENTED_EDGE('',*,*,#8680,.T.);
#11480=ORIENTED_EDGE('',*,*,#8681,.F.);
#11481=ORIENTED_EDGE('',*,*,#8682,.T.);
#11482=ORIENTED_EDGE('',*,*,#8683,.T.);
#11483=ORIENTED_EDGE('',*,*,#8617,.T.);
#11484=ORIENTED_EDGE('',*,*,#8684,.F.);
#11485=ORIENTED_EDGE('',*,*,#8685,.T.);
#11486=ORIENTED_EDGE('',*,*,#8686,.T.);
#11487=ORIENTED_EDGE('',*,*,#8615,.T.);
#11488=ORIENTED_EDGE('',*,*,#8687,.F.);
#11489=ORIENTED_EDGE('',*,*,#8688,.T.);
#11490=ORIENTED_EDGE('',*,*,#8689,.T.);
#11491=ORIENTED_EDGE('',*,*,#8621,.T.);
#11492=ORIENTED_EDGE('',*,*,#8690,.F.);
#11493=ORIENTED_EDGE('',*,*,#8691,.T.);
#11494=ORIENTED_EDGE('',*,*,#8692,.T.);
#11495=ORIENTED_EDGE('',*,*,#8624,.T.);
#11496=ORIENTED_EDGE('',*,*,#8693,.F.);
#11497=ORIENTED_EDGE('',*,*,#8694,.T.);
#11498=ORIENTED_EDGE('',*,*,#8695,.T.);
#11499=ORIENTED_EDGE('',*,*,#8633,.T.);
#11500=ORIENTED_EDGE('',*,*,#8696,.F.);
#11501=ORIENTED_EDGE('',*,*,#8697,.T.);
#11502=ORIENTED_EDGE('',*,*,#8698,.T.);
#11503=ORIENTED_EDGE('',*,*,#8629,.T.);
#11504=ORIENTED_EDGE('',*,*,#8699,.F.);
#11505=ORIENTED_EDGE('',*,*,#8700,.T.);
#11506=ORIENTED_EDGE('',*,*,#8701,.T.);
#11507=ORIENTED_EDGE('',*,*,#8627,.T.);
#11508=ORIENTED_EDGE('',*,*,#8702,.F.);
#11509=ORIENTED_EDGE('',*,*,#8703,.T.);
#11510=ORIENTED_EDGE('',*,*,#8704,.T.);
#11511=ORIENTED_EDGE('',*,*,#8638,.T.);
#11512=ORIENTED_EDGE('',*,*,#8705,.F.);
#11513=ORIENTED_EDGE('',*,*,#8706,.T.);
#11514=ORIENTED_EDGE('',*,*,#8707,.T.);
#11515=ORIENTED_EDGE('',*,*,#8636,.T.);
#11516=ORIENTED_EDGE('',*,*,#8708,.F.);
#11517=ORIENTED_EDGE('',*,*,#8709,.T.);
#11518=ORIENTED_EDGE('',*,*,#8710,.T.);
#11519=ORIENTED_EDGE('',*,*,#8642,.T.);
#11520=ORIENTED_EDGE('',*,*,#8711,.F.);
#11521=ORIENTED_EDGE('',*,*,#8712,.T.);
#11522=ORIENTED_EDGE('',*,*,#8713,.T.);
#11523=ORIENTED_EDGE('',*,*,#8645,.T.);
#11524=ORIENTED_EDGE('',*,*,#8714,.F.);
#11525=ORIENTED_EDGE('',*,*,#8715,.T.);
#11526=ORIENTED_EDGE('',*,*,#8716,.T.);
#11527=ORIENTED_EDGE('',*,*,#8584,.T.);
#11528=ORIENTED_EDGE('',*,*,#8717,.F.);
#11529=ORIENTED_EDGE('',*,*,#8718,.T.);
#11530=ORIENTED_EDGE('',*,*,#8719,.T.);
#11531=ORIENTED_EDGE('',*,*,#8582,.T.);
#11532=ORIENTED_EDGE('',*,*,#8720,.F.);
#11533=ORIENTED_EDGE('',*,*,#8721,.T.);
#11534=ORIENTED_EDGE('',*,*,#8722,.T.);
#11535=ORIENTED_EDGE('',*,*,#8588,.T.);
#11536=ORIENTED_EDGE('',*,*,#8723,.F.);
#11537=ORIENTED_EDGE('',*,*,#8724,.T.);
#11538=ORIENTED_EDGE('',*,*,#8725,.T.);
#11539=ORIENTED_EDGE('',*,*,#8591,.T.);
#11540=ORIENTED_EDGE('',*,*,#8726,.F.);
#11541=ORIENTED_EDGE('',*,*,#8727,.T.);
#11542=ORIENTED_EDGE('',*,*,#8728,.T.);
#11543=ORIENTED_EDGE('',*,*,#8600,.T.);
#11544=ORIENTED_EDGE('',*,*,#8729,.F.);
#11545=ORIENTED_EDGE('',*,*,#8730,.T.);
#11546=ORIENTED_EDGE('',*,*,#8731,.T.);
#11547=ORIENTED_EDGE('',*,*,#8596,.T.);
#11548=ORIENTED_EDGE('',*,*,#8732,.F.);
#11549=ORIENTED_EDGE('',*,*,#8733,.T.);
#11550=ORIENTED_EDGE('',*,*,#8734,.T.);
#11551=ORIENTED_EDGE('',*,*,#8594,.T.);
#11552=ORIENTED_EDGE('',*,*,#8735,.F.);
#11553=ORIENTED_EDGE('',*,*,#8736,.T.);
#11554=ORIENTED_EDGE('',*,*,#8737,.T.);
#11555=ORIENTED_EDGE('',*,*,#8605,.T.);
#11556=ORIENTED_EDGE('',*,*,#8738,.F.);
#11557=ORIENTED_EDGE('',*,*,#8739,.T.);
#11558=ORIENTED_EDGE('',*,*,#8740,.T.);
#11559=ORIENTED_EDGE('',*,*,#8603,.T.);
#11560=ORIENTED_EDGE('',*,*,#8741,.F.);
#11561=ORIENTED_EDGE('',*,*,#8742,.T.);
#11562=ORIENTED_EDGE('',*,*,#8743,.T.);
#11563=ORIENTED_EDGE('',*,*,#8609,.T.);
#11564=ORIENTED_EDGE('',*,*,#8744,.F.);
#11565=ORIENTED_EDGE('',*,*,#8745,.T.);
#11566=ORIENTED_EDGE('',*,*,#8746,.T.);
#11567=ORIENTED_EDGE('',*,*,#8612,.T.);
#11568=ORIENTED_EDGE('',*,*,#8747,.F.);
#11569=ORIENTED_EDGE('',*,*,#8748,.T.);
#11570=ORIENTED_EDGE('',*,*,#8749,.T.);
#11571=ORIENTED_EDGE('',*,*,#8551,.T.);
#11572=ORIENTED_EDGE('',*,*,#8750,.F.);
#11573=ORIENTED_EDGE('',*,*,#8751,.T.);
#11574=ORIENTED_EDGE('',*,*,#8752,.T.);
#11575=ORIENTED_EDGE('',*,*,#8549,.T.);
#11576=ORIENTED_EDGE('',*,*,#8753,.F.);
#11577=ORIENTED_EDGE('',*,*,#8754,.T.);
#11578=ORIENTED_EDGE('',*,*,#8755,.T.);
#11579=ORIENTED_EDGE('',*,*,#8555,.T.);
#11580=ORIENTED_EDGE('',*,*,#8756,.F.);
#11581=ORIENTED_EDGE('',*,*,#8757,.T.);
#11582=ORIENTED_EDGE('',*,*,#8758,.T.);
#11583=ORIENTED_EDGE('',*,*,#8558,.T.);
#11584=ORIENTED_EDGE('',*,*,#8759,.F.);
#11585=ORIENTED_EDGE('',*,*,#8760,.T.);
#11586=ORIENTED_EDGE('',*,*,#8761,.T.);
#11587=ORIENTED_EDGE('',*,*,#8566,.T.);
#11588=ORIENTED_EDGE('',*,*,#8762,.F.);
#11589=ORIENTED_EDGE('',*,*,#8763,.T.);
#11590=ORIENTED_EDGE('',*,*,#8764,.T.);
#11591=ORIENTED_EDGE('',*,*,#8563,.T.);
#11592=ORIENTED_EDGE('',*,*,#8765,.F.);
#11593=ORIENTED_EDGE('',*,*,#8766,.T.);
#11594=ORIENTED_EDGE('',*,*,#8767,.T.);
#11595=ORIENTED_EDGE('',*,*,#8561,.T.);
#11596=ORIENTED_EDGE('',*,*,#8768,.F.);
#11597=ORIENTED_EDGE('',*,*,#8769,.T.);
#11598=ORIENTED_EDGE('',*,*,#8770,.T.);
#11599=ORIENTED_EDGE('',*,*,#8576,.T.);
#11600=ORIENTED_EDGE('',*,*,#8771,.F.);
#11601=ORIENTED_EDGE('',*,*,#8772,.T.);
#11602=ORIENTED_EDGE('',*,*,#8773,.T.);
#11603=ORIENTED_EDGE('',*,*,#8572,.T.);
#11604=ORIENTED_EDGE('',*,*,#8774,.F.);
#11605=ORIENTED_EDGE('',*,*,#8775,.T.);
#11606=ORIENTED_EDGE('',*,*,#8776,.T.);
#11607=ORIENTED_EDGE('',*,*,#8570,.T.);
#11608=ORIENTED_EDGE('',*,*,#8777,.F.);
#11609=ORIENTED_EDGE('',*,*,#8778,.T.);
#11610=ORIENTED_EDGE('',*,*,#8779,.T.);
#11611=ORIENTED_EDGE('',*,*,#8579,.T.);
#11612=ORIENTED_EDGE('',*,*,#8780,.F.);
#11613=ORIENTED_EDGE('',*,*,#8781,.T.);
#11614=ORIENTED_EDGE('',*,*,#8782,.T.);
#11615=ORIENTED_EDGE('',*,*,#8515,.T.);
#11616=ORIENTED_EDGE('',*,*,#8783,.F.);
#11617=ORIENTED_EDGE('',*,*,#8784,.T.);
#11618=ORIENTED_EDGE('',*,*,#8785,.F.);
#11619=ORIENTED_EDGE('',*,*,#8786,.F.);
#11620=ORIENTED_EDGE('',*,*,#8465,.T.);
#11621=ORIENTED_EDGE('',*,*,#8787,.F.);
#11622=ORIENTED_EDGE('',*,*,#8680,.F.);
#11623=ORIENTED_EDGE('',*,*,#8618,.T.);
#11624=ORIENTED_EDGE('',*,*,#8683,.F.);
#11625=ORIENTED_EDGE('',*,*,#8788,.F.);
#11626=ORIENTED_EDGE('',*,*,#8462,.T.);
#11627=ORIENTED_EDGE('',*,*,#8787,.T.);
#11628=ORIENTED_EDGE('',*,*,#8464,.T.);
#11629=ORIENTED_EDGE('',*,*,#8789,.T.);
#11630=ORIENTED_EDGE('',*,*,#8681,.T.);
#11631=ORIENTED_EDGE('',*,*,#8682,.F.);
#11632=ORIENTED_EDGE('',*,*,#8789,.F.);
#11633=ORIENTED_EDGE('',*,*,#8463,.T.);
#11634=ORIENTED_EDGE('',*,*,#8788,.T.);
#11635=ORIENTED_EDGE('',*,*,#8786,.T.);
#11636=ORIENTED_EDGE('',*,*,#8679,.F.);
#11637=ORIENTED_EDGE('',*,*,#8790,.F.);
#11638=ORIENTED_EDGE('',*,*,#8466,.T.);
#11639=ORIENTED_EDGE('',*,*,#8545,.T.);
#11640=ORIENTED_EDGE('',*,*,#8468,.T.);
#11641=ORIENTED_EDGE('',*,*,#8791,.T.);
#11642=ORIENTED_EDGE('',*,*,#8677,.T.);
#11643=ORIENTED_EDGE('',*,*,#8678,.F.);
#11644=ORIENTED_EDGE('',*,*,#8791,.F.);
#11645=ORIENTED_EDGE('',*,*,#8467,.T.);
#11646=ORIENTED_EDGE('',*,*,#8790,.T.);
#11647=ORIENTED_EDGE('',*,*,#8585,.T.);
#11648=ORIENTED_EDGE('',*,*,#8716,.F.);
#11649=ORIENTED_EDGE('',*,*,#8792,.F.);
#11650=ORIENTED_EDGE('',*,*,#8418,.T.);
#11651=ORIENTED_EDGE('',*,*,#8644,.T.);
#11652=ORIENTED_EDGE('',*,*,#8420,.T.);
#11653=ORIENTED_EDGE('',*,*,#8793,.T.);
#11654=ORIENTED_EDGE('',*,*,#8714,.T.);
#11655=ORIENTED_EDGE('',*,*,#8715,.F.);
#11656=ORIENTED_EDGE('',*,*,#8793,.F.);
#11657=ORIENTED_EDGE('',*,*,#8419,.T.);
#11658=ORIENTED_EDGE('',*,*,#8792,.T.);
#11659=ORIENTED_EDGE('',*,*,#8643,.T.);
#11660=ORIENTED_EDGE('',*,*,#8713,.F.);
#11661=ORIENTED_EDGE('',*,*,#8794,.F.);
#11662=ORIENTED_EDGE('',*,*,#8422,.T.);
#11663=ORIENTED_EDGE('',*,*,#8641,.T.);
#11664=ORIENTED_EDGE('',*,*,#8424,.T.);
#11665=ORIENTED_EDGE('',*,*,#8795,.T.);
#11666=ORIENTED_EDGE('',*,*,#8711,.T.);
#11667=ORIENTED_EDGE('',*,*,#8712,.F.);
#11668=ORIENTED_EDGE('',*,*,#8795,.F.);
#11669=ORIENTED_EDGE('',*,*,#8423,.T.);
#11670=ORIENTED_EDGE('',*,*,#8794,.T.);
#11671=ORIENTED_EDGE('',*,*,#8640,.T.);
#11672=ORIENTED_EDGE('',*,*,#8710,.F.);
#11673=ORIENTED_EDGE('',*,*,#8796,.F.);
#11674=ORIENTED_EDGE('',*,*,#8426,.T.);
#11675=ORIENTED_EDGE('',*,*,#8635,.T.);
#11676=ORIENTED_EDGE('',*,*,#8428,.T.);
#11677=ORIENTED_EDGE('',*,*,#8797,.T.);
#11678=ORIENTED_EDGE('',*,*,#8708,.T.);
#11679=ORIENTED_EDGE('',*,*,#8709,.F.);
#11680=ORIENTED_EDGE('',*,*,#8797,.F.);
#11681=ORIENTED_EDGE('',*,*,#8427,.T.);
#11682=ORIENTED_EDGE('',*,*,#8796,.T.);
#11683=ORIENTED_EDGE('',*,*,#8639,.T.);
#11684=ORIENTED_EDGE('',*,*,#8704,.F.);
#11685=ORIENTED_EDGE('',*,*,#8798,.F.);
#11686=ORIENTED_EDGE('',*,*,#8434,.T.);
#11687=ORIENTED_EDGE('',*,*,#8626,.T.);
#11688=ORIENTED_EDGE('',*,*,#8436,.T.);
#11689=ORIENTED_EDGE('',*,*,#8799,.T.);
#11690=ORIENTED_EDGE('',*,*,#8702,.T.);
#11691=ORIENTED_EDGE('',*,*,#8703,.F.);
#11692=ORIENTED_EDGE('',*,*,#8799,.F.);
#11693=ORIENTED_EDGE('',*,*,#8435,.T.);
#11694=ORIENTED_EDGE('',*,*,#8798,.T.);
#11695=ORIENTED_EDGE('',*,*,#8634,.T.);
#11696=ORIENTED_EDGE('',*,*,#8707,.F.);
#11697=ORIENTED_EDGE('',*,*,#8800,.F.);
#11698=ORIENTED_EDGE('',*,*,#8430,.T.);
#11699=ORIENTED_EDGE('',*,*,#8637,.T.);
#11700=ORIENTED_EDGE('',*,*,#8432,.T.);
#11701=ORIENTED_EDGE('',*,*,#8801,.T.);
#11702=ORIENTED_EDGE('',*,*,#8705,.T.);
#11703=ORIENTED_EDGE('',*,*,#8706,.F.);
#11704=ORIENTED_EDGE('',*,*,#8801,.F.);
#11705=ORIENTED_EDGE('',*,*,#8431,.T.);
#11706=ORIENTED_EDGE('',*,*,#8800,.T.);
#11707=ORIENTED_EDGE('',*,*,#8630,.T.);
#11708=ORIENTED_EDGE('',*,*,#8698,.F.);
#11709=ORIENTED_EDGE('',*,*,#8802,.F.);
#11710=ORIENTED_EDGE('',*,*,#8442,.T.);
#11711=ORIENTED_EDGE('',*,*,#8632,.T.);
#11712=ORIENTED_EDGE('',*,*,#8444,.T.);
#11713=ORIENTED_EDGE('',*,*,#8803,.T.);
#11714=ORIENTED_EDGE('',*,*,#8696,.T.);
#11715=ORIENTED_EDGE('',*,*,#8697,.F.);
#11716=ORIENTED_EDGE('',*,*,#8803,.F.);
#11717=ORIENTED_EDGE('',*,*,#8443,.T.);
#11718=ORIENTED_EDGE('',*,*,#8802,.T.);
#11719=ORIENTED_EDGE('',*,*,#8631,.T.);
#11720=ORIENTED_EDGE('',*,*,#8695,.F.);
#11721=ORIENTED_EDGE('',*,*,#8804,.F.);
#11722=ORIENTED_EDGE('',*,*,#8446,.T.);
#11723=ORIENTED_EDGE('',*,*,#8623,.T.);
#11724=ORIENTED_EDGE('',*,*,#8448,.T.);
#11725=ORIENTED_EDGE('',*,*,#8805,.T.);
#11726=ORIENTED_EDGE('',*,*,#8693,.T.);
#11727=ORIENTED_EDGE('',*,*,#8694,.F.);
#11728=ORIENTED_EDGE('',*,*,#8805,.F.);
#11729=ORIENTED_EDGE('',*,*,#8447,.T.);
#11730=ORIENTED_EDGE('',*,*,#8804,.T.);
#11731=ORIENTED_EDGE('',*,*,#8625,.T.);
#11732=ORIENTED_EDGE('',*,*,#8701,.F.);
#11733=ORIENTED_EDGE('',*,*,#8806,.F.);
#11734=ORIENTED_EDGE('',*,*,#8438,.T.);
#11735=ORIENTED_EDGE('',*,*,#8628,.T.);
#11736=ORIENTED_EDGE('',*,*,#8440,.T.);
#11737=ORIENTED_EDGE('',*,*,#8807,.T.);
#11738=ORIENTED_EDGE('',*,*,#8699,.T.);
#11739=ORIENTED_EDGE('',*,*,#8700,.F.);
#11740=ORIENTED_EDGE('',*,*,#8807,.F.);
#11741=ORIENTED_EDGE('',*,*,#8439,.T.);
#11742=ORIENTED_EDGE('',*,*,#8806,.T.);
#11743=ORIENTED_EDGE('',*,*,#8622,.T.);
#11744=ORIENTED_EDGE('',*,*,#8692,.F.);
#11745=ORIENTED_EDGE('',*,*,#8808,.F.);
#11746=ORIENTED_EDGE('',*,*,#8450,.T.);
#11747=ORIENTED_EDGE('',*,*,#8620,.T.);
#11748=ORIENTED_EDGE('',*,*,#8452,.T.);
#11749=ORIENTED_EDGE('',*,*,#8809,.T.);
#11750=ORIENTED_EDGE('',*,*,#8690,.T.);
#11751=ORIENTED_EDGE('',*,*,#8691,.F.);
#11752=ORIENTED_EDGE('',*,*,#8809,.F.);
#11753=ORIENTED_EDGE('',*,*,#8451,.T.);
#11754=ORIENTED_EDGE('',*,*,#8808,.T.);
#11755=ORIENTED_EDGE('',*,*,#8619,.T.);
#11756=ORIENTED_EDGE('',*,*,#8689,.F.);
#11757=ORIENTED_EDGE('',*,*,#8810,.F.);
#11758=ORIENTED_EDGE('',*,*,#8454,.T.);
#11759=ORIENTED_EDGE('',*,*,#8614,.T.);
#11760=ORIENTED_EDGE('',*,*,#8456,.T.);
#11761=ORIENTED_EDGE('',*,*,#8811,.T.);
#11762=ORIENTED_EDGE('',*,*,#8687,.T.);
#11763=ORIENTED_EDGE('',*,*,#8688,.F.);
#11764=ORIENTED_EDGE('',*,*,#8811,.F.);
#11765=ORIENTED_EDGE('',*,*,#8455,.T.);
#11766=ORIENTED_EDGE('',*,*,#8810,.T.);
#11767=ORIENTED_EDGE('',*,*,#8613,.T.);
#11768=ORIENTED_EDGE('',*,*,#8686,.F.);
#11769=ORIENTED_EDGE('',*,*,#8812,.F.);
#11770=ORIENTED_EDGE('',*,*,#8458,.T.);
#11771=ORIENTED_EDGE('',*,*,#8616,.T.);
#11772=ORIENTED_EDGE('',*,*,#8460,.T.);
#11773=ORIENTED_EDGE('',*,*,#8813,.T.);
#11774=ORIENTED_EDGE('',*,*,#8684,.T.);
#11775=ORIENTED_EDGE('',*,*,#8685,.F.);
#11776=ORIENTED_EDGE('',*,*,#8813,.F.);
#11777=ORIENTED_EDGE('',*,*,#8459,.T.);
#11778=ORIENTED_EDGE('',*,*,#8812,.T.);
#11779=ORIENTED_EDGE('',*,*,#8552,.T.);
#11780=ORIENTED_EDGE('',*,*,#8749,.F.);
#11781=ORIENTED_EDGE('',*,*,#8814,.F.);
#11782=ORIENTED_EDGE('',*,*,#8374,.T.);
#11783=ORIENTED_EDGE('',*,*,#8611,.T.);
#11784=ORIENTED_EDGE('',*,*,#8376,.T.);
#11785=ORIENTED_EDGE('',*,*,#8815,.T.);
#11786=ORIENTED_EDGE('',*,*,#8747,.T.);
#11787=ORIENTED_EDGE('',*,*,#8748,.F.);
#11788=ORIENTED_EDGE('',*,*,#8815,.F.);
#11789=ORIENTED_EDGE('',*,*,#8375,.T.);
#11790=ORIENTED_EDGE('',*,*,#8814,.T.);
#11791=ORIENTED_EDGE('',*,*,#8610,.T.);
#11792=ORIENTED_EDGE('',*,*,#8746,.F.);
#11793=ORIENTED_EDGE('',*,*,#8816,.F.);
#11794=ORIENTED_EDGE('',*,*,#8378,.T.);
#11795=ORIENTED_EDGE('',*,*,#8608,.T.);
#11796=ORIENTED_EDGE('',*,*,#8380,.T.);
#11797=ORIENTED_EDGE('',*,*,#8817,.T.);
#11798=ORIENTED_EDGE('',*,*,#8744,.T.);
#11799=ORIENTED_EDGE('',*,*,#8745,.F.);
#11800=ORIENTED_EDGE('',*,*,#8817,.F.);
#11801=ORIENTED_EDGE('',*,*,#8379,.T.);
#11802=ORIENTED_EDGE('',*,*,#8816,.T.);
#11803=ORIENTED_EDGE('',*,*,#8607,.T.);
#11804=ORIENTED_EDGE('',*,*,#8743,.F.);
#11805=ORIENTED_EDGE('',*,*,#8818,.F.);
#11806=ORIENTED_EDGE('',*,*,#8382,.T.);
#11807=ORIENTED_EDGE('',*,*,#8602,.T.);
#11808=ORIENTED_EDGE('',*,*,#8384,.T.);
#11809=ORIENTED_EDGE('',*,*,#8819,.T.);
#11810=ORIENTED_EDGE('',*,*,#8741,.T.);
#11811=ORIENTED_EDGE('',*,*,#8742,.F.);
#11812=ORIENTED_EDGE('',*,*,#8819,.F.);
#11813=ORIENTED_EDGE('',*,*,#8383,.T.);
#11814=ORIENTED_EDGE('',*,*,#8818,.T.);
#11815=ORIENTED_EDGE('',*,*,#8606,.T.);
#11816=ORIENTED_EDGE('',*,*,#8737,.F.);
#11817=ORIENTED_EDGE('',*,*,#8820,.F.);
#11818=ORIENTED_EDGE('',*,*,#8390,.T.);
#11819=ORIENTED_EDGE('',*,*,#8593,.T.);
#11820=ORIENTED_EDGE('',*,*,#8392,.T.);
#11821=ORIENTED_EDGE('',*,*,#8821,.T.);
#11822=ORIENTED_EDGE('',*,*,#8735,.T.);
#11823=ORIENTED_EDGE('',*,*,#8736,.F.);
#11824=ORIENTED_EDGE('',*,*,#8821,.F.);
#11825=ORIENTED_EDGE('',*,*,#8391,.T.);
#11826=ORIENTED_EDGE('',*,*,#8820,.T.);
#11827=ORIENTED_EDGE('',*,*,#8601,.T.);
#11828=ORIENTED_EDGE('',*,*,#8740,.F.);
#11829=ORIENTED_EDGE('',*,*,#8822,.F.);
#11830=ORIENTED_EDGE('',*,*,#8386,.T.);
#11831=ORIENTED_EDGE('',*,*,#8604,.T.);
#11832=ORIENTED_EDGE('',*,*,#8388,.T.);
#11833=ORIENTED_EDGE('',*,*,#8823,.T.);
#11834=ORIENTED_EDGE('',*,*,#8738,.T.);
#11835=ORIENTED_EDGE('',*,*,#8739,.F.);
#11836=ORIENTED_EDGE('',*,*,#8823,.F.);
#11837=ORIENTED_EDGE('',*,*,#8387,.T.);
#11838=ORIENTED_EDGE('',*,*,#8822,.T.);
#11839=ORIENTED_EDGE('',*,*,#8597,.T.);
#11840=ORIENTED_EDGE('',*,*,#8731,.F.);
#11841=ORIENTED_EDGE('',*,*,#8824,.F.);
#11842=ORIENTED_EDGE('',*,*,#8398,.T.);
#11843=ORIENTED_EDGE('',*,*,#8599,.T.);
#11844=ORIENTED_EDGE('',*,*,#8400,.T.);
#11845=ORIENTED_EDGE('',*,*,#8825,.T.);
#11846=ORIENTED_EDGE('',*,*,#8729,.T.);
#11847=ORIENTED_EDGE('',*,*,#8730,.F.);
#11848=ORIENTED_EDGE('',*,*,#8825,.F.);
#11849=ORIENTED_EDGE('',*,*,#8399,.T.);
#11850=ORIENTED_EDGE('',*,*,#8824,.T.);
#11851=ORIENTED_EDGE('',*,*,#8598,.T.);
#11852=ORIENTED_EDGE('',*,*,#8728,.F.);
#11853=ORIENTED_EDGE('',*,*,#8826,.F.);
#11854=ORIENTED_EDGE('',*,*,#8402,.T.);
#11855=ORIENTED_EDGE('',*,*,#8590,.T.);
#11856=ORIENTED_EDGE('',*,*,#8404,.T.);
#11857=ORIENTED_EDGE('',*,*,#8827,.T.);
#11858=ORIENTED_EDGE('',*,*,#8726,.T.);
#11859=ORIENTED_EDGE('',*,*,#8727,.F.);
#11860=ORIENTED_EDGE('',*,*,#8827,.F.);
#11861=ORIENTED_EDGE('',*,*,#8403,.T.);
#11862=ORIENTED_EDGE('',*,*,#8826,.T.);
#11863=ORIENTED_EDGE('',*,*,#8592,.T.);
#11864=ORIENTED_EDGE('',*,*,#8734,.F.);
#11865=ORIENTED_EDGE('',*,*,#8828,.F.);
#11866=ORIENTED_EDGE('',*,*,#8394,.T.);
#11867=ORIENTED_EDGE('',*,*,#8595,.T.);
#11868=ORIENTED_EDGE('',*,*,#8396,.T.);
#11869=ORIENTED_EDGE('',*,*,#8829,.T.);
#11870=ORIENTED_EDGE('',*,*,#8732,.T.);
#11871=ORIENTED_EDGE('',*,*,#8733,.F.);
#11872=ORIENTED_EDGE('',*,*,#8829,.F.);
#11873=ORIENTED_EDGE('',*,*,#8395,.T.);
#11874=ORIENTED_EDGE('',*,*,#8828,.T.);
#11875=ORIENTED_EDGE('',*,*,#8589,.T.);
#11876=ORIENTED_EDGE('',*,*,#8725,.F.);
#11877=ORIENTED_EDGE('',*,*,#8830,.F.);
#11878=ORIENTED_EDGE('',*,*,#8406,.T.);
#11879=ORIENTED_EDGE('',*,*,#8587,.T.);
#11880=ORIENTED_EDGE('',*,*,#8408,.T.);
#11881=ORIENTED_EDGE('',*,*,#8831,.T.);
#11882=ORIENTED_EDGE('',*,*,#8723,.T.);
#11883=ORIENTED_EDGE('',*,*,#8724,.F.);
#11884=ORIENTED_EDGE('',*,*,#8831,.F.);
#11885=ORIENTED_EDGE('',*,*,#8407,.T.);
#11886=ORIENTED_EDGE('',*,*,#8830,.T.);
#11887=ORIENTED_EDGE('',*,*,#8586,.T.);
#11888=ORIENTED_EDGE('',*,*,#8722,.F.);
#11889=ORIENTED_EDGE('',*,*,#8832,.F.);
#11890=ORIENTED_EDGE('',*,*,#8410,.T.);
#11891=ORIENTED_EDGE('',*,*,#8581,.T.);
#11892=ORIENTED_EDGE('',*,*,#8412,.T.);
#11893=ORIENTED_EDGE('',*,*,#8833,.T.);
#11894=ORIENTED_EDGE('',*,*,#8720,.T.);
#11895=ORIENTED_EDGE('',*,*,#8721,.F.);
#11896=ORIENTED_EDGE('',*,*,#8833,.F.);
#11897=ORIENTED_EDGE('',*,*,#8411,.T.);
#11898=ORIENTED_EDGE('',*,*,#8832,.T.);
#11899=ORIENTED_EDGE('',*,*,#8580,.T.);
#11900=ORIENTED_EDGE('',*,*,#8719,.F.);
#11901=ORIENTED_EDGE('',*,*,#8834,.F.);
#11902=ORIENTED_EDGE('',*,*,#8414,.T.);
#11903=ORIENTED_EDGE('',*,*,#8583,.T.);
#11904=ORIENTED_EDGE('',*,*,#8416,.T.);
#11905=ORIENTED_EDGE('',*,*,#8835,.T.);
#11906=ORIENTED_EDGE('',*,*,#8717,.T.);
#11907=ORIENTED_EDGE('',*,*,#8718,.F.);
#11908=ORIENTED_EDGE('',*,*,#8835,.F.);
#11909=ORIENTED_EDGE('',*,*,#8415,.T.);
#11910=ORIENTED_EDGE('',*,*,#8834,.T.);
#11911=ORIENTED_EDGE('',*,*,#8516,.T.);
#11912=ORIENTED_EDGE('',*,*,#8782,.F.);
#11913=ORIENTED_EDGE('',*,*,#8836,.F.);
#11914=ORIENTED_EDGE('',*,*,#8330,.T.);
#11915=ORIENTED_EDGE('',*,*,#8578,.T.);
#11916=ORIENTED_EDGE('',*,*,#8332,.T.);
#11917=ORIENTED_EDGE('',*,*,#8837,.T.);
#11918=ORIENTED_EDGE('',*,*,#8780,.T.);
#11919=ORIENTED_EDGE('',*,*,#8781,.F.);
#11920=ORIENTED_EDGE('',*,*,#8837,.F.);
#11921=ORIENTED_EDGE('',*,*,#8331,.T.);
#11922=ORIENTED_EDGE('',*,*,#8836,.T.);
#11923=ORIENTED_EDGE('',*,*,#8577,.T.);
#11924=ORIENTED_EDGE('',*,*,#8779,.F.);
#11925=ORIENTED_EDGE('',*,*,#8838,.F.);
#11926=ORIENTED_EDGE('',*,*,#8334,.T.);
#11927=ORIENTED_EDGE('',*,*,#8569,.T.);
#11928=ORIENTED_EDGE('',*,*,#8336,.T.);
#11929=ORIENTED_EDGE('',*,*,#8839,.T.);
#11930=ORIENTED_EDGE('',*,*,#8777,.T.);
#11931=ORIENTED_EDGE('',*,*,#8778,.F.);
#11932=ORIENTED_EDGE('',*,*,#8839,.F.);
#11933=ORIENTED_EDGE('',*,*,#8335,.T.);
#11934=ORIENTED_EDGE('',*,*,#8838,.T.);
#11935=ORIENTED_EDGE('',*,*,#8573,.T.);
#11936=ORIENTED_EDGE('',*,*,#8773,.F.);
#11937=ORIENTED_EDGE('',*,*,#8840,.F.);
#11938=ORIENTED_EDGE('',*,*,#8342,.T.);
#11939=ORIENTED_EDGE('',*,*,#8575,.T.);
#11940=ORIENTED_EDGE('',*,*,#8344,.T.);
#11941=ORIENTED_EDGE('',*,*,#8841,.T.);
#11942=ORIENTED_EDGE('',*,*,#8771,.T.);
#11943=ORIENTED_EDGE('',*,*,#8772,.F.);
#11944=ORIENTED_EDGE('',*,*,#8841,.F.);
#11945=ORIENTED_EDGE('',*,*,#8343,.T.);
#11946=ORIENTED_EDGE('',*,*,#8840,.T.);
#11947=ORIENTED_EDGE('',*,*,#8574,.T.);
#11948=ORIENTED_EDGE('',*,*,#8770,.F.);
#11949=ORIENTED_EDGE('',*,*,#8842,.F.);
#11950=ORIENTED_EDGE('',*,*,#8346,.T.);
#11951=ORIENTED_EDGE('',*,*,#8560,.T.);
#11952=ORIENTED_EDGE('',*,*,#8348,.T.);
#11953=ORIENTED_EDGE('',*,*,#8843,.T.);
#11954=ORIENTED_EDGE('',*,*,#8768,.T.);
#11955=ORIENTED_EDGE('',*,*,#8769,.F.);
#11956=ORIENTED_EDGE('',*,*,#8843,.F.);
#11957=ORIENTED_EDGE('',*,*,#8347,.T.);
#11958=ORIENTED_EDGE('',*,*,#8842,.T.);
#11959=ORIENTED_EDGE('',*,*,#8568,.T.);
#11960=ORIENTED_EDGE('',*,*,#8776,.F.);
#11961=ORIENTED_EDGE('',*,*,#8844,.F.);
#11962=ORIENTED_EDGE('',*,*,#8338,.T.);
#11963=ORIENTED_EDGE('',*,*,#8571,.T.);
#11964=ORIENTED_EDGE('',*,*,#8340,.T.);
#11965=ORIENTED_EDGE('',*,*,#8845,.T.);
#11966=ORIENTED_EDGE('',*,*,#8774,.T.);
#11967=ORIENTED_EDGE('',*,*,#8775,.F.);
#11968=ORIENTED_EDGE('',*,*,#8845,.F.);
#11969=ORIENTED_EDGE('',*,*,#8339,.T.);
#11970=ORIENTED_EDGE('',*,*,#8844,.T.);
#11971=ORIENTED_EDGE('',*,*,#8567,.T.);
#11972=ORIENTED_EDGE('',*,*,#8761,.F.);
#11973=ORIENTED_EDGE('',*,*,#8846,.F.);
#11974=ORIENTED_EDGE('',*,*,#8358,.T.);
#11975=ORIENTED_EDGE('',*,*,#8557,.T.);
#11976=ORIENTED_EDGE('',*,*,#8360,.T.);
#11977=ORIENTED_EDGE('',*,*,#8847,.T.);
#11978=ORIENTED_EDGE('',*,*,#8759,.T.);
#11979=ORIENTED_EDGE('',*,*,#8760,.F.);
#11980=ORIENTED_EDGE('',*,*,#8847,.F.);
#11981=ORIENTED_EDGE('',*,*,#8359,.T.);
#11982=ORIENTED_EDGE('',*,*,#8846,.T.);
#11983=ORIENTED_EDGE('',*,*,#8564,.T.);
#11984=ORIENTED_EDGE('',*,*,#8764,.F.);
#11985=ORIENTED_EDGE('',*,*,#8848,.F.);
#11986=ORIENTED_EDGE('',*,*,#8354,.T.);
#11987=ORIENTED_EDGE('',*,*,#8565,.T.);
#11988=ORIENTED_EDGE('',*,*,#8356,.T.);
#11989=ORIENTED_EDGE('',*,*,#8849,.T.);
#11990=ORIENTED_EDGE('',*,*,#8762,.T.);
#11991=ORIENTED_EDGE('',*,*,#8763,.F.);
#11992=ORIENTED_EDGE('',*,*,#8849,.F.);
#11993=ORIENTED_EDGE('',*,*,#8355,.T.);
#11994=ORIENTED_EDGE('',*,*,#8848,.T.);
#11995=ORIENTED_EDGE('',*,*,#8559,.T.);
#11996=ORIENTED_EDGE('',*,*,#8767,.F.);
#11997=ORIENTED_EDGE('',*,*,#8850,.F.);
#11998=ORIENTED_EDGE('',*,*,#8350,.T.);
#11999=ORIENTED_EDGE('',*,*,#8562,.T.);
#12000=ORIENTED_EDGE('',*,*,#8352,.T.);
#12001=ORIENTED_EDGE('',*,*,#8851,.T.);
#12002=ORIENTED_EDGE('',*,*,#8765,.T.);
#12003=ORIENTED_EDGE('',*,*,#8766,.F.);
#12004=ORIENTED_EDGE('',*,*,#8851,.F.);
#12005=ORIENTED_EDGE('',*,*,#8351,.T.);
#12006=ORIENTED_EDGE('',*,*,#8850,.T.);
#12007=ORIENTED_EDGE('',*,*,#8556,.T.);
#12008=ORIENTED_EDGE('',*,*,#8758,.F.);
#12009=ORIENTED_EDGE('',*,*,#8852,.F.);
#12010=ORIENTED_EDGE('',*,*,#8362,.T.);
#12011=ORIENTED_EDGE('',*,*,#8554,.T.);
#12012=ORIENTED_EDGE('',*,*,#8364,.T.);
#12013=ORIENTED_EDGE('',*,*,#8853,.T.);
#12014=ORIENTED_EDGE('',*,*,#8756,.T.);
#12015=ORIENTED_EDGE('',*,*,#8757,.F.);
#12016=ORIENTED_EDGE('',*,*,#8853,.F.);
#12017=ORIENTED_EDGE('',*,*,#8363,.T.);
#12018=ORIENTED_EDGE('',*,*,#8852,.T.);
#12019=ORIENTED_EDGE('',*,*,#8553,.T.);
#12020=ORIENTED_EDGE('',*,*,#8755,.F.);
#12021=ORIENTED_EDGE('',*,*,#8854,.F.);
#12022=ORIENTED_EDGE('',*,*,#8366,.T.);
#12023=ORIENTED_EDGE('',*,*,#8548,.T.);
#12024=ORIENTED_EDGE('',*,*,#8368,.T.);
#12025=ORIENTED_EDGE('',*,*,#8855,.T.);
#12026=ORIENTED_EDGE('',*,*,#8753,.T.);
#12027=ORIENTED_EDGE('',*,*,#8754,.F.);
#12028=ORIENTED_EDGE('',*,*,#8855,.F.);
#12029=ORIENTED_EDGE('',*,*,#8367,.T.);
#12030=ORIENTED_EDGE('',*,*,#8854,.T.);
#12031=ORIENTED_EDGE('',*,*,#8547,.T.);
#12032=ORIENTED_EDGE('',*,*,#8752,.F.);
#12033=ORIENTED_EDGE('',*,*,#8856,.F.);
#12034=ORIENTED_EDGE('',*,*,#8370,.T.);
#12035=ORIENTED_EDGE('',*,*,#8550,.T.);
#12036=ORIENTED_EDGE('',*,*,#8372,.T.);
#12037=ORIENTED_EDGE('',*,*,#8857,.T.);
#12038=ORIENTED_EDGE('',*,*,#8750,.T.);
#12039=ORIENTED_EDGE('',*,*,#8751,.F.);
#12040=ORIENTED_EDGE('',*,*,#8857,.F.);
#12041=ORIENTED_EDGE('',*,*,#8371,.T.);
#12042=ORIENTED_EDGE('',*,*,#8856,.T.);
#12043=ORIENTED_EDGE('',*,*,#8544,.T.);
#12044=ORIENTED_EDGE('',*,*,#8676,.F.);
#12045=ORIENTED_EDGE('',*,*,#8858,.F.);
#12046=ORIENTED_EDGE('',*,*,#8470,.T.);
#12047=ORIENTED_EDGE('',*,*,#8542,.T.);
#12048=ORIENTED_EDGE('',*,*,#8472,.T.);
#12049=ORIENTED_EDGE('',*,*,#8859,.T.);
#12050=ORIENTED_EDGE('',*,*,#8674,.T.);
#12051=ORIENTED_EDGE('',*,*,#8675,.F.);
#12052=ORIENTED_EDGE('',*,*,#8859,.F.);
#12053=ORIENTED_EDGE('',*,*,#8471,.T.);
#12054=ORIENTED_EDGE('',*,*,#8858,.T.);
#12055=ORIENTED_EDGE('',*,*,#8541,.T.);
#12056=ORIENTED_EDGE('',*,*,#8673,.F.);
#12057=ORIENTED_EDGE('',*,*,#8860,.F.);
#12058=ORIENTED_EDGE('',*,*,#8474,.T.);
#12059=ORIENTED_EDGE('',*,*,#8533,.T.);
#12060=ORIENTED_EDGE('',*,*,#8476,.T.);
#12061=ORIENTED_EDGE('',*,*,#8861,.T.);
#12062=ORIENTED_EDGE('',*,*,#8671,.T.);
#12063=ORIENTED_EDGE('',*,*,#8672,.F.);
#12064=ORIENTED_EDGE('',*,*,#8861,.F.);
#12065=ORIENTED_EDGE('',*,*,#8475,.T.);
#12066=ORIENTED_EDGE('',*,*,#8860,.T.);
#12067=ORIENTED_EDGE('',*,*,#8537,.T.);
#12068=ORIENTED_EDGE('',*,*,#8667,.F.);
#12069=ORIENTED_EDGE('',*,*,#8862,.F.);
#12070=ORIENTED_EDGE('',*,*,#8482,.T.);
#12071=ORIENTED_EDGE('',*,*,#8539,.T.);
#12072=ORIENTED_EDGE('',*,*,#8484,.T.);
#12073=ORIENTED_EDGE('',*,*,#8863,.T.);
#12074=ORIENTED_EDGE('',*,*,#8665,.T.);
#12075=ORIENTED_EDGE('',*,*,#8666,.F.);
#12076=ORIENTED_EDGE('',*,*,#8863,.F.);
#12077=ORIENTED_EDGE('',*,*,#8483,.T.);
#12078=ORIENTED_EDGE('',*,*,#8862,.T.);
#12079=ORIENTED_EDGE('',*,*,#8538,.T.);
#12080=ORIENTED_EDGE('',*,*,#8664,.F.);
#12081=ORIENTED_EDGE('',*,*,#8864,.F.);
#12082=ORIENTED_EDGE('',*,*,#8486,.T.);
#12083=ORIENTED_EDGE('',*,*,#8524,.T.);
#12084=ORIENTED_EDGE('',*,*,#8488,.T.);
#12085=ORIENTED_EDGE('',*,*,#8865,.T.);
#12086=ORIENTED_EDGE('',*,*,#8662,.T.);
#12087=ORIENTED_EDGE('',*,*,#8663,.F.);
#12088=ORIENTED_EDGE('',*,*,#8865,.F.);
#12089=ORIENTED_EDGE('',*,*,#8487,.T.);
#12090=ORIENTED_EDGE('',*,*,#8864,.T.);
#12091=ORIENTED_EDGE('',*,*,#8532,.T.);
#12092=ORIENTED_EDGE('',*,*,#8670,.F.);
#12093=ORIENTED_EDGE('',*,*,#8866,.F.);
#12094=ORIENTED_EDGE('',*,*,#8478,.T.);
#12095=ORIENTED_EDGE('',*,*,#8535,.T.);
#12096=ORIENTED_EDGE('',*,*,#8480,.T.);
#12097=ORIENTED_EDGE('',*,*,#8867,.T.);
#12098=ORIENTED_EDGE('',*,*,#8668,.T.);
#12099=ORIENTED_EDGE('',*,*,#8669,.F.);
#12100=ORIENTED_EDGE('',*,*,#8867,.F.);
#12101=ORIENTED_EDGE('',*,*,#8479,.T.);
#12102=ORIENTED_EDGE('',*,*,#8866,.T.);
#12103=ORIENTED_EDGE('',*,*,#8531,.T.);
#12104=ORIENTED_EDGE('',*,*,#8655,.F.);
#12105=ORIENTED_EDGE('',*,*,#8868,.F.);
#12106=ORIENTED_EDGE('',*,*,#8498,.T.);
#12107=ORIENTED_EDGE('',*,*,#8521,.T.);
#12108=ORIENTED_EDGE('',*,*,#8500,.T.);
#12109=ORIENTED_EDGE('',*,*,#8869,.T.);
#12110=ORIENTED_EDGE('',*,*,#8653,.T.);
#12111=ORIENTED_EDGE('',*,*,#8654,.F.);
#12112=ORIENTED_EDGE('',*,*,#8869,.F.);
#12113=ORIENTED_EDGE('',*,*,#8499,.T.);
#12114=ORIENTED_EDGE('',*,*,#8868,.T.);
#12115=ORIENTED_EDGE('',*,*,#8528,.T.);
#12116=ORIENTED_EDGE('',*,*,#8658,.F.);
#12117=ORIENTED_EDGE('',*,*,#8870,.F.);
#12118=ORIENTED_EDGE('',*,*,#8494,.T.);
#12119=ORIENTED_EDGE('',*,*,#8529,.T.);
#12120=ORIENTED_EDGE('',*,*,#8496,.T.);
#12121=ORIENTED_EDGE('',*,*,#8871,.T.);
#12122=ORIENTED_EDGE('',*,*,#8656,.T.);
#12123=ORIENTED_EDGE('',*,*,#8657,.F.);
#12124=ORIENTED_EDGE('',*,*,#8871,.F.);
#12125=ORIENTED_EDGE('',*,*,#8495,.T.);
#12126=ORIENTED_EDGE('',*,*,#8870,.T.);
#12127=ORIENTED_EDGE('',*,*,#8523,.T.);
#12128=ORIENTED_EDGE('',*,*,#8661,.F.);
#12129=ORIENTED_EDGE('',*,*,#8872,.F.);
#12130=ORIENTED_EDGE('',*,*,#8490,.T.);
#12131=ORIENTED_EDGE('',*,*,#8526,.T.);
#12132=ORIENTED_EDGE('',*,*,#8492,.T.);
#12133=ORIENTED_EDGE('',*,*,#8873,.T.);
#12134=ORIENTED_EDGE('',*,*,#8659,.T.);
#12135=ORIENTED_EDGE('',*,*,#8660,.F.);
#12136=ORIENTED_EDGE('',*,*,#8873,.F.);
#12137=ORIENTED_EDGE('',*,*,#8491,.T.);
#12138=ORIENTED_EDGE('',*,*,#8872,.T.);
#12139=ORIENTED_EDGE('',*,*,#8520,.T.);
#12140=ORIENTED_EDGE('',*,*,#8652,.F.);
#12141=ORIENTED_EDGE('',*,*,#8874,.F.);
#12142=ORIENTED_EDGE('',*,*,#8502,.T.);
#12143=ORIENTED_EDGE('',*,*,#8518,.T.);
#12144=ORIENTED_EDGE('',*,*,#8504,.T.);
#12145=ORIENTED_EDGE('',*,*,#8875,.T.);
#12146=ORIENTED_EDGE('',*,*,#8650,.T.);
#12147=ORIENTED_EDGE('',*,*,#8651,.F.);
#12148=ORIENTED_EDGE('',*,*,#8875,.F.);
#12149=ORIENTED_EDGE('',*,*,#8503,.T.);
#12150=ORIENTED_EDGE('',*,*,#8874,.T.);
#12151=ORIENTED_EDGE('',*,*,#8517,.T.);
#12152=ORIENTED_EDGE('',*,*,#8649,.F.);
#12153=ORIENTED_EDGE('',*,*,#8876,.F.);
#12154=ORIENTED_EDGE('',*,*,#8506,.T.);
#12155=ORIENTED_EDGE('',*,*,#8512,.T.);
#12156=ORIENTED_EDGE('',*,*,#8508,.T.);
#12157=ORIENTED_EDGE('',*,*,#8877,.T.);
#12158=ORIENTED_EDGE('',*,*,#8647,.T.);
#12159=ORIENTED_EDGE('',*,*,#8648,.F.);
#12160=ORIENTED_EDGE('',*,*,#8877,.F.);
#12161=ORIENTED_EDGE('',*,*,#8507,.T.);
#12162=ORIENTED_EDGE('',*,*,#8876,.T.);
#12163=ORIENTED_EDGE('',*,*,#8511,.T.);
#12164=ORIENTED_EDGE('',*,*,#8646,.F.);
#12165=ORIENTED_EDGE('',*,*,#8878,.F.);
#12166=ORIENTED_EDGE('',*,*,#8326,.T.);
#12167=ORIENTED_EDGE('',*,*,#8514,.T.);
#12168=ORIENTED_EDGE('',*,*,#8328,.T.);
#12169=ORIENTED_EDGE('',*,*,#8879,.T.);
#12170=ORIENTED_EDGE('',*,*,#8783,.T.);
#12171=ORIENTED_EDGE('',*,*,#8784,.F.);
#12172=ORIENTED_EDGE('',*,*,#8879,.F.);
#12173=ORIENTED_EDGE('',*,*,#8327,.T.);
#12174=ORIENTED_EDGE('',*,*,#8878,.T.);
#12175=ORIENTED_EDGE('',*,*,#8510,.T.);
#12176=ORIENTED_EDGE('',*,*,#8880,.T.);
#12177=ORIENTED_EDGE('',*,*,#8785,.T.);
#12178=ORIENTED_EDGE('',*,*,#8880,.F.);
#12179=ORIENTED_EDGE('',*,*,#8881,.F.);
#12180=ORIENTED_EDGE('',*,*,#8882,.F.);
#12181=ORIENTED_EDGE('',*,*,#8883,.T.);
#12182=ORIENTED_EDGE('',*,*,#8884,.F.);
#12183=ORIENTED_EDGE('',*,*,#8885,.F.);
#12184=ORIENTED_EDGE('',*,*,#8886,.F.);
#12185=ORIENTED_EDGE('',*,*,#8884,.T.);
#12186=ORIENTED_EDGE('',*,*,#8887,.T.);
#12187=ORIENTED_EDGE('',*,*,#8888,.T.);
#12188=ORIENTED_EDGE('',*,*,#8889,.T.);
#12189=ORIENTED_EDGE('',*,*,#8890,.T.);
#12190=ORIENTED_EDGE('',*,*,#8891,.T.);
#12191=ORIENTED_EDGE('',*,*,#8892,.T.);
#12192=ORIENTED_EDGE('',*,*,#8893,.T.);
#12193=ORIENTED_EDGE('',*,*,#8894,.T.);
#12194=ORIENTED_EDGE('',*,*,#8895,.T.);
#12195=ORIENTED_EDGE('',*,*,#8896,.T.);
#12196=ORIENTED_EDGE('',*,*,#8894,.F.);
#12197=ORIENTED_EDGE('',*,*,#8897,.T.);
#12198=ORIENTED_EDGE('',*,*,#8898,.T.);
#12199=ORIENTED_EDGE('',*,*,#8899,.T.);
#12200=ORIENTED_EDGE('',*,*,#8900,.T.);
#12201=ORIENTED_EDGE('',*,*,#8898,.F.);
#12202=ORIENTED_EDGE('',*,*,#8901,.T.);
#12203=ORIENTED_EDGE('',*,*,#8902,.T.);
#12204=ORIENTED_EDGE('',*,*,#8903,.T.);
#12205=ORIENTED_EDGE('',*,*,#8904,.T.);
#12206=ORIENTED_EDGE('',*,*,#8905,.T.);
#12207=ORIENTED_EDGE('',*,*,#8903,.F.);
#12208=ORIENTED_EDGE('',*,*,#8906,.T.);
#12209=ORIENTED_EDGE('',*,*,#8907,.T.);
#12210=ORIENTED_EDGE('',*,*,#8908,.T.);
#12211=ORIENTED_EDGE('',*,*,#8909,.T.);
#12212=ORIENTED_EDGE('',*,*,#8907,.F.);
#12213=ORIENTED_EDGE('',*,*,#8910,.T.);
#12214=ORIENTED_EDGE('',*,*,#8911,.T.);
#12215=ORIENTED_EDGE('',*,*,#8912,.T.);
#12216=ORIENTED_EDGE('',*,*,#8897,.F.);
#12217=ORIENTED_EDGE('',*,*,#8913,.F.);
#12218=ORIENTED_EDGE('',*,*,#8914,.F.);
#12219=ORIENTED_EDGE('',*,*,#8915,.T.);
#12220=ORIENTED_EDGE('',*,*,#8916,.T.);
#12221=ORIENTED_EDGE('',*,*,#8915,.F.);
#12222=ORIENTED_EDGE('',*,*,#8917,.F.);
#12223=ORIENTED_EDGE('',*,*,#8918,.F.);
#12224=ORIENTED_EDGE('',*,*,#8919,.T.);
#12225=ORIENTED_EDGE('',*,*,#8920,.T.);
#12226=ORIENTED_EDGE('',*,*,#8919,.F.);
#12227=ORIENTED_EDGE('',*,*,#8921,.T.);
#12228=ORIENTED_EDGE('',*,*,#8922,.T.);
#12229=ORIENTED_EDGE('',*,*,#8923,.T.);
#12230=ORIENTED_EDGE('',*,*,#8924,.T.);
#12231=ORIENTED_EDGE('',*,*,#8922,.F.);
#12232=ORIENTED_EDGE('',*,*,#8925,.T.);
#12233=ORIENTED_EDGE('',*,*,#8926,.T.);
#12234=ORIENTED_EDGE('',*,*,#8927,.T.);
#12235=ORIENTED_EDGE('',*,*,#8928,.T.);
#12236=ORIENTED_EDGE('',*,*,#8926,.F.);
#12237=ORIENTED_EDGE('',*,*,#8929,.F.);
#12238=ORIENTED_EDGE('',*,*,#8930,.F.);
#12239=ORIENTED_EDGE('',*,*,#8931,.T.);
#12240=ORIENTED_EDGE('',*,*,#8932,.T.);
#12241=ORIENTED_EDGE('',*,*,#8931,.F.);
#12242=ORIENTED_EDGE('',*,*,#8933,.F.);
#12243=ORIENTED_EDGE('',*,*,#8934,.F.);
#12244=ORIENTED_EDGE('',*,*,#8935,.T.);
#12245=ORIENTED_EDGE('',*,*,#8936,.T.);
#12246=ORIENTED_EDGE('',*,*,#8935,.F.);
#12247=ORIENTED_EDGE('',*,*,#8937,.T.);
#12248=ORIENTED_EDGE('',*,*,#8938,.T.);
#12249=ORIENTED_EDGE('',*,*,#8939,.T.);
#12250=ORIENTED_EDGE('',*,*,#8940,.T.);
#12251=ORIENTED_EDGE('',*,*,#8938,.F.);
#12252=ORIENTED_EDGE('',*,*,#8941,.F.);
#12253=ORIENTED_EDGE('',*,*,#8942,.F.);
#12254=ORIENTED_EDGE('',*,*,#8943,.T.);
#12255=ORIENTED_EDGE('',*,*,#8944,.T.);
#12256=ORIENTED_EDGE('',*,*,#8943,.F.);
#12257=ORIENTED_EDGE('',*,*,#8945,.T.);
#12258=ORIENTED_EDGE('',*,*,#8946,.T.);
#12259=ORIENTED_EDGE('',*,*,#8947,.T.);
#12260=ORIENTED_EDGE('',*,*,#8948,.T.);
#12261=ORIENTED_EDGE('',*,*,#8946,.F.);
#12262=ORIENTED_EDGE('',*,*,#8949,.F.);
#12263=ORIENTED_EDGE('',*,*,#8950,.F.);
#12264=ORIENTED_EDGE('',*,*,#8951,.T.);
#12265=ORIENTED_EDGE('',*,*,#8952,.T.);
#12266=ORIENTED_EDGE('',*,*,#8951,.F.);
#12267=ORIENTED_EDGE('',*,*,#8953,.T.);
#12268=ORIENTED_EDGE('',*,*,#8954,.T.);
#12269=ORIENTED_EDGE('',*,*,#8955,.T.);
#12270=ORIENTED_EDGE('',*,*,#8956,.T.);
#12271=ORIENTED_EDGE('',*,*,#8954,.F.);
#12272=ORIENTED_EDGE('',*,*,#8957,.F.);
#12273=ORIENTED_EDGE('',*,*,#8958,.F.);
#12274=ORIENTED_EDGE('',*,*,#8959,.T.);
#12275=ORIENTED_EDGE('',*,*,#8960,.T.);
#12276=ORIENTED_EDGE('',*,*,#8959,.F.);
#12277=ORIENTED_EDGE('',*,*,#8961,.T.);
#12278=ORIENTED_EDGE('',*,*,#8962,.T.);
#12279=ORIENTED_EDGE('',*,*,#8963,.T.);
#12280=ORIENTED_EDGE('',*,*,#8964,.T.);
#12281=ORIENTED_EDGE('',*,*,#8962,.F.);
#12282=ORIENTED_EDGE('',*,*,#8886,.T.);
#12283=ORIENTED_EDGE('',*,*,#8965,.T.);
#12284=ORIENTED_EDGE('',*,*,#8966,.T.);
#12285=ORIENTED_EDGE('',*,*,#8887,.F.);
#12286=ORIENTED_EDGE('',*,*,#8967,.T.);
#12287=ORIENTED_EDGE('',*,*,#8885,.T.);
#12288=ORIENTED_EDGE('',*,*,#8968,.T.);
#12289=ORIENTED_EDGE('',*,*,#8882,.T.);
#12290=ORIENTED_EDGE('',*,*,#8969,.T.);
#12291=ORIENTED_EDGE('',*,*,#8970,.T.);
#12292=ORIENTED_EDGE('',*,*,#8971,.T.);
#12293=ORIENTED_EDGE('',*,*,#8972,.T.);
#12294=ORIENTED_EDGE('',*,*,#8973,.T.);
#12295=ORIENTED_EDGE('',*,*,#8974,.T.);
#12296=ORIENTED_EDGE('',*,*,#8975,.T.);
#12297=ORIENTED_EDGE('',*,*,#8976,.F.);
#12298=ORIENTED_EDGE('',*,*,#8889,.F.);
#12299=ORIENTED_EDGE('',*,*,#8977,.F.);
#12300=ORIENTED_EDGE('',*,*,#8975,.F.);
#12301=ORIENTED_EDGE('',*,*,#8977,.T.);
#12302=ORIENTED_EDGE('',*,*,#8888,.F.);
#12303=ORIENTED_EDGE('',*,*,#8966,.F.);
#12304=ORIENTED_EDGE('',*,*,#8978,.F.);
#12305=ORIENTED_EDGE('',*,*,#8972,.F.);
#12306=ORIENTED_EDGE('',*,*,#8976,.T.);
#12307=ORIENTED_EDGE('',*,*,#8974,.F.);
#12308=ORIENTED_EDGE('',*,*,#8979,.F.);
#12309=ORIENTED_EDGE('',*,*,#8890,.F.);
#12310=ORIENTED_EDGE('',*,*,#8978,.T.);
#12311=ORIENTED_EDGE('',*,*,#8965,.F.);
#12312=ORIENTED_EDGE('',*,*,#8891,.F.);
#12313=ORIENTED_EDGE('',*,*,#8979,.T.);
#12314=ORIENTED_EDGE('',*,*,#8973,.F.);
#12315=ORIENTED_EDGE('',*,*,#8970,.F.);
#12316=ORIENTED_EDGE('',*,*,#8980,.T.);
#12317=ORIENTED_EDGE('',*,*,#8899,.F.);
#12318=ORIENTED_EDGE('',*,*,#8900,.F.);
#12319=ORIENTED_EDGE('',*,*,#8980,.F.);
#12320=ORIENTED_EDGE('',*,*,#8892,.F.);
#12321=ORIENTED_EDGE('',*,*,#8893,.F.);
#12322=ORIENTED_EDGE('',*,*,#8981,.T.);
#12323=ORIENTED_EDGE('',*,*,#8971,.F.);
#12324=ORIENTED_EDGE('',*,*,#8981,.F.);
#12325=ORIENTED_EDGE('',*,*,#8911,.F.);
#12326=ORIENTED_EDGE('',*,*,#8982,.T.);
#12327=ORIENTED_EDGE('',*,*,#8895,.F.);
#12328=ORIENTED_EDGE('',*,*,#8896,.F.);
#12329=ORIENTED_EDGE('',*,*,#8982,.F.);
#12330=ORIENTED_EDGE('',*,*,#8901,.F.);
#12331=ORIENTED_EDGE('',*,*,#8902,.F.);
#12332=ORIENTED_EDGE('',*,*,#8983,.T.);
#12333=ORIENTED_EDGE('',*,*,#8910,.F.);
#12334=ORIENTED_EDGE('',*,*,#8983,.F.);
#12335=ORIENTED_EDGE('',*,*,#8917,.T.);
#12336=ORIENTED_EDGE('',*,*,#8918,.T.);
#12337=ORIENTED_EDGE('',*,*,#8984,.T.);
#12338=ORIENTED_EDGE('',*,*,#8904,.F.);
#12339=ORIENTED_EDGE('',*,*,#8905,.F.);
#12340=ORIENTED_EDGE('',*,*,#8984,.F.);
#12341=ORIENTED_EDGE('',*,*,#8933,.T.);
#12342=ORIENTED_EDGE('',*,*,#8934,.T.);
#12343=ORIENTED_EDGE('',*,*,#8985,.T.);
#12344=ORIENTED_EDGE('',*,*,#8927,.F.);
#12345=ORIENTED_EDGE('',*,*,#8928,.F.);
#12346=ORIENTED_EDGE('',*,*,#8985,.F.);
#12347=ORIENTED_EDGE('',*,*,#8920,.F.);
#12348=ORIENTED_EDGE('',*,*,#8986,.T.);
#12349=ORIENTED_EDGE('',*,*,#8925,.F.);
#12350=ORIENTED_EDGE('',*,*,#8986,.F.);
#12351=ORIENTED_EDGE('',*,*,#8957,.T.);
#12352=ORIENTED_EDGE('',*,*,#8958,.T.);
#12353=ORIENTED_EDGE('',*,*,#8987,.T.);
#12354=ORIENTED_EDGE('',*,*,#8963,.F.);
#12355=ORIENTED_EDGE('',*,*,#8964,.F.);
#12356=ORIENTED_EDGE('',*,*,#8987,.F.);
#12357=ORIENTED_EDGE('',*,*,#8936,.F.);
#12358=ORIENTED_EDGE('',*,*,#8988,.T.);
#12359=ORIENTED_EDGE('',*,*,#8961,.F.);
#12360=ORIENTED_EDGE('',*,*,#8988,.F.);
#12361=ORIENTED_EDGE('',*,*,#8949,.T.);
#12362=ORIENTED_EDGE('',*,*,#8950,.T.);
#12363=ORIENTED_EDGE('',*,*,#8989,.T.);
#12364=ORIENTED_EDGE('',*,*,#8955,.F.);
#12365=ORIENTED_EDGE('',*,*,#8956,.F.);
#12366=ORIENTED_EDGE('',*,*,#8989,.F.);
#12367=ORIENTED_EDGE('',*,*,#8960,.F.);
#12368=ORIENTED_EDGE('',*,*,#8990,.T.);
#12369=ORIENTED_EDGE('',*,*,#8953,.F.);
#12370=ORIENTED_EDGE('',*,*,#8990,.F.);
#12371=ORIENTED_EDGE('',*,*,#8952,.F.);
#12372=ORIENTED_EDGE('',*,*,#8991,.T.);
#12373=ORIENTED_EDGE('',*,*,#8945,.F.);
#12374=ORIENTED_EDGE('',*,*,#8991,.F.);
#12375=ORIENTED_EDGE('',*,*,#8941,.T.);
#12376=ORIENTED_EDGE('',*,*,#8942,.T.);
#12377=ORIENTED_EDGE('',*,*,#8992,.T.);
#12378=ORIENTED_EDGE('',*,*,#8947,.F.);
#12379=ORIENTED_EDGE('',*,*,#8948,.F.);
#12380=ORIENTED_EDGE('',*,*,#8992,.F.);
#12381=ORIENTED_EDGE('',*,*,#8944,.F.);
#12382=ORIENTED_EDGE('',*,*,#8993,.T.);
#12383=ORIENTED_EDGE('',*,*,#8937,.F.);
#12384=ORIENTED_EDGE('',*,*,#8993,.F.);
#12385=ORIENTED_EDGE('',*,*,#8929,.T.);
#12386=ORIENTED_EDGE('',*,*,#8930,.T.);
#12387=ORIENTED_EDGE('',*,*,#8994,.T.);
#12388=ORIENTED_EDGE('',*,*,#8939,.F.);
#12389=ORIENTED_EDGE('',*,*,#8940,.F.);
#12390=ORIENTED_EDGE('',*,*,#8994,.F.);
#12391=ORIENTED_EDGE('',*,*,#8912,.F.);
#12392=ORIENTED_EDGE('',*,*,#8995,.T.);
#12393=ORIENTED_EDGE('',*,*,#8908,.F.);
#12394=ORIENTED_EDGE('',*,*,#8909,.F.);
#12395=ORIENTED_EDGE('',*,*,#8995,.F.);
#12396=ORIENTED_EDGE('',*,*,#8916,.F.);
#12397=ORIENTED_EDGE('',*,*,#8996,.T.);
#12398=ORIENTED_EDGE('',*,*,#8906,.F.);
#12399=ORIENTED_EDGE('',*,*,#8996,.F.);
#12400=ORIENTED_EDGE('',*,*,#8913,.T.);
#12401=ORIENTED_EDGE('',*,*,#8914,.T.);
#12402=ORIENTED_EDGE('',*,*,#8997,.T.);
#12403=ORIENTED_EDGE('',*,*,#8923,.F.);
#12404=ORIENTED_EDGE('',*,*,#8924,.F.);
#12405=ORIENTED_EDGE('',*,*,#8997,.F.);
#12406=ORIENTED_EDGE('',*,*,#8932,.F.);
#12407=ORIENTED_EDGE('',*,*,#8998,.T.);
#12408=ORIENTED_EDGE('',*,*,#8921,.F.);
#12409=ORIENTED_EDGE('',*,*,#8998,.F.);
#12410=ORIENTED_EDGE('',*,*,#8881,.T.);
#12411=ORIENTED_EDGE('',*,*,#8967,.F.);
#12412=ORIENTED_EDGE('',*,*,#8883,.F.);
#12413=ORIENTED_EDGE('',*,*,#8968,.F.);
#12414=ORIENTED_EDGE('',*,*,#8969,.F.);
#12415=ORIENTED_EDGE('',*,*,#8999,.F.);
#12416=ORIENTED_EDGE('',*,*,#8999,.T.);
#12417=ORIENTED_EDGE('',*,*,#9000,.F.);
#12418=ORIENTED_EDGE('',*,*,#9001,.T.);
#12419=ORIENTED_EDGE('',*,*,#9002,.T.);
#12420=ORIENTED_EDGE('',*,*,#9003,.T.);
#12421=ORIENTED_EDGE('',*,*,#9004,.T.);
#12422=ORIENTED_EDGE('',*,*,#9005,.T.);
#12423=ORIENTED_EDGE('',*,*,#9006,.T.);
#12424=ORIENTED_EDGE('',*,*,#9007,.F.);
#12425=ORIENTED_EDGE('',*,*,#9008,.T.);
#12426=ORIENTED_EDGE('',*,*,#9009,.T.);
#12427=ORIENTED_EDGE('',*,*,#9010,.T.);
#12428=ORIENTED_EDGE('',*,*,#9011,.T.);
#12429=ORIENTED_EDGE('',*,*,#9012,.T.);
#12430=ORIENTED_EDGE('',*,*,#9013,.T.);
#12431=ORIENTED_EDGE('',*,*,#9014,.T.);
#12432=ORIENTED_EDGE('',*,*,#9015,.T.);
#12433=ORIENTED_EDGE('',*,*,#9016,.T.);
#12434=ORIENTED_EDGE('',*,*,#9017,.T.);
#12435=ORIENTED_EDGE('',*,*,#9018,.T.);
#12436=ORIENTED_EDGE('',*,*,#9019,.T.);
#12437=ORIENTED_EDGE('',*,*,#9020,.T.);
#12438=ORIENTED_EDGE('',*,*,#9021,.F.);
#12439=ORIENTED_EDGE('',*,*,#9022,.T.);
#12440=ORIENTED_EDGE('',*,*,#9023,.T.);
#12441=ORIENTED_EDGE('',*,*,#9024,.T.);
#12442=ORIENTED_EDGE('',*,*,#9025,.T.);
#12443=ORIENTED_EDGE('',*,*,#9026,.T.);
#12444=ORIENTED_EDGE('',*,*,#9027,.T.);
#12445=ORIENTED_EDGE('',*,*,#9028,.T.);
#12446=ORIENTED_EDGE('',*,*,#9029,.T.);
#12447=ORIENTED_EDGE('',*,*,#9030,.T.);
#12448=ORIENTED_EDGE('',*,*,#9031,.T.);
#12449=ORIENTED_EDGE('',*,*,#9032,.T.);
#12450=ORIENTED_EDGE('',*,*,#9033,.T.);
#12451=ORIENTED_EDGE('',*,*,#9034,.T.);
#12452=ORIENTED_EDGE('',*,*,#9035,.T.);
#12453=ORIENTED_EDGE('',*,*,#9036,.T.);
#12454=ORIENTED_EDGE('',*,*,#9037,.T.);
#12455=ORIENTED_EDGE('',*,*,#9038,.T.);
#12456=ORIENTED_EDGE('',*,*,#9039,.T.);
#12457=ORIENTED_EDGE('',*,*,#9040,.T.);
#12458=ORIENTED_EDGE('',*,*,#9041,.T.);
#12459=ORIENTED_EDGE('',*,*,#9042,.T.);
#12460=ORIENTED_EDGE('',*,*,#9043,.T.);
#12461=ORIENTED_EDGE('',*,*,#9044,.T.);
#12462=ORIENTED_EDGE('',*,*,#9045,.T.);
#12463=ORIENTED_EDGE('',*,*,#9046,.T.);
#12464=ORIENTED_EDGE('',*,*,#9047,.T.);
#12465=ORIENTED_EDGE('',*,*,#9048,.T.);
#12466=ORIENTED_EDGE('',*,*,#9049,.T.);
#12467=ORIENTED_EDGE('',*,*,#9050,.T.);
#12468=ORIENTED_EDGE('',*,*,#9051,.T.);
#12469=ORIENTED_EDGE('',*,*,#9052,.T.);
#12470=ORIENTED_EDGE('',*,*,#9053,.T.);
#12471=ORIENTED_EDGE('',*,*,#9054,.T.);
#12472=ORIENTED_EDGE('',*,*,#9055,.T.);
#12473=ORIENTED_EDGE('',*,*,#9056,.T.);
#12474=ORIENTED_EDGE('',*,*,#9057,.T.);
#12475=ORIENTED_EDGE('',*,*,#9058,.T.);
#12476=ORIENTED_EDGE('',*,*,#9059,.T.);
#12477=ORIENTED_EDGE('',*,*,#9060,.T.);
#12478=ORIENTED_EDGE('',*,*,#9061,.T.);
#12479=ORIENTED_EDGE('',*,*,#9062,.T.);
#12480=ORIENTED_EDGE('',*,*,#9063,.T.);
#12481=ORIENTED_EDGE('',*,*,#9064,.T.);
#12482=ORIENTED_EDGE('',*,*,#9065,.T.);
#12483=ORIENTED_EDGE('',*,*,#9066,.T.);
#12484=ORIENTED_EDGE('',*,*,#9067,.T.);
#12485=ORIENTED_EDGE('',*,*,#9068,.T.);
#12486=ORIENTED_EDGE('',*,*,#9069,.T.);
#12487=ORIENTED_EDGE('',*,*,#9070,.T.);
#12488=ORIENTED_EDGE('',*,*,#9071,.T.);
#12489=ORIENTED_EDGE('',*,*,#9072,.T.);
#12490=ORIENTED_EDGE('',*,*,#9073,.T.);
#12491=ORIENTED_EDGE('',*,*,#9074,.T.);
#12492=ORIENTED_EDGE('',*,*,#9075,.T.);
#12493=ORIENTED_EDGE('',*,*,#9076,.T.);
#12494=ORIENTED_EDGE('',*,*,#9077,.T.);
#12495=ORIENTED_EDGE('',*,*,#9078,.T.);
#12496=ORIENTED_EDGE('',*,*,#9079,.T.);
#12497=ORIENTED_EDGE('',*,*,#9080,.T.);
#12498=ORIENTED_EDGE('',*,*,#9081,.T.);
#12499=ORIENTED_EDGE('',*,*,#9082,.T.);
#12500=ORIENTED_EDGE('',*,*,#9083,.T.);
#12501=ORIENTED_EDGE('',*,*,#9084,.T.);
#12502=ORIENTED_EDGE('',*,*,#9085,.T.);
#12503=ORIENTED_EDGE('',*,*,#9086,.T.);
#12504=ORIENTED_EDGE('',*,*,#9087,.T.);
#12505=ORIENTED_EDGE('',*,*,#9088,.T.);
#12506=ORIENTED_EDGE('',*,*,#9089,.T.);
#12507=ORIENTED_EDGE('',*,*,#9090,.T.);
#12508=ORIENTED_EDGE('',*,*,#9091,.T.);
#12509=ORIENTED_EDGE('',*,*,#9092,.T.);
#12510=ORIENTED_EDGE('',*,*,#9093,.T.);
#12511=ORIENTED_EDGE('',*,*,#9094,.T.);
#12512=ORIENTED_EDGE('',*,*,#9095,.T.);
#12513=ORIENTED_EDGE('',*,*,#9096,.T.);
#12514=ORIENTED_EDGE('',*,*,#9097,.T.);
#12515=ORIENTED_EDGE('',*,*,#9098,.T.);
#12516=ORIENTED_EDGE('',*,*,#9099,.T.);
#12517=ORIENTED_EDGE('',*,*,#9100,.T.);
#12518=ORIENTED_EDGE('',*,*,#9101,.T.);
#12519=ORIENTED_EDGE('',*,*,#9102,.T.);
#12520=ORIENTED_EDGE('',*,*,#9103,.T.);
#12521=ORIENTED_EDGE('',*,*,#9104,.T.);
#12522=ORIENTED_EDGE('',*,*,#9105,.T.);
#12523=ORIENTED_EDGE('',*,*,#9106,.T.);
#12524=ORIENTED_EDGE('',*,*,#9107,.T.);
#12525=ORIENTED_EDGE('',*,*,#9108,.T.);
#12526=ORIENTED_EDGE('',*,*,#9109,.T.);
#12527=ORIENTED_EDGE('',*,*,#9110,.T.);
#12528=ORIENTED_EDGE('',*,*,#9111,.T.);
#12529=ORIENTED_EDGE('',*,*,#9112,.T.);
#12530=ORIENTED_EDGE('',*,*,#9113,.T.);
#12531=ORIENTED_EDGE('',*,*,#9114,.T.);
#12532=ORIENTED_EDGE('',*,*,#9115,.T.);
#12533=ORIENTED_EDGE('',*,*,#9116,.T.);
#12534=ORIENTED_EDGE('',*,*,#9117,.T.);
#12535=ORIENTED_EDGE('',*,*,#9118,.T.);
#12536=ORIENTED_EDGE('',*,*,#9119,.T.);
#12537=ORIENTED_EDGE('',*,*,#9120,.T.);
#12538=ORIENTED_EDGE('',*,*,#9121,.T.);
#12539=ORIENTED_EDGE('',*,*,#9122,.T.);
#12540=ORIENTED_EDGE('',*,*,#9123,.T.);
#12541=ORIENTED_EDGE('',*,*,#9124,.T.);
#12542=ORIENTED_EDGE('',*,*,#9125,.T.);
#12543=ORIENTED_EDGE('',*,*,#9126,.T.);
#12544=ORIENTED_EDGE('',*,*,#9127,.T.);
#12545=ORIENTED_EDGE('',*,*,#9128,.T.);
#12546=ORIENTED_EDGE('',*,*,#9129,.T.);
#12547=ORIENTED_EDGE('',*,*,#9130,.T.);
#12548=ORIENTED_EDGE('',*,*,#9131,.T.);
#12549=ORIENTED_EDGE('',*,*,#9132,.T.);
#12550=ORIENTED_EDGE('',*,*,#9133,.T.);
#12551=ORIENTED_EDGE('',*,*,#9134,.T.);
#12552=ORIENTED_EDGE('',*,*,#9135,.T.);
#12553=ORIENTED_EDGE('',*,*,#9136,.T.);
#12554=ORIENTED_EDGE('',*,*,#9137,.T.);
#12555=ORIENTED_EDGE('',*,*,#9138,.T.);
#12556=ORIENTED_EDGE('',*,*,#9139,.T.);
#12557=ORIENTED_EDGE('',*,*,#9140,.T.);
#12558=ORIENTED_EDGE('',*,*,#9141,.T.);
#12559=ORIENTED_EDGE('',*,*,#9142,.T.);
#12560=ORIENTED_EDGE('',*,*,#9143,.T.);
#12561=ORIENTED_EDGE('',*,*,#9144,.T.);
#12562=ORIENTED_EDGE('',*,*,#9145,.T.);
#12563=ORIENTED_EDGE('',*,*,#9146,.T.);
#12564=ORIENTED_EDGE('',*,*,#9147,.T.);
#12565=ORIENTED_EDGE('',*,*,#9148,.T.);
#12566=ORIENTED_EDGE('',*,*,#9149,.T.);
#12567=ORIENTED_EDGE('',*,*,#9150,.T.);
#12568=ORIENTED_EDGE('',*,*,#9151,.T.);
#12569=ORIENTED_EDGE('',*,*,#9152,.T.);
#12570=ORIENTED_EDGE('',*,*,#9153,.T.);
#12571=ORIENTED_EDGE('',*,*,#9154,.T.);
#12572=ORIENTED_EDGE('',*,*,#9155,.T.);
#12573=ORIENTED_EDGE('',*,*,#9156,.T.);
#12574=ORIENTED_EDGE('',*,*,#9157,.T.);
#12575=ORIENTED_EDGE('',*,*,#9158,.T.);
#12576=ORIENTED_EDGE('',*,*,#9159,.T.);
#12577=ORIENTED_EDGE('',*,*,#9160,.F.);
#12578=ORIENTED_EDGE('',*,*,#9161,.F.);
#12579=ORIENTED_EDGE('',*,*,#9162,.T.);
#12580=ORIENTED_EDGE('',*,*,#9163,.T.);
#12581=ORIENTED_EDGE('',*,*,#9164,.F.);
#12582=ORIENTED_EDGE('',*,*,#9165,.T.);
#12583=ORIENTED_EDGE('',*,*,#9166,.F.);
#12584=ORIENTED_EDGE('',*,*,#9167,.T.);
#12585=ORIENTED_EDGE('',*,*,#9168,.T.);
#12586=ORIENTED_EDGE('',*,*,#9169,.T.);
#12587=ORIENTED_EDGE('',*,*,#9170,.T.);
#12588=ORIENTED_EDGE('',*,*,#9171,.F.);
#12589=ORIENTED_EDGE('',*,*,#9172,.F.);
#12590=ORIENTED_EDGE('',*,*,#9173,.T.);
#12591=ORIENTED_EDGE('',*,*,#9174,.T.);
#12592=ORIENTED_EDGE('',*,*,#9175,.T.);
#12593=ORIENTED_EDGE('',*,*,#9176,.F.);
#12594=ORIENTED_EDGE('',*,*,#9177,.F.);
#12595=ORIENTED_EDGE('',*,*,#9178,.T.);
#12596=ORIENTED_EDGE('',*,*,#9179,.T.);
#12597=ORIENTED_EDGE('',*,*,#9180,.F.);
#12598=ORIENTED_EDGE('',*,*,#9181,.F.);
#12599=ORIENTED_EDGE('',*,*,#9182,.F.);
#12600=ORIENTED_EDGE('',*,*,#9183,.F.);
#12601=ORIENTED_EDGE('',*,*,#9184,.F.);
#12602=ORIENTED_EDGE('',*,*,#9185,.F.);
#12603=ORIENTED_EDGE('',*,*,#9186,.F.);
#12604=ORIENTED_EDGE('',*,*,#9187,.F.);
#12605=ORIENTED_EDGE('',*,*,#9188,.F.);
#12606=ORIENTED_EDGE('',*,*,#9189,.T.);
#12607=ORIENTED_EDGE('',*,*,#9190,.T.);
#12608=ORIENTED_EDGE('',*,*,#9191,.F.);
#12609=ORIENTED_EDGE('',*,*,#9192,.F.);
#12610=ORIENTED_EDGE('',*,*,#9193,.F.);
#12611=ORIENTED_EDGE('',*,*,#9194,.T.);
#12612=ORIENTED_EDGE('',*,*,#9195,.T.);
#12613=ORIENTED_EDGE('',*,*,#9196,.F.);
#12614=ORIENTED_EDGE('',*,*,#9197,.T.);
#12615=ORIENTED_EDGE('',*,*,#9198,.F.);
#12616=ORIENTED_EDGE('',*,*,#9199,.F.);
#12617=ORIENTED_EDGE('',*,*,#9200,.F.);
#12618=ORIENTED_EDGE('',*,*,#9201,.T.);
#12619=ORIENTED_EDGE('',*,*,#9202,.T.);
#12620=ORIENTED_EDGE('',*,*,#9203,.F.);
#12621=ORIENTED_EDGE('',*,*,#9204,.T.);
#12622=ORIENTED_EDGE('',*,*,#9160,.T.);
#12623=ORIENTED_EDGE('',*,*,#9205,.F.);
#12624=ORIENTED_EDGE('',*,*,#9206,.F.);
#12625=ORIENTED_EDGE('',*,*,#9165,.F.);
#12626=ORIENTED_EDGE('',*,*,#9207,.F.);
#12627=ORIENTED_EDGE('',*,*,#9208,.F.);
#12628=ORIENTED_EDGE('',*,*,#9209,.F.);
#12629=ORIENTED_EDGE('',*,*,#9210,.F.);
#12630=ORIENTED_EDGE('',*,*,#9211,.F.);
#12631=ORIENTED_EDGE('',*,*,#9212,.F.);
#12632=ORIENTED_EDGE('',*,*,#9021,.T.);
#12633=ORIENTED_EDGE('',*,*,#9213,.T.);
#12634=ORIENTED_EDGE('',*,*,#9214,.T.);
#12635=ORIENTED_EDGE('',*,*,#9215,.T.);
#12636=ORIENTED_EDGE('',*,*,#9216,.T.);
#12637=ORIENTED_EDGE('',*,*,#9217,.T.);
#12638=ORIENTED_EDGE('',*,*,#9218,.T.);
#12639=ORIENTED_EDGE('',*,*,#9219,.T.);
#12640=ORIENTED_EDGE('',*,*,#9220,.T.);
#12641=ORIENTED_EDGE('',*,*,#9221,.T.);
#12642=ORIENTED_EDGE('',*,*,#9222,.T.);
#12643=ORIENTED_EDGE('',*,*,#9223,.T.);
#12644=ORIENTED_EDGE('',*,*,#9224,.T.);
#12645=ORIENTED_EDGE('',*,*,#9151,.F.);
#12646=ORIENTED_EDGE('',*,*,#9225,.T.);
#12647=ORIENTED_EDGE('',*,*,#9226,.T.);
#12648=ORIENTED_EDGE('',*,*,#9227,.T.);
#12649=ORIENTED_EDGE('',*,*,#9228,.T.);
#12650=ORIENTED_EDGE('',*,*,#9229,.T.);
#12651=ORIENTED_EDGE('',*,*,#9230,.T.);
#12652=ORIENTED_EDGE('',*,*,#9143,.F.);
#12653=ORIENTED_EDGE('',*,*,#9231,.T.);
#12654=ORIENTED_EDGE('',*,*,#9232,.T.);
#12655=ORIENTED_EDGE('',*,*,#9233,.T.);
#12656=ORIENTED_EDGE('',*,*,#9137,.F.);
#12657=ORIENTED_EDGE('',*,*,#9234,.T.);
#12658=ORIENTED_EDGE('',*,*,#9235,.T.);
#12659=ORIENTED_EDGE('',*,*,#9236,.T.);
#12660=ORIENTED_EDGE('',*,*,#9131,.F.);
#12661=ORIENTED_EDGE('',*,*,#9237,.T.);
#12662=ORIENTED_EDGE('',*,*,#9238,.T.);
#12663=ORIENTED_EDGE('',*,*,#9239,.T.);
#12664=ORIENTED_EDGE('',*,*,#9125,.F.);
#12665=ORIENTED_EDGE('',*,*,#9240,.T.);
#12666=ORIENTED_EDGE('',*,*,#9241,.T.);
#12667=ORIENTED_EDGE('',*,*,#9242,.T.);
#12668=ORIENTED_EDGE('',*,*,#9119,.F.);
#12669=ORIENTED_EDGE('',*,*,#9243,.T.);
#12670=ORIENTED_EDGE('',*,*,#9244,.T.);
#12671=ORIENTED_EDGE('',*,*,#9245,.T.);
#12672=ORIENTED_EDGE('',*,*,#9113,.F.);
#12673=ORIENTED_EDGE('',*,*,#9246,.T.);
#12674=ORIENTED_EDGE('',*,*,#9247,.T.);
#12675=ORIENTED_EDGE('',*,*,#9248,.T.);
#12676=ORIENTED_EDGE('',*,*,#9107,.F.);
#12677=ORIENTED_EDGE('',*,*,#9249,.T.);
#12678=ORIENTED_EDGE('',*,*,#9250,.T.);
#12679=ORIENTED_EDGE('',*,*,#9251,.T.);
#12680=ORIENTED_EDGE('',*,*,#9101,.F.);
#12681=ORIENTED_EDGE('',*,*,#9252,.T.);
#12682=ORIENTED_EDGE('',*,*,#9253,.T.);
#12683=ORIENTED_EDGE('',*,*,#9254,.T.);
#12684=ORIENTED_EDGE('',*,*,#9095,.F.);
#12685=ORIENTED_EDGE('',*,*,#9255,.T.);
#12686=ORIENTED_EDGE('',*,*,#9256,.T.);
#12687=ORIENTED_EDGE('',*,*,#9257,.T.);
#12688=ORIENTED_EDGE('',*,*,#9089,.F.);
#12689=ORIENTED_EDGE('',*,*,#9258,.T.);
#12690=ORIENTED_EDGE('',*,*,#9259,.T.);
#12691=ORIENTED_EDGE('',*,*,#9260,.T.);
#12692=ORIENTED_EDGE('',*,*,#9083,.F.);
#12693=ORIENTED_EDGE('',*,*,#9261,.T.);
#12694=ORIENTED_EDGE('',*,*,#9262,.T.);
#12695=ORIENTED_EDGE('',*,*,#9263,.T.);
#12696=ORIENTED_EDGE('',*,*,#9077,.F.);
#12697=ORIENTED_EDGE('',*,*,#9264,.T.);
#12698=ORIENTED_EDGE('',*,*,#9265,.T.);
#12699=ORIENTED_EDGE('',*,*,#9266,.T.);
#12700=ORIENTED_EDGE('',*,*,#9267,.T.);
#12701=ORIENTED_EDGE('',*,*,#9070,.F.);
#12702=ORIENTED_EDGE('',*,*,#9268,.T.);
#12703=ORIENTED_EDGE('',*,*,#9269,.T.);
#12704=ORIENTED_EDGE('',*,*,#9270,.T.);
#12705=ORIENTED_EDGE('',*,*,#9271,.T.);
#12706=ORIENTED_EDGE('',*,*,#9272,.T.);
#12707=ORIENTED_EDGE('',*,*,#9059,.F.);
#12708=ORIENTED_EDGE('',*,*,#9273,.T.);
#12709=ORIENTED_EDGE('',*,*,#9274,.T.);
#12710=ORIENTED_EDGE('',*,*,#9275,.T.);
#12711=ORIENTED_EDGE('',*,*,#9276,.T.);
#12712=ORIENTED_EDGE('',*,*,#9277,.T.);
#12713=ORIENTED_EDGE('',*,*,#9051,.F.);
#12714=ORIENTED_EDGE('',*,*,#9278,.T.);
#12715=ORIENTED_EDGE('',*,*,#9279,.T.);
#12716=ORIENTED_EDGE('',*,*,#9280,.T.);
#12717=ORIENTED_EDGE('',*,*,#9281,.T.);
#12718=ORIENTED_EDGE('',*,*,#9282,.T.);
#12719=ORIENTED_EDGE('',*,*,#9043,.F.);
#12720=ORIENTED_EDGE('',*,*,#9283,.T.);
#12721=ORIENTED_EDGE('',*,*,#9284,.T.);
#12722=ORIENTED_EDGE('',*,*,#9285,.T.);
#12723=ORIENTED_EDGE('',*,*,#9286,.T.);
#12724=ORIENTED_EDGE('',*,*,#9287,.T.);
#12725=ORIENTED_EDGE('',*,*,#9035,.F.);
#12726=ORIENTED_EDGE('',*,*,#9288,.T.);
#12727=ORIENTED_EDGE('',*,*,#9289,.T.);
#12728=ORIENTED_EDGE('',*,*,#9290,.T.);
#12729=ORIENTED_EDGE('',*,*,#9291,.T.);
#12730=ORIENTED_EDGE('',*,*,#9292,.T.);
#12731=ORIENTED_EDGE('',*,*,#9293,.T.);
#12732=ORIENTED_EDGE('',*,*,#9294,.T.);
#12733=ORIENTED_EDGE('',*,*,#9295,.T.);
#12734=ORIENTED_EDGE('',*,*,#9296,.T.);
#12735=ORIENTED_EDGE('',*,*,#9297,.T.);
#12736=ORIENTED_EDGE('',*,*,#9298,.T.);
#12737=ORIENTED_EDGE('',*,*,#9299,.T.);
#12738=ORIENTED_EDGE('',*,*,#9300,.T.);
#12739=ORIENTED_EDGE('',*,*,#9301,.T.);
#12740=ORIENTED_EDGE('',*,*,#9302,.T.);
#12741=ORIENTED_EDGE('',*,*,#9303,.T.);
#12742=ORIENTED_EDGE('',*,*,#9304,.T.);
#12743=ORIENTED_EDGE('',*,*,#9305,.T.);
#12744=ORIENTED_EDGE('',*,*,#9306,.T.);
#12745=ORIENTED_EDGE('',*,*,#9307,.T.);
#12746=ORIENTED_EDGE('',*,*,#9308,.T.);
#12747=ORIENTED_EDGE('',*,*,#9309,.T.);
#12748=ORIENTED_EDGE('',*,*,#9310,.T.);
#12749=ORIENTED_EDGE('',*,*,#9311,.T.);
#12750=ORIENTED_EDGE('',*,*,#9312,.T.);
#12751=ORIENTED_EDGE('',*,*,#9313,.T.);
#12752=ORIENTED_EDGE('',*,*,#9314,.T.);
#12753=ORIENTED_EDGE('',*,*,#9315,.T.);
#12754=ORIENTED_EDGE('',*,*,#9316,.T.);
#12755=ORIENTED_EDGE('',*,*,#9317,.T.);
#12756=ORIENTED_EDGE('',*,*,#9318,.T.);
#12757=ORIENTED_EDGE('',*,*,#9319,.T.);
#12758=ORIENTED_EDGE('',*,*,#9320,.T.);
#12759=ORIENTED_EDGE('',*,*,#9321,.T.);
#12760=ORIENTED_EDGE('',*,*,#9322,.T.);
#12761=ORIENTED_EDGE('',*,*,#9323,.T.);
#12762=ORIENTED_EDGE('',*,*,#9324,.T.);
#12763=ORIENTED_EDGE('',*,*,#9325,.T.);
#12764=ORIENTED_EDGE('',*,*,#9326,.T.);
#12765=ORIENTED_EDGE('',*,*,#9327,.T.);
#12766=ORIENTED_EDGE('',*,*,#9328,.T.);
#12767=ORIENTED_EDGE('',*,*,#9329,.T.);
#12768=ORIENTED_EDGE('',*,*,#9330,.T.);
#12769=ORIENTED_EDGE('',*,*,#9331,.T.);
#12770=ORIENTED_EDGE('',*,*,#9332,.T.);
#12771=ORIENTED_EDGE('',*,*,#9333,.T.);
#12772=ORIENTED_EDGE('',*,*,#9334,.T.);
#12773=ORIENTED_EDGE('',*,*,#9335,.T.);
#12774=ORIENTED_EDGE('',*,*,#9336,.T.);
#12775=ORIENTED_EDGE('',*,*,#9337,.T.);
#12776=ORIENTED_EDGE('',*,*,#9338,.T.);
#12777=ORIENTED_EDGE('',*,*,#9339,.T.);
#12778=ORIENTED_EDGE('',*,*,#9340,.T.);
#12779=ORIENTED_EDGE('',*,*,#9341,.T.);
#12780=ORIENTED_EDGE('',*,*,#9342,.T.);
#12781=ORIENTED_EDGE('',*,*,#9343,.T.);
#12782=ORIENTED_EDGE('',*,*,#9344,.T.);
#12783=ORIENTED_EDGE('',*,*,#9345,.T.);
#12784=ORIENTED_EDGE('',*,*,#9346,.T.);
#12785=ORIENTED_EDGE('',*,*,#9347,.T.);
#12786=ORIENTED_EDGE('',*,*,#9348,.T.);
#12787=ORIENTED_EDGE('',*,*,#9349,.T.);
#12788=ORIENTED_EDGE('',*,*,#9350,.T.);
#12789=ORIENTED_EDGE('',*,*,#9351,.T.);
#12790=ORIENTED_EDGE('',*,*,#9352,.T.);
#12791=ORIENTED_EDGE('',*,*,#9353,.T.);
#12792=ORIENTED_EDGE('',*,*,#9354,.T.);
#12793=ORIENTED_EDGE('',*,*,#9355,.T.);
#12794=ORIENTED_EDGE('',*,*,#9356,.T.);
#12795=ORIENTED_EDGE('',*,*,#9357,.T.);
#12796=ORIENTED_EDGE('',*,*,#9358,.T.);
#12797=ORIENTED_EDGE('',*,*,#9359,.T.);
#12798=ORIENTED_EDGE('',*,*,#9360,.T.);
#12799=ORIENTED_EDGE('',*,*,#9361,.T.);
#12800=ORIENTED_EDGE('',*,*,#9362,.T.);
#12801=ORIENTED_EDGE('',*,*,#9363,.T.);
#12802=ORIENTED_EDGE('',*,*,#9364,.T.);
#12803=ORIENTED_EDGE('',*,*,#9365,.T.);
#12804=ORIENTED_EDGE('',*,*,#9366,.T.);
#12805=ORIENTED_EDGE('',*,*,#9367,.T.);
#12806=ORIENTED_EDGE('',*,*,#9368,.T.);
#12807=ORIENTED_EDGE('',*,*,#9369,.T.);
#12808=ORIENTED_EDGE('',*,*,#9370,.T.);
#12809=ORIENTED_EDGE('',*,*,#9371,.T.);
#12810=ORIENTED_EDGE('',*,*,#9372,.T.);
#12811=ORIENTED_EDGE('',*,*,#9373,.T.);
#12812=ORIENTED_EDGE('',*,*,#9374,.T.);
#12813=ORIENTED_EDGE('',*,*,#9375,.T.);
#12814=ORIENTED_EDGE('',*,*,#9376,.T.);
#12815=ORIENTED_EDGE('',*,*,#9377,.T.);
#12816=ORIENTED_EDGE('',*,*,#9378,.T.);
#12817=ORIENTED_EDGE('',*,*,#9379,.T.);
#12818=ORIENTED_EDGE('',*,*,#9380,.T.);
#12819=ORIENTED_EDGE('',*,*,#9381,.T.);
#12820=ORIENTED_EDGE('',*,*,#9382,.T.);
#12821=ORIENTED_EDGE('',*,*,#9383,.T.);
#12822=ORIENTED_EDGE('',*,*,#9384,.T.);
#12823=ORIENTED_EDGE('',*,*,#9385,.T.);
#12824=ORIENTED_EDGE('',*,*,#9386,.T.);
#12825=ORIENTED_EDGE('',*,*,#9387,.T.);
#12826=ORIENTED_EDGE('',*,*,#9388,.T.);
#12827=ORIENTED_EDGE('',*,*,#9389,.T.);
#12828=ORIENTED_EDGE('',*,*,#9390,.T.);
#12829=ORIENTED_EDGE('',*,*,#9391,.T.);
#12830=ORIENTED_EDGE('',*,*,#9392,.T.);
#12831=ORIENTED_EDGE('',*,*,#9393,.T.);
#12832=ORIENTED_EDGE('',*,*,#9394,.T.);
#12833=ORIENTED_EDGE('',*,*,#9395,.T.);
#12834=ORIENTED_EDGE('',*,*,#9396,.T.);
#12835=ORIENTED_EDGE('',*,*,#9397,.T.);
#12836=ORIENTED_EDGE('',*,*,#9398,.T.);
#12837=ORIENTED_EDGE('',*,*,#9399,.T.);
#12838=ORIENTED_EDGE('',*,*,#9400,.T.);
#12839=ORIENTED_EDGE('',*,*,#9401,.T.);
#12840=ORIENTED_EDGE('',*,*,#9402,.T.);
#12841=ORIENTED_EDGE('',*,*,#9403,.T.);
#12842=ORIENTED_EDGE('',*,*,#9404,.T.);
#12843=ORIENTED_EDGE('',*,*,#9405,.T.);
#12844=ORIENTED_EDGE('',*,*,#9406,.T.);
#12845=ORIENTED_EDGE('',*,*,#9407,.T.);
#12846=ORIENTED_EDGE('',*,*,#9408,.T.);
#12847=ORIENTED_EDGE('',*,*,#9409,.T.);
#12848=ORIENTED_EDGE('',*,*,#9410,.T.);
#12849=ORIENTED_EDGE('',*,*,#9411,.T.);
#12850=ORIENTED_EDGE('',*,*,#9412,.T.);
#12851=ORIENTED_EDGE('',*,*,#9413,.T.);
#12852=ORIENTED_EDGE('',*,*,#9414,.T.);
#12853=ORIENTED_EDGE('',*,*,#9415,.T.);
#12854=ORIENTED_EDGE('',*,*,#9416,.T.);
#12855=ORIENTED_EDGE('',*,*,#9417,.T.);
#12856=ORIENTED_EDGE('',*,*,#9418,.T.);
#12857=ORIENTED_EDGE('',*,*,#9419,.T.);
#12858=ORIENTED_EDGE('',*,*,#9420,.T.);
#12859=ORIENTED_EDGE('',*,*,#9421,.T.);
#12860=ORIENTED_EDGE('',*,*,#9422,.T.);
#12861=ORIENTED_EDGE('',*,*,#9423,.T.);
#12862=ORIENTED_EDGE('',*,*,#9424,.T.);
#12863=ORIENTED_EDGE('',*,*,#9425,.T.);
#12864=ORIENTED_EDGE('',*,*,#9426,.T.);
#12865=ORIENTED_EDGE('',*,*,#9427,.T.);
#12866=ORIENTED_EDGE('',*,*,#9428,.T.);
#12867=ORIENTED_EDGE('',*,*,#9429,.T.);
#12868=ORIENTED_EDGE('',*,*,#9430,.T.);
#12869=ORIENTED_EDGE('',*,*,#9431,.T.);
#12870=ORIENTED_EDGE('',*,*,#9432,.T.);
#12871=ORIENTED_EDGE('',*,*,#9433,.T.);
#12872=ORIENTED_EDGE('',*,*,#9434,.T.);
#12873=ORIENTED_EDGE('',*,*,#9435,.T.);
#12874=ORIENTED_EDGE('',*,*,#9436,.T.);
#12875=ORIENTED_EDGE('',*,*,#9437,.T.);
#12876=ORIENTED_EDGE('',*,*,#9438,.T.);
#12877=ORIENTED_EDGE('',*,*,#9439,.T.);
#12878=ORIENTED_EDGE('',*,*,#9440,.T.);
#12879=ORIENTED_EDGE('',*,*,#9441,.T.);
#12880=ORIENTED_EDGE('',*,*,#9442,.T.);
#12881=ORIENTED_EDGE('',*,*,#9443,.T.);
#12882=ORIENTED_EDGE('',*,*,#9444,.T.);
#12883=ORIENTED_EDGE('',*,*,#9445,.T.);
#12884=ORIENTED_EDGE('',*,*,#9446,.T.);
#12885=ORIENTED_EDGE('',*,*,#9447,.T.);
#12886=ORIENTED_EDGE('',*,*,#9448,.T.);
#12887=ORIENTED_EDGE('',*,*,#9449,.T.);
#12888=ORIENTED_EDGE('',*,*,#9450,.T.);
#12889=ORIENTED_EDGE('',*,*,#9451,.T.);
#12890=ORIENTED_EDGE('',*,*,#9452,.T.);
#12891=ORIENTED_EDGE('',*,*,#9007,.T.);
#12892=ORIENTED_EDGE('',*,*,#9453,.T.);
#12893=ORIENTED_EDGE('',*,*,#9013,.F.);
#12894=ORIENTED_EDGE('',*,*,#9454,.T.);
#12895=ORIENTED_EDGE('',*,*,#9455,.F.);
#12896=ORIENTED_EDGE('',*,*,#9200,.T.);
#12897=ORIENTED_EDGE('',*,*,#9456,.F.);
#12898=ORIENTED_EDGE('',*,*,#9210,.T.);
#12899=ORIENTED_EDGE('',*,*,#9203,.T.);
#12900=ORIENTED_EDGE('',*,*,#9457,.T.);
#12901=ORIENTED_EDGE('',*,*,#9458,.T.);
#12902=ORIENTED_EDGE('',*,*,#9459,.F.);
#12903=ORIENTED_EDGE('',*,*,#9204,.F.);
#12904=ORIENTED_EDGE('',*,*,#9459,.T.);
#12905=ORIENTED_EDGE('',*,*,#9460,.T.);
#12906=ORIENTED_EDGE('',*,*,#9461,.F.);
#12907=ORIENTED_EDGE('',*,*,#9462,.T.);
#12908=ORIENTED_EDGE('',*,*,#9463,.T.);
#12909=ORIENTED_EDGE('',*,*,#9464,.T.);
#12910=ORIENTED_EDGE('',*,*,#9465,.T.);
#12911=ORIENTED_EDGE('',*,*,#9466,.T.);
#12912=ORIENTED_EDGE('',*,*,#9467,.T.);
#12913=ORIENTED_EDGE('',*,*,#9468,.T.);
#12914=ORIENTED_EDGE('',*,*,#9469,.T.);
#12915=ORIENTED_EDGE('',*,*,#9470,.T.);
#12916=ORIENTED_EDGE('',*,*,#9471,.T.);
#12917=ORIENTED_EDGE('',*,*,#9472,.F.);
#12918=ORIENTED_EDGE('',*,*,#9473,.T.);
#12919=ORIENTED_EDGE('',*,*,#9474,.T.);
#12920=ORIENTED_EDGE('',*,*,#9475,.T.);
#12921=ORIENTED_EDGE('',*,*,#9476,.T.);
#12922=ORIENTED_EDGE('',*,*,#9477,.T.);
#12923=ORIENTED_EDGE('',*,*,#9478,.T.);
#12924=ORIENTED_EDGE('',*,*,#9479,.T.);
#12925=ORIENTED_EDGE('',*,*,#9480,.T.);
#12926=ORIENTED_EDGE('',*,*,#9481,.F.);
#12927=ORIENTED_EDGE('',*,*,#9482,.F.);
#12928=ORIENTED_EDGE('',*,*,#9483,.F.);
#12929=ORIENTED_EDGE('',*,*,#9460,.F.);
#12930=ORIENTED_EDGE('',*,*,#9458,.F.);
#12931=ORIENTED_EDGE('',*,*,#9000,.T.);
#12932=ORIENTED_EDGE('',*,*,#9484,.T.);
#12933=ORIENTED_EDGE('',*,*,#9485,.T.);
#12934=ORIENTED_EDGE('',*,*,#9486,.T.);
#12935=ORIENTED_EDGE('',*,*,#9487,.T.);
#12936=ORIENTED_EDGE('',*,*,#9488,.T.);
#12937=ORIENTED_EDGE('',*,*,#9004,.F.);
#12938=ORIENTED_EDGE('',*,*,#9489,.T.);
#12939=ORIENTED_EDGE('',*,*,#9490,.T.);
#12940=ORIENTED_EDGE('',*,*,#9491,.T.);
#12941=ORIENTED_EDGE('',*,*,#9492,.T.);
#12942=ORIENTED_EDGE('',*,*,#9493,.T.);
#12943=ORIENTED_EDGE('',*,*,#9494,.T.);
#12944=ORIENTED_EDGE('',*,*,#9495,.T.);
#12945=ORIENTED_EDGE('',*,*,#9496,.T.);
#12946=ORIENTED_EDGE('',*,*,#9497,.T.);
#12947=ORIENTED_EDGE('',*,*,#9498,.T.);
#12948=ORIENTED_EDGE('',*,*,#9499,.T.);
#12949=ORIENTED_EDGE('',*,*,#9500,.T.);
#12950=ORIENTED_EDGE('',*,*,#9501,.T.);
#12951=ORIENTED_EDGE('',*,*,#9502,.T.);
#12952=ORIENTED_EDGE('',*,*,#9503,.T.);
#12953=ORIENTED_EDGE('',*,*,#9504,.T.);
#12954=ORIENTED_EDGE('',*,*,#9505,.T.);
#12955=ORIENTED_EDGE('',*,*,#9466,.F.);
#12956=ORIENTED_EDGE('',*,*,#9506,.T.);
#12957=ORIENTED_EDGE('',*,*,#9507,.T.);
#12958=ORIENTED_EDGE('',*,*,#9472,.T.);
#12959=ORIENTED_EDGE('',*,*,#9508,.T.);
#12960=ORIENTED_EDGE('',*,*,#9509,.T.);
#12961=ORIENTED_EDGE('',*,*,#9481,.T.);
#12962=ORIENTED_EDGE('',*,*,#9510,.T.);
#12963=ORIENTED_EDGE('',*,*,#9511,.T.);
#12964=ORIENTED_EDGE('',*,*,#9467,.F.);
#12965=ORIENTED_EDGE('',*,*,#9512,.T.);
#12966=ORIENTED_EDGE('',*,*,#9513,.T.);
#12967=ORIENTED_EDGE('',*,*,#9514,.T.);
#12968=ORIENTED_EDGE('',*,*,#9515,.T.);
#12969=ORIENTED_EDGE('',*,*,#9516,.T.);
#12970=ORIENTED_EDGE('',*,*,#9517,.T.);
#12971=ORIENTED_EDGE('',*,*,#9518,.T.);
#12972=ORIENTED_EDGE('',*,*,#9519,.T.);
#12973=ORIENTED_EDGE('',*,*,#9520,.T.);
#12974=ORIENTED_EDGE('',*,*,#9521,.T.);
#12975=ORIENTED_EDGE('',*,*,#9522,.T.);
#12976=ORIENTED_EDGE('',*,*,#9523,.T.);
#12977=ORIENTED_EDGE('',*,*,#9524,.T.);
#12978=ORIENTED_EDGE('',*,*,#9525,.T.);
#12979=ORIENTED_EDGE('',*,*,#9526,.T.);
#12980=ORIENTED_EDGE('',*,*,#9527,.T.);
#12981=ORIENTED_EDGE('',*,*,#9526,.F.);
#12982=ORIENTED_EDGE('',*,*,#9528,.T.);
#12983=ORIENTED_EDGE('',*,*,#9529,.T.);
#12984=ORIENTED_EDGE('',*,*,#9530,.T.);
#12985=ORIENTED_EDGE('',*,*,#9531,.T.);
#12986=ORIENTED_EDGE('',*,*,#9532,.T.);
#12987=ORIENTED_EDGE('',*,*,#9533,.T.);
#12988=ORIENTED_EDGE('',*,*,#9534,.T.);
#12989=ORIENTED_EDGE('',*,*,#9535,.T.);
#12990=ORIENTED_EDGE('',*,*,#9536,.T.);
#12991=ORIENTED_EDGE('',*,*,#9537,.T.);
#12992=ORIENTED_EDGE('',*,*,#9538,.T.);
#12993=ORIENTED_EDGE('',*,*,#9539,.T.);
#12994=ORIENTED_EDGE('',*,*,#9540,.T.);
#12995=ORIENTED_EDGE('',*,*,#9541,.T.);
#12996=ORIENTED_EDGE('',*,*,#9542,.T.);
#12997=ORIENTED_EDGE('',*,*,#9543,.T.);
#12998=ORIENTED_EDGE('',*,*,#9544,.T.);
#12999=ORIENTED_EDGE('',*,*,#9521,.F.);
#13000=ORIENTED_EDGE('',*,*,#9545,.T.);
#13001=ORIENTED_EDGE('',*,*,#9546,.T.);
#13002=ORIENTED_EDGE('',*,*,#9547,.T.);
#13003=ORIENTED_EDGE('',*,*,#9548,.T.);
#13004=ORIENTED_EDGE('',*,*,#9549,.T.);
#13005=ORIENTED_EDGE('',*,*,#9533,.F.);
#13006=ORIENTED_EDGE('',*,*,#9550,.T.);
#13007=ORIENTED_EDGE('',*,*,#9551,.T.);
#13008=ORIENTED_EDGE('',*,*,#9552,.T.);
#13009=ORIENTED_EDGE('',*,*,#9553,.T.);
#13010=ORIENTED_EDGE('',*,*,#9539,.F.);
#13011=ORIENTED_EDGE('',*,*,#9554,.T.);
#13012=ORIENTED_EDGE('',*,*,#9555,.T.);
#13013=ORIENTED_EDGE('',*,*,#9556,.T.);
#13014=ORIENTED_EDGE('',*,*,#9557,.T.);
#13015=ORIENTED_EDGE('',*,*,#9515,.F.);
#13016=ORIENTED_EDGE('',*,*,#9558,.T.);
#13017=ORIENTED_EDGE('',*,*,#9559,.T.);
#13018=ORIENTED_EDGE('',*,*,#9560,.T.);
#13019=ORIENTED_EDGE('',*,*,#9519,.F.);
#13020=ORIENTED_EDGE('',*,*,#9561,.T.);
#13021=ORIENTED_EDGE('',*,*,#9562,.T.);
#13022=ORIENTED_EDGE('',*,*,#9504,.F.);
#13023=ORIENTED_EDGE('',*,*,#9563,.T.);
#13024=ORIENTED_EDGE('',*,*,#9564,.T.);
#13025=ORIENTED_EDGE('',*,*,#9565,.T.);
#13026=ORIENTED_EDGE('',*,*,#9566,.T.);
#13027=ORIENTED_EDGE('',*,*,#9500,.F.);
#13028=ORIENTED_EDGE('',*,*,#9567,.F.);
#13029=ORIENTED_EDGE('',*,*,#9509,.F.);
#13030=ORIENTED_EDGE('',*,*,#9508,.F.);
#13031=ORIENTED_EDGE('',*,*,#9568,.F.);
#13032=ORIENTED_EDGE('',*,*,#9492,.F.);
#13033=ORIENTED_EDGE('',*,*,#9568,.T.);
#13034=ORIENTED_EDGE('',*,*,#9476,.F.);
#13035=ORIENTED_EDGE('',*,*,#9569,.F.);
#13036=ORIENTED_EDGE('',*,*,#9493,.F.);
#13037=ORIENTED_EDGE('',*,*,#9491,.F.);
#13038=ORIENTED_EDGE('',*,*,#9570,.T.);
#13039=ORIENTED_EDGE('',*,*,#9462,.F.);
#13040=ORIENTED_EDGE('',*,*,#9567,.T.);
#13041=ORIENTED_EDGE('',*,*,#9475,.F.);
#13042=ORIENTED_EDGE('',*,*,#9571,.T.);
#13043=ORIENTED_EDGE('',*,*,#9558,.F.);
#13044=ORIENTED_EDGE('',*,*,#9518,.F.);
#13045=ORIENTED_EDGE('',*,*,#9572,.F.);
#13046=ORIENTED_EDGE('',*,*,#9494,.F.);
#13047=ORIENTED_EDGE('',*,*,#9569,.T.);
#13048=ORIENTED_EDGE('',*,*,#9566,.F.);
#13049=ORIENTED_EDGE('',*,*,#9573,.T.);
#13050=ORIENTED_EDGE('',*,*,#9490,.F.);
#13051=ORIENTED_EDGE('',*,*,#9574,.F.);
#13052=ORIENTED_EDGE('',*,*,#9501,.F.);
#13053=ORIENTED_EDGE('',*,*,#9572,.T.);
#13054=ORIENTED_EDGE('',*,*,#9517,.F.);
#13055=ORIENTED_EDGE('',*,*,#9575,.F.);
#13056=ORIENTED_EDGE('',*,*,#9495,.F.);
#13057=ORIENTED_EDGE('',*,*,#9574,.T.);
#13058=ORIENTED_EDGE('',*,*,#9489,.F.);
#13059=ORIENTED_EDGE('',*,*,#9576,.F.);
#13060=ORIENTED_EDGE('',*,*,#9502,.F.);
#13061=ORIENTED_EDGE('',*,*,#9557,.F.);
#13062=ORIENTED_EDGE('',*,*,#9577,.T.);
#13063=ORIENTED_EDGE('',*,*,#9496,.F.);
#13064=ORIENTED_EDGE('',*,*,#9575,.T.);
#13065=ORIENTED_EDGE('',*,*,#9516,.F.);
#13066=ORIENTED_EDGE('',*,*,#9003,.F.);
#13067=ORIENTED_EDGE('',*,*,#9578,.T.);
#13068=ORIENTED_EDGE('',*,*,#9563,.F.);
#13069=ORIENTED_EDGE('',*,*,#9503,.F.);
#13070=ORIENTED_EDGE('',*,*,#9576,.T.);
#13071=ORIENTED_EDGE('',*,*,#9497,.F.);
#13072=ORIENTED_EDGE('',*,*,#9579,.T.);
#13073=ORIENTED_EDGE('',*,*,#9477,.F.);
#13074=ORIENTED_EDGE('',*,*,#9580,.F.);
#13075=ORIENTED_EDGE('',*,*,#9471,.F.);
#13076=ORIENTED_EDGE('',*,*,#9581,.T.);
#13077=ORIENTED_EDGE('',*,*,#9002,.F.);
#13078=ORIENTED_EDGE('',*,*,#9582,.F.);
#13079=ORIENTED_EDGE('',*,*,#9580,.T.);
#13080=ORIENTED_EDGE('',*,*,#9513,.F.);
#13081=ORIENTED_EDGE('',*,*,#9512,.F.);
#13082=ORIENTED_EDGE('',*,*,#9582,.T.);
#13083=ORIENTED_EDGE('',*,*,#9001,.F.);
#13084=ORIENTED_EDGE('',*,*,#9498,.F.);
#13085=ORIENTED_EDGE('',*,*,#9583,.F.);
#13086=ORIENTED_EDGE('',*,*,#9527,.F.);
#13087=ORIENTED_EDGE('',*,*,#9584,.F.);
#13088=ORIENTED_EDGE('',*,*,#9486,.F.);
#13089=ORIENTED_EDGE('',*,*,#9485,.F.);
#13090=ORIENTED_EDGE('',*,*,#9584,.T.);
#13091=ORIENTED_EDGE('',*,*,#9538,.F.);
#13092=ORIENTED_EDGE('',*,*,#9537,.F.);
#13093=ORIENTED_EDGE('',*,*,#9536,.F.);
#13094=ORIENTED_EDGE('',*,*,#9535,.F.);
#13095=ORIENTED_EDGE('',*,*,#9534,.F.);
#13096=ORIENTED_EDGE('',*,*,#9585,.F.);
#13097=ORIENTED_EDGE('',*,*,#9487,.F.);
#13098=ORIENTED_EDGE('',*,*,#9583,.T.);
#13099=ORIENTED_EDGE('',*,*,#9484,.F.);
#13100=ORIENTED_EDGE('',*,*,#9006,.F.);
#13101=ORIENTED_EDGE('',*,*,#9586,.F.);
#13102=ORIENTED_EDGE('',*,*,#9549,.F.);
#13103=ORIENTED_EDGE('',*,*,#9548,.F.);
#13104=ORIENTED_EDGE('',*,*,#9547,.F.);
#13105=ORIENTED_EDGE('',*,*,#9546,.F.);
#13106=ORIENTED_EDGE('',*,*,#9545,.F.);
#13107=ORIENTED_EDGE('',*,*,#9585,.T.);
#13108=ORIENTED_EDGE('',*,*,#9554,.F.);
#13109=ORIENTED_EDGE('',*,*,#9586,.T.);
#13110=ORIENTED_EDGE('',*,*,#9005,.F.);
#13111=ORIENTED_EDGE('',*,*,#9488,.F.);
#13112=ORIENTED_EDGE('',*,*,#9587,.F.);
#13113=ORIENTED_EDGE('',*,*,#9578,.F.);
#13114=ORIENTED_EDGE('',*,*,#9581,.F.);
#13115=ORIENTED_EDGE('',*,*,#9470,.F.);
#13116=ORIENTED_EDGE('',*,*,#9588,.T.);
#13117=ORIENTED_EDGE('',*,*,#9561,.F.);
#13118=ORIENTED_EDGE('',*,*,#9587,.T.);
#13119=ORIENTED_EDGE('',*,*,#9158,.F.);
#13120=ORIENTED_EDGE('',*,*,#9589,.T.);
#13121=ORIENTED_EDGE('',*,*,#9469,.F.);
#13122=ORIENTED_EDGE('',*,*,#9468,.F.);
#13123=ORIENTED_EDGE('',*,*,#9590,.F.);
#13124=ORIENTED_EDGE('',*,*,#9590,.T.);
#13125=ORIENTED_EDGE('',*,*,#9511,.F.);
#13126=ORIENTED_EDGE('',*,*,#9510,.F.);
#13127=ORIENTED_EDGE('',*,*,#9591,.F.);
#13128=ORIENTED_EDGE('',*,*,#9213,.F.);
#13129=ORIENTED_EDGE('',*,*,#9159,.F.);
#13130=ORIENTED_EDGE('',*,*,#9479,.F.);
#13131=ORIENTED_EDGE('',*,*,#9592,.T.);
#13132=ORIENTED_EDGE('',*,*,#9214,.F.);
#13133=ORIENTED_EDGE('',*,*,#9591,.T.);
#13134=ORIENTED_EDGE('',*,*,#9480,.F.);
#13135=ORIENTED_EDGE('',*,*,#9224,.F.);
#13136=ORIENTED_EDGE('',*,*,#9593,.T.);
#13137=ORIENTED_EDGE('',*,*,#9564,.F.);
#13138=ORIENTED_EDGE('',*,*,#9594,.F.);
#13139=ORIENTED_EDGE('',*,*,#9152,.F.);
#13140=ORIENTED_EDGE('',*,*,#9499,.F.);
#13141=ORIENTED_EDGE('',*,*,#9154,.F.);
#13142=ORIENTED_EDGE('',*,*,#9153,.F.);
#13143=ORIENTED_EDGE('',*,*,#9594,.T.);
#13144=ORIENTED_EDGE('',*,*,#9155,.F.);
#13145=ORIENTED_EDGE('',*,*,#9505,.F.);
#13146=ORIENTED_EDGE('',*,*,#9595,.F.);
#13147=ORIENTED_EDGE('',*,*,#9156,.F.);
#13148=ORIENTED_EDGE('',*,*,#9596,.F.);
#13149=ORIENTED_EDGE('',*,*,#9157,.F.);
#13150=ORIENTED_EDGE('',*,*,#9595,.T.);
#13151=ORIENTED_EDGE('',*,*,#9562,.F.);
#13152=ORIENTED_EDGE('',*,*,#9596,.T.);
#13153=ORIENTED_EDGE('',*,*,#9588,.F.);
#13154=ORIENTED_EDGE('',*,*,#9589,.F.);
#13155=ORIENTED_EDGE('',*,*,#9514,.F.);
#13156=ORIENTED_EDGE('',*,*,#9217,.F.);
#13157=ORIENTED_EDGE('',*,*,#9216,.F.);
#13158=ORIENTED_EDGE('',*,*,#9597,.F.);
#13159=ORIENTED_EDGE('',*,*,#9597,.T.);
#13160=ORIENTED_EDGE('',*,*,#9215,.F.);
#13161=ORIENTED_EDGE('',*,*,#9598,.F.);
#13162=ORIENTED_EDGE('',*,*,#9555,.F.);
#13163=ORIENTED_EDGE('',*,*,#9598,.T.);
#13164=ORIENTED_EDGE('',*,*,#9592,.F.);
#13165=ORIENTED_EDGE('',*,*,#9599,.F.);
#13166=ORIENTED_EDGE('',*,*,#9600,.F.);
#13167=ORIENTED_EDGE('',*,*,#9556,.F.);
#13168=ORIENTED_EDGE('',*,*,#9599,.T.);
#13169=ORIENTED_EDGE('',*,*,#9478,.F.);
#13170=ORIENTED_EDGE('',*,*,#9579,.F.);
#13171=ORIENTED_EDGE('',*,*,#9577,.F.);
#13172=ORIENTED_EDGE('',*,*,#9600,.T.);
#13173=ORIENTED_EDGE('',*,*,#9218,.F.);
#13174=ORIENTED_EDGE('',*,*,#9520,.F.);
#13175=ORIENTED_EDGE('',*,*,#9601,.F.);
#13176=ORIENTED_EDGE('',*,*,#9219,.F.);
#13177=ORIENTED_EDGE('',*,*,#9601,.T.);
#13178=ORIENTED_EDGE('',*,*,#9560,.F.);
#13179=ORIENTED_EDGE('',*,*,#9602,.F.);
#13180=ORIENTED_EDGE('',*,*,#9220,.F.);
#13181=ORIENTED_EDGE('',*,*,#9571,.F.);
#13182=ORIENTED_EDGE('',*,*,#9474,.F.);
#13183=ORIENTED_EDGE('',*,*,#9473,.F.);
#13184=ORIENTED_EDGE('',*,*,#9603,.F.);
#13185=ORIENTED_EDGE('',*,*,#9221,.F.);
#13186=ORIENTED_EDGE('',*,*,#9602,.T.);
#13187=ORIENTED_EDGE('',*,*,#9559,.F.);
#13188=ORIENTED_EDGE('',*,*,#9603,.T.);
#13189=ORIENTED_EDGE('',*,*,#9507,.F.);
#13190=ORIENTED_EDGE('',*,*,#9506,.F.);
#13191=ORIENTED_EDGE('',*,*,#9604,.F.);
#13192=ORIENTED_EDGE('',*,*,#9222,.F.);
#13193=ORIENTED_EDGE('',*,*,#9605,.F.);
#13194=ORIENTED_EDGE('',*,*,#9223,.F.);
#13195=ORIENTED_EDGE('',*,*,#9604,.T.);
#13196=ORIENTED_EDGE('',*,*,#9465,.F.);
#13197=ORIENTED_EDGE('',*,*,#9464,.F.);
#13198=ORIENTED_EDGE('',*,*,#9593,.F.);
#13199=ORIENTED_EDGE('',*,*,#9605,.T.);
#13200=ORIENTED_EDGE('',*,*,#9606,.F.);
#13201=ORIENTED_EDGE('',*,*,#9607,.F.);
#13202=ORIENTED_EDGE('',*,*,#9565,.F.);
#13203=ORIENTED_EDGE('',*,*,#9606,.T.);
#13204=ORIENTED_EDGE('',*,*,#9463,.F.);
#13205=ORIENTED_EDGE('',*,*,#9607,.T.);
#13206=ORIENTED_EDGE('',*,*,#9570,.F.);
#13207=ORIENTED_EDGE('',*,*,#9573,.F.);
#13208=ORIENTED_EDGE('',*,*,#9608,.F.);
#13209=ORIENTED_EDGE('',*,*,#9008,.F.);
#13210=ORIENTED_EDGE('',*,*,#9454,.F.);
#13211=ORIENTED_EDGE('',*,*,#9012,.F.);
#13212=ORIENTED_EDGE('',*,*,#9609,.F.);
#13213=ORIENTED_EDGE('',*,*,#9544,.F.);
#13214=ORIENTED_EDGE('',*,*,#9543,.F.);
#13215=ORIENTED_EDGE('',*,*,#9542,.F.);
#13216=ORIENTED_EDGE('',*,*,#9541,.F.);
#13217=ORIENTED_EDGE('',*,*,#9540,.F.);
#13218=ORIENTED_EDGE('',*,*,#9609,.T.);
#13219=ORIENTED_EDGE('',*,*,#9011,.F.);
#13220=ORIENTED_EDGE('',*,*,#9610,.F.);
#13221=ORIENTED_EDGE('',*,*,#9525,.F.);
#13222=ORIENTED_EDGE('',*,*,#9524,.F.);
#13223=ORIENTED_EDGE('',*,*,#9523,.F.);
#13224=ORIENTED_EDGE('',*,*,#9522,.F.);
#13225=ORIENTED_EDGE('',*,*,#9608,.T.);
#13226=ORIENTED_EDGE('',*,*,#9553,.F.);
#13227=ORIENTED_EDGE('',*,*,#9552,.F.);
#13228=ORIENTED_EDGE('',*,*,#9551,.F.);
#13229=ORIENTED_EDGE('',*,*,#9550,.F.);
#13230=ORIENTED_EDGE('',*,*,#9611,.F.);
#13231=ORIENTED_EDGE('',*,*,#9009,.F.);
#13232=ORIENTED_EDGE('',*,*,#9610,.T.);
#13233=ORIENTED_EDGE('',*,*,#9010,.F.);
#13234=ORIENTED_EDGE('',*,*,#9611,.T.);
#13235=ORIENTED_EDGE('',*,*,#9532,.F.);
#13236=ORIENTED_EDGE('',*,*,#9531,.F.);
#13237=ORIENTED_EDGE('',*,*,#9530,.F.);
#13238=ORIENTED_EDGE('',*,*,#9529,.F.);
#13239=ORIENTED_EDGE('',*,*,#9528,.F.);
#13240=ORIENTED_EDGE('',*,*,#9483,.T.);
#13241=ORIENTED_EDGE('',*,*,#9612,.T.);
#13242=ORIENTED_EDGE('',*,*,#9201,.F.);
#13243=ORIENTED_EDGE('',*,*,#9461,.T.);
#13244=ORIENTED_EDGE('',*,*,#9168,.F.);
#13245=ORIENTED_EDGE('',*,*,#9613,.T.);
#13246=ORIENTED_EDGE('',*,*,#9614,.T.);
#13247=ORIENTED_EDGE('',*,*,#9615,.T.);
#13248=ORIENTED_EDGE('',*,*,#9616,.T.);
#13249=ORIENTED_EDGE('',*,*,#9617,.T.);
#13250=ORIENTED_EDGE('',*,*,#9618,.T.);
#13251=ORIENTED_EDGE('',*,*,#9619,.T.);
#13252=ORIENTED_EDGE('',*,*,#9620,.T.);
#13253=ORIENTED_EDGE('',*,*,#9621,.T.);
#13254=ORIENTED_EDGE('',*,*,#9622,.T.);
#13255=ORIENTED_EDGE('',*,*,#9623,.T.);
#13256=ORIENTED_EDGE('',*,*,#9624,.T.);
#13257=ORIENTED_EDGE('',*,*,#9625,.T.);
#13258=ORIENTED_EDGE('',*,*,#9626,.T.);
#13259=ORIENTED_EDGE('',*,*,#9627,.T.);
#13260=ORIENTED_EDGE('',*,*,#9628,.T.);
#13261=ORIENTED_EDGE('',*,*,#9629,.T.);
#13262=ORIENTED_EDGE('',*,*,#9630,.T.);
#13263=ORIENTED_EDGE('',*,*,#9631,.T.);
#13264=ORIENTED_EDGE('',*,*,#9632,.T.);
#13265=ORIENTED_EDGE('',*,*,#9633,.T.);
#13266=ORIENTED_EDGE('',*,*,#9634,.T.);
#13267=ORIENTED_EDGE('',*,*,#9635,.T.);
#13268=ORIENTED_EDGE('',*,*,#9636,.T.);
#13269=ORIENTED_EDGE('',*,*,#9637,.T.);
#13270=ORIENTED_EDGE('',*,*,#9638,.T.);
#13271=ORIENTED_EDGE('',*,*,#9639,.T.);
#13272=ORIENTED_EDGE('',*,*,#9640,.T.);
#13273=ORIENTED_EDGE('',*,*,#9641,.T.);
#13274=ORIENTED_EDGE('',*,*,#9642,.T.);
#13275=ORIENTED_EDGE('',*,*,#9643,.T.);
#13276=ORIENTED_EDGE('',*,*,#9644,.T.);
#13277=ORIENTED_EDGE('',*,*,#9645,.T.);
#13278=ORIENTED_EDGE('',*,*,#9646,.T.);
#13279=ORIENTED_EDGE('',*,*,#9647,.T.);
#13280=ORIENTED_EDGE('',*,*,#9648,.T.);
#13281=ORIENTED_EDGE('',*,*,#9649,.T.);
#13282=ORIENTED_EDGE('',*,*,#9650,.T.);
#13283=ORIENTED_EDGE('',*,*,#9651,.T.);
#13284=ORIENTED_EDGE('',*,*,#9652,.T.);
#13285=ORIENTED_EDGE('',*,*,#9653,.T.);
#13286=ORIENTED_EDGE('',*,*,#9654,.T.);
#13287=ORIENTED_EDGE('',*,*,#9655,.T.);
#13288=ORIENTED_EDGE('',*,*,#9656,.T.);
#13289=ORIENTED_EDGE('',*,*,#9657,.T.);
#13290=ORIENTED_EDGE('',*,*,#9658,.T.);
#13291=ORIENTED_EDGE('',*,*,#9659,.T.);
#13292=ORIENTED_EDGE('',*,*,#9660,.T.);
#13293=ORIENTED_EDGE('',*,*,#9661,.T.);
#13294=ORIENTED_EDGE('',*,*,#9662,.T.);
#13295=ORIENTED_EDGE('',*,*,#9663,.T.);
#13296=ORIENTED_EDGE('',*,*,#9664,.T.);
#13297=ORIENTED_EDGE('',*,*,#9665,.T.);
#13298=ORIENTED_EDGE('',*,*,#9666,.T.);
#13299=ORIENTED_EDGE('',*,*,#9667,.T.);
#13300=ORIENTED_EDGE('',*,*,#9668,.T.);
#13301=ORIENTED_EDGE('',*,*,#9669,.T.);
#13302=ORIENTED_EDGE('',*,*,#9670,.T.);
#13303=ORIENTED_EDGE('',*,*,#9671,.T.);
#13304=ORIENTED_EDGE('',*,*,#9672,.T.);
#13305=ORIENTED_EDGE('',*,*,#9673,.T.);
#13306=ORIENTED_EDGE('',*,*,#9674,.T.);
#13307=ORIENTED_EDGE('',*,*,#9675,.T.);
#13308=ORIENTED_EDGE('',*,*,#9676,.T.);
#13309=ORIENTED_EDGE('',*,*,#9677,.T.);
#13310=ORIENTED_EDGE('',*,*,#9678,.T.);
#13311=ORIENTED_EDGE('',*,*,#9679,.T.);
#13312=ORIENTED_EDGE('',*,*,#9680,.T.);
#13313=ORIENTED_EDGE('',*,*,#9681,.T.);
#13314=ORIENTED_EDGE('',*,*,#9682,.T.);
#13315=ORIENTED_EDGE('',*,*,#9683,.T.);
#13316=ORIENTED_EDGE('',*,*,#9684,.T.);
#13317=ORIENTED_EDGE('',*,*,#9685,.T.);
#13318=ORIENTED_EDGE('',*,*,#9686,.T.);
#13319=ORIENTED_EDGE('',*,*,#9687,.T.);
#13320=ORIENTED_EDGE('',*,*,#9688,.T.);
#13321=ORIENTED_EDGE('',*,*,#9689,.T.);
#13322=ORIENTED_EDGE('',*,*,#9690,.T.);
#13323=ORIENTED_EDGE('',*,*,#9691,.T.);
#13324=ORIENTED_EDGE('',*,*,#9692,.T.);
#13325=ORIENTED_EDGE('',*,*,#9693,.T.);
#13326=ORIENTED_EDGE('',*,*,#9694,.T.);
#13327=ORIENTED_EDGE('',*,*,#9695,.T.);
#13328=ORIENTED_EDGE('',*,*,#9696,.T.);
#13329=ORIENTED_EDGE('',*,*,#9697,.T.);
#13330=ORIENTED_EDGE('',*,*,#9698,.T.);
#13331=ORIENTED_EDGE('',*,*,#9699,.T.);
#13332=ORIENTED_EDGE('',*,*,#9700,.T.);
#13333=ORIENTED_EDGE('',*,*,#9701,.T.);
#13334=ORIENTED_EDGE('',*,*,#9702,.T.);
#13335=ORIENTED_EDGE('',*,*,#9703,.T.);
#13336=ORIENTED_EDGE('',*,*,#9704,.T.);
#13337=ORIENTED_EDGE('',*,*,#9705,.T.);
#13338=ORIENTED_EDGE('',*,*,#9706,.T.);
#13339=ORIENTED_EDGE('',*,*,#9707,.T.);
#13340=ORIENTED_EDGE('',*,*,#9708,.T.);
#13341=ORIENTED_EDGE('',*,*,#9709,.T.);
#13342=ORIENTED_EDGE('',*,*,#9710,.T.);
#13343=ORIENTED_EDGE('',*,*,#9711,.T.);
#13344=ORIENTED_EDGE('',*,*,#9712,.T.);
#13345=ORIENTED_EDGE('',*,*,#9713,.T.);
#13346=ORIENTED_EDGE('',*,*,#9714,.T.);
#13347=ORIENTED_EDGE('',*,*,#9715,.T.);
#13348=ORIENTED_EDGE('',*,*,#9716,.T.);
#13349=ORIENTED_EDGE('',*,*,#9717,.T.);
#13350=ORIENTED_EDGE('',*,*,#9718,.T.);
#13351=ORIENTED_EDGE('',*,*,#9719,.T.);
#13352=ORIENTED_EDGE('',*,*,#9720,.T.);
#13353=ORIENTED_EDGE('',*,*,#9721,.T.);
#13354=ORIENTED_EDGE('',*,*,#9198,.T.);
#13355=ORIENTED_EDGE('',*,*,#9722,.T.);
#13356=ORIENTED_EDGE('',*,*,#9212,.T.);
#13357=ORIENTED_EDGE('',*,*,#9723,.F.);
#13358=ORIENTED_EDGE('',*,*,#9211,.T.);
#13359=ORIENTED_EDGE('',*,*,#9456,.T.);
#13360=ORIENTED_EDGE('',*,*,#9199,.T.);
#13361=ORIENTED_EDGE('',*,*,#9723,.T.);
#13362=ORIENTED_EDGE('',*,*,#9724,.F.);
#13363=ORIENTED_EDGE('',*,*,#9725,.F.);
#13364=ORIENTED_EDGE('',*,*,#9726,.F.);
#13365=ORIENTED_EDGE('',*,*,#9727,.F.);
#13366=ORIENTED_EDGE('',*,*,#9728,.F.);
#13367=ORIENTED_EDGE('',*,*,#9729,.F.);
#13368=ORIENTED_EDGE('',*,*,#9730,.F.);
#13369=ORIENTED_EDGE('',*,*,#9731,.F.);
#13370=ORIENTED_EDGE('',*,*,#9732,.F.);
#13371=ORIENTED_EDGE('',*,*,#9733,.F.);
#13372=ORIENTED_EDGE('',*,*,#9734,.F.);
#13373=ORIENTED_EDGE('',*,*,#9735,.F.);
#13374=ORIENTED_EDGE('',*,*,#9736,.F.);
#13375=ORIENTED_EDGE('',*,*,#9737,.F.);
#13376=ORIENTED_EDGE('',*,*,#9738,.F.);
#13377=ORIENTED_EDGE('',*,*,#9739,.F.);
#13378=ORIENTED_EDGE('',*,*,#9740,.F.);
#13379=ORIENTED_EDGE('',*,*,#9741,.F.);
#13380=ORIENTED_EDGE('',*,*,#9742,.F.);
#13381=ORIENTED_EDGE('',*,*,#9743,.F.);
#13382=ORIENTED_EDGE('',*,*,#9744,.F.);
#13383=ORIENTED_EDGE('',*,*,#9745,.F.);
#13384=ORIENTED_EDGE('',*,*,#9746,.F.);
#13385=ORIENTED_EDGE('',*,*,#9747,.F.);
#13386=ORIENTED_EDGE('',*,*,#9748,.F.);
#13387=ORIENTED_EDGE('',*,*,#9749,.F.);
#13388=ORIENTED_EDGE('',*,*,#9750,.F.);
#13389=ORIENTED_EDGE('',*,*,#9751,.F.);
#13390=ORIENTED_EDGE('',*,*,#9752,.F.);
#13391=ORIENTED_EDGE('',*,*,#9753,.F.);
#13392=ORIENTED_EDGE('',*,*,#9754,.F.);
#13393=ORIENTED_EDGE('',*,*,#9755,.F.);
#13394=ORIENTED_EDGE('',*,*,#9756,.F.);
#13395=ORIENTED_EDGE('',*,*,#9757,.F.);
#13396=ORIENTED_EDGE('',*,*,#9758,.F.);
#13397=ORIENTED_EDGE('',*,*,#9759,.F.);
#13398=ORIENTED_EDGE('',*,*,#9760,.F.);
#13399=ORIENTED_EDGE('',*,*,#9761,.F.);
#13400=ORIENTED_EDGE('',*,*,#9762,.F.);
#13401=ORIENTED_EDGE('',*,*,#9763,.F.);
#13402=ORIENTED_EDGE('',*,*,#9764,.F.);
#13403=ORIENTED_EDGE('',*,*,#9765,.F.);
#13404=ORIENTED_EDGE('',*,*,#9766,.F.);
#13405=ORIENTED_EDGE('',*,*,#9767,.F.);
#13406=ORIENTED_EDGE('',*,*,#9768,.F.);
#13407=ORIENTED_EDGE('',*,*,#9769,.F.);
#13408=ORIENTED_EDGE('',*,*,#9770,.F.);
#13409=ORIENTED_EDGE('',*,*,#9771,.F.);
#13410=ORIENTED_EDGE('',*,*,#9772,.F.);
#13411=ORIENTED_EDGE('',*,*,#9773,.F.);
#13412=ORIENTED_EDGE('',*,*,#9774,.F.);
#13413=ORIENTED_EDGE('',*,*,#9775,.F.);
#13414=ORIENTED_EDGE('',*,*,#9776,.F.);
#13415=ORIENTED_EDGE('',*,*,#9777,.F.);
#13416=ORIENTED_EDGE('',*,*,#9778,.F.);
#13417=ORIENTED_EDGE('',*,*,#9779,.F.);
#13418=ORIENTED_EDGE('',*,*,#9780,.F.);
#13419=ORIENTED_EDGE('',*,*,#9781,.F.);
#13420=ORIENTED_EDGE('',*,*,#9782,.F.);
#13421=ORIENTED_EDGE('',*,*,#9783,.F.);
#13422=ORIENTED_EDGE('',*,*,#9784,.F.);
#13423=ORIENTED_EDGE('',*,*,#9785,.F.);
#13424=ORIENTED_EDGE('',*,*,#9786,.F.);
#13425=ORIENTED_EDGE('',*,*,#9787,.F.);
#13426=ORIENTED_EDGE('',*,*,#9788,.F.);
#13427=ORIENTED_EDGE('',*,*,#9789,.F.);
#13428=ORIENTED_EDGE('',*,*,#9790,.F.);
#13429=ORIENTED_EDGE('',*,*,#9791,.F.);
#13430=ORIENTED_EDGE('',*,*,#9792,.F.);
#13431=ORIENTED_EDGE('',*,*,#9793,.F.);
#13432=ORIENTED_EDGE('',*,*,#9794,.F.);
#13433=ORIENTED_EDGE('',*,*,#9795,.F.);
#13434=ORIENTED_EDGE('',*,*,#9796,.F.);
#13435=ORIENTED_EDGE('',*,*,#9797,.F.);
#13436=ORIENTED_EDGE('',*,*,#9798,.F.);
#13437=ORIENTED_EDGE('',*,*,#9799,.F.);
#13438=ORIENTED_EDGE('',*,*,#9800,.F.);
#13439=ORIENTED_EDGE('',*,*,#9801,.F.);
#13440=ORIENTED_EDGE('',*,*,#9802,.F.);
#13441=ORIENTED_EDGE('',*,*,#9803,.F.);
#13442=ORIENTED_EDGE('',*,*,#9804,.F.);
#13443=ORIENTED_EDGE('',*,*,#9805,.F.);
#13444=ORIENTED_EDGE('',*,*,#9806,.F.);
#13445=ORIENTED_EDGE('',*,*,#9807,.F.);
#13446=ORIENTED_EDGE('',*,*,#9808,.F.);
#13447=ORIENTED_EDGE('',*,*,#9809,.F.);
#13448=ORIENTED_EDGE('',*,*,#9810,.F.);
#13449=ORIENTED_EDGE('',*,*,#9811,.F.);
#13450=ORIENTED_EDGE('',*,*,#9812,.F.);
#13451=ORIENTED_EDGE('',*,*,#9813,.F.);
#13452=ORIENTED_EDGE('',*,*,#9814,.F.);
#13453=ORIENTED_EDGE('',*,*,#9815,.F.);
#13454=ORIENTED_EDGE('',*,*,#9816,.F.);
#13455=ORIENTED_EDGE('',*,*,#9817,.F.);
#13456=ORIENTED_EDGE('',*,*,#9818,.F.);
#13457=ORIENTED_EDGE('',*,*,#9819,.F.);
#13458=ORIENTED_EDGE('',*,*,#9820,.F.);
#13459=ORIENTED_EDGE('',*,*,#9821,.F.);
#13460=ORIENTED_EDGE('',*,*,#9822,.F.);
#13461=ORIENTED_EDGE('',*,*,#9823,.F.);
#13462=ORIENTED_EDGE('',*,*,#9824,.F.);
#13463=ORIENTED_EDGE('',*,*,#9825,.F.);
#13464=ORIENTED_EDGE('',*,*,#9612,.F.);
#13465=ORIENTED_EDGE('',*,*,#9482,.T.);
#13466=ORIENTED_EDGE('',*,*,#9457,.F.);
#13467=ORIENTED_EDGE('',*,*,#9202,.F.);
#13468=ORIENTED_EDGE('',*,*,#9197,.F.);
#13469=ORIENTED_EDGE('',*,*,#9455,.T.);
#13470=ORIENTED_EDGE('',*,*,#9209,.T.);
#13471=ORIENTED_EDGE('',*,*,#9722,.F.);
#13472=ORIENTED_EDGE('',*,*,#9826,.F.);
#13473=ORIENTED_EDGE('',*,*,#9330,.F.);
#13474=ORIENTED_EDGE('',*,*,#9827,.F.);
#13475=ORIENTED_EDGE('',*,*,#9624,.F.);
#13476=ORIENTED_EDGE('',*,*,#9827,.T.);
#13477=ORIENTED_EDGE('',*,*,#9329,.F.);
#13478=ORIENTED_EDGE('',*,*,#9828,.F.);
#13479=ORIENTED_EDGE('',*,*,#9625,.F.);
#13480=ORIENTED_EDGE('',*,*,#9826,.T.);
#13481=ORIENTED_EDGE('',*,*,#9623,.F.);
#13482=ORIENTED_EDGE('',*,*,#9829,.F.);
#13483=ORIENTED_EDGE('',*,*,#9331,.F.);
#13484=ORIENTED_EDGE('',*,*,#9828,.T.);
#13485=ORIENTED_EDGE('',*,*,#9328,.F.);
#13486=ORIENTED_EDGE('',*,*,#9830,.F.);
#13487=ORIENTED_EDGE('',*,*,#9620,.F.);
#13488=ORIENTED_EDGE('',*,*,#9829,.T.);
#13489=ORIENTED_EDGE('',*,*,#9622,.F.);
#13490=ORIENTED_EDGE('',*,*,#9831,.F.);
#13491=ORIENTED_EDGE('',*,*,#9326,.F.);
#13492=ORIENTED_EDGE('',*,*,#9830,.T.);
#13493=ORIENTED_EDGE('',*,*,#9327,.F.);
#13494=ORIENTED_EDGE('',*,*,#9831,.T.);
#13495=ORIENTED_EDGE('',*,*,#9621,.F.);
#13496=ORIENTED_EDGE('',*,*,#9832,.F.);
#13497=ORIENTED_EDGE('',*,*,#9336,.F.);
#13498=ORIENTED_EDGE('',*,*,#9833,.F.);
#13499=ORIENTED_EDGE('',*,*,#9630,.F.);
#13500=ORIENTED_EDGE('',*,*,#9833,.T.);
#13501=ORIENTED_EDGE('',*,*,#9335,.F.);
#13502=ORIENTED_EDGE('',*,*,#9834,.F.);
#13503=ORIENTED_EDGE('',*,*,#9631,.F.);
#13504=ORIENTED_EDGE('',*,*,#9832,.T.);
#13505=ORIENTED_EDGE('',*,*,#9629,.F.);
#13506=ORIENTED_EDGE('',*,*,#9835,.F.);
#13507=ORIENTED_EDGE('',*,*,#9337,.F.);
#13508=ORIENTED_EDGE('',*,*,#9834,.T.);
#13509=ORIENTED_EDGE('',*,*,#9334,.F.);
#13510=ORIENTED_EDGE('',*,*,#9836,.F.);
#13511=ORIENTED_EDGE('',*,*,#9626,.F.);
#13512=ORIENTED_EDGE('',*,*,#9835,.T.);
#13513=ORIENTED_EDGE('',*,*,#9628,.F.);
#13514=ORIENTED_EDGE('',*,*,#9837,.F.);
#13515=ORIENTED_EDGE('',*,*,#9332,.F.);
#13516=ORIENTED_EDGE('',*,*,#9836,.T.);
#13517=ORIENTED_EDGE('',*,*,#9333,.F.);
#13518=ORIENTED_EDGE('',*,*,#9837,.T.);
#13519=ORIENTED_EDGE('',*,*,#9627,.F.);
#13520=ORIENTED_EDGE('',*,*,#9838,.F.);
#13521=ORIENTED_EDGE('',*,*,#9342,.F.);
#13522=ORIENTED_EDGE('',*,*,#9839,.F.);
#13523=ORIENTED_EDGE('',*,*,#9636,.F.);
#13524=ORIENTED_EDGE('',*,*,#9839,.T.);
#13525=ORIENTED_EDGE('',*,*,#9341,.F.);
#13526=ORIENTED_EDGE('',*,*,#9840,.F.);
#13527=ORIENTED_EDGE('',*,*,#9637,.F.);
#13528=ORIENTED_EDGE('',*,*,#9838,.T.);
#13529=ORIENTED_EDGE('',*,*,#9635,.F.);
#13530=ORIENTED_EDGE('',*,*,#9841,.F.);
#13531=ORIENTED_EDGE('',*,*,#9343,.F.);
#13532=ORIENTED_EDGE('',*,*,#9840,.T.);
#13533=ORIENTED_EDGE('',*,*,#9340,.F.);
#13534=ORIENTED_EDGE('',*,*,#9842,.F.);
#13535=ORIENTED_EDGE('',*,*,#9632,.F.);
#13536=ORIENTED_EDGE('',*,*,#9841,.T.);
#13537=ORIENTED_EDGE('',*,*,#9634,.F.);
#13538=ORIENTED_EDGE('',*,*,#9843,.F.);
#13539=ORIENTED_EDGE('',*,*,#9338,.F.);
#13540=ORIENTED_EDGE('',*,*,#9842,.T.);
#13541=ORIENTED_EDGE('',*,*,#9339,.F.);
#13542=ORIENTED_EDGE('',*,*,#9843,.T.);
#13543=ORIENTED_EDGE('',*,*,#9633,.F.);
#13544=ORIENTED_EDGE('',*,*,#9844,.F.);
#13545=ORIENTED_EDGE('',*,*,#9348,.F.);
#13546=ORIENTED_EDGE('',*,*,#9845,.F.);
#13547=ORIENTED_EDGE('',*,*,#9642,.F.);
#13548=ORIENTED_EDGE('',*,*,#9845,.T.);
#13549=ORIENTED_EDGE('',*,*,#9347,.F.);
#13550=ORIENTED_EDGE('',*,*,#9846,.F.);
#13551=ORIENTED_EDGE('',*,*,#9643,.F.);
#13552=ORIENTED_EDGE('',*,*,#9844,.T.);
#13553=ORIENTED_EDGE('',*,*,#9641,.F.);
#13554=ORIENTED_EDGE('',*,*,#9847,.F.);
#13555=ORIENTED_EDGE('',*,*,#9349,.F.);
#13556=ORIENTED_EDGE('',*,*,#9846,.T.);
#13557=ORIENTED_EDGE('',*,*,#9346,.F.);
#13558=ORIENTED_EDGE('',*,*,#9848,.F.);
#13559=ORIENTED_EDGE('',*,*,#9638,.F.);
#13560=ORIENTED_EDGE('',*,*,#9847,.T.);
#13561=ORIENTED_EDGE('',*,*,#9640,.F.);
#13562=ORIENTED_EDGE('',*,*,#9849,.F.);
#13563=ORIENTED_EDGE('',*,*,#9344,.F.);
#13564=ORIENTED_EDGE('',*,*,#9848,.T.);
#13565=ORIENTED_EDGE('',*,*,#9345,.F.);
#13566=ORIENTED_EDGE('',*,*,#9849,.T.);
#13567=ORIENTED_EDGE('',*,*,#9639,.F.);
#13568=ORIENTED_EDGE('',*,*,#9850,.F.);
#13569=ORIENTED_EDGE('',*,*,#9354,.F.);
#13570=ORIENTED_EDGE('',*,*,#9851,.F.);
#13571=ORIENTED_EDGE('',*,*,#9648,.F.);
#13572=ORIENTED_EDGE('',*,*,#9851,.T.);
#13573=ORIENTED_EDGE('',*,*,#9353,.F.);
#13574=ORIENTED_EDGE('',*,*,#9852,.F.);
#13575=ORIENTED_EDGE('',*,*,#9649,.F.);
#13576=ORIENTED_EDGE('',*,*,#9850,.T.);
#13577=ORIENTED_EDGE('',*,*,#9647,.F.);
#13578=ORIENTED_EDGE('',*,*,#9853,.F.);
#13579=ORIENTED_EDGE('',*,*,#9355,.F.);
#13580=ORIENTED_EDGE('',*,*,#9852,.T.);
#13581=ORIENTED_EDGE('',*,*,#9352,.F.);
#13582=ORIENTED_EDGE('',*,*,#9854,.F.);
#13583=ORIENTED_EDGE('',*,*,#9644,.F.);
#13584=ORIENTED_EDGE('',*,*,#9853,.T.);
#13585=ORIENTED_EDGE('',*,*,#9646,.F.);
#13586=ORIENTED_EDGE('',*,*,#9855,.F.);
#13587=ORIENTED_EDGE('',*,*,#9350,.F.);
#13588=ORIENTED_EDGE('',*,*,#9854,.T.);
#13589=ORIENTED_EDGE('',*,*,#9351,.F.);
#13590=ORIENTED_EDGE('',*,*,#9855,.T.);
#13591=ORIENTED_EDGE('',*,*,#9645,.F.);
#13592=ORIENTED_EDGE('',*,*,#9856,.F.);
#13593=ORIENTED_EDGE('',*,*,#9360,.F.);
#13594=ORIENTED_EDGE('',*,*,#9857,.F.);
#13595=ORIENTED_EDGE('',*,*,#9654,.F.);
#13596=ORIENTED_EDGE('',*,*,#9857,.T.);
#13597=ORIENTED_EDGE('',*,*,#9359,.F.);
#13598=ORIENTED_EDGE('',*,*,#9858,.F.);
#13599=ORIENTED_EDGE('',*,*,#9655,.F.);
#13600=ORIENTED_EDGE('',*,*,#9856,.T.);
#13601=ORIENTED_EDGE('',*,*,#9653,.F.);
#13602=ORIENTED_EDGE('',*,*,#9859,.F.);
#13603=ORIENTED_EDGE('',*,*,#9361,.F.);
#13604=ORIENTED_EDGE('',*,*,#9858,.T.);
#13605=ORIENTED_EDGE('',*,*,#9358,.F.);
#13606=ORIENTED_EDGE('',*,*,#9860,.F.);
#13607=ORIENTED_EDGE('',*,*,#9650,.F.);
#13608=ORIENTED_EDGE('',*,*,#9859,.T.);
#13609=ORIENTED_EDGE('',*,*,#9652,.F.);
#13610=ORIENTED_EDGE('',*,*,#9861,.F.);
#13611=ORIENTED_EDGE('',*,*,#9356,.F.);
#13612=ORIENTED_EDGE('',*,*,#9860,.T.);
#13613=ORIENTED_EDGE('',*,*,#9357,.F.);
#13614=ORIENTED_EDGE('',*,*,#9861,.T.);
#13615=ORIENTED_EDGE('',*,*,#9651,.F.);
#13616=ORIENTED_EDGE('',*,*,#9862,.F.);
#13617=ORIENTED_EDGE('',*,*,#9369,.F.);
#13618=ORIENTED_EDGE('',*,*,#9368,.F.);
#13619=ORIENTED_EDGE('',*,*,#9863,.F.);
#13620=ORIENTED_EDGE('',*,*,#9660,.F.);
#13621=ORIENTED_EDGE('',*,*,#9863,.T.);
#13622=ORIENTED_EDGE('',*,*,#9367,.F.);
#13623=ORIENTED_EDGE('',*,*,#9864,.F.);
#13624=ORIENTED_EDGE('',*,*,#9661,.F.);
#13625=ORIENTED_EDGE('',*,*,#9862,.T.);
#13626=ORIENTED_EDGE('',*,*,#9659,.F.);
#13627=ORIENTED_EDGE('',*,*,#9865,.F.);
#13628=ORIENTED_EDGE('',*,*,#9371,.F.);
#13629=ORIENTED_EDGE('',*,*,#9370,.F.);
#13630=ORIENTED_EDGE('',*,*,#9864,.T.);
#13631=ORIENTED_EDGE('',*,*,#9366,.F.);
#13632=ORIENTED_EDGE('',*,*,#9365,.F.);
#13633=ORIENTED_EDGE('',*,*,#9866,.F.);
#13634=ORIENTED_EDGE('',*,*,#9656,.F.);
#13635=ORIENTED_EDGE('',*,*,#9865,.T.);
#13636=ORIENTED_EDGE('',*,*,#9658,.F.);
#13637=ORIENTED_EDGE('',*,*,#9867,.F.);
#13638=ORIENTED_EDGE('',*,*,#9362,.F.);
#13639=ORIENTED_EDGE('',*,*,#9866,.T.);
#13640=ORIENTED_EDGE('',*,*,#9364,.F.);
#13641=ORIENTED_EDGE('',*,*,#9363,.F.);
#13642=ORIENTED_EDGE('',*,*,#9867,.T.);
#13643=ORIENTED_EDGE('',*,*,#9657,.F.);
#13644=ORIENTED_EDGE('',*,*,#9868,.F.);
#13645=ORIENTED_EDGE('',*,*,#9376,.F.);
#13646=ORIENTED_EDGE('',*,*,#9869,.F.);
#13647=ORIENTED_EDGE('',*,*,#9666,.F.);
#13648=ORIENTED_EDGE('',*,*,#9869,.T.);
#13649=ORIENTED_EDGE('',*,*,#9375,.F.);
#13650=ORIENTED_EDGE('',*,*,#9870,.F.);
#13651=ORIENTED_EDGE('',*,*,#9667,.F.);
#13652=ORIENTED_EDGE('',*,*,#9868,.T.);
#13653=ORIENTED_EDGE('',*,*,#9665,.F.);
#13654=ORIENTED_EDGE('',*,*,#9871,.F.);
#13655=ORIENTED_EDGE('',*,*,#9377,.F.);
#13656=ORIENTED_EDGE('',*,*,#9870,.T.);
#13657=ORIENTED_EDGE('',*,*,#9374,.F.);
#13658=ORIENTED_EDGE('',*,*,#9872,.F.);
#13659=ORIENTED_EDGE('',*,*,#9662,.F.);
#13660=ORIENTED_EDGE('',*,*,#9871,.T.);
#13661=ORIENTED_EDGE('',*,*,#9664,.F.);
#13662=ORIENTED_EDGE('',*,*,#9873,.F.);
#13663=ORIENTED_EDGE('',*,*,#9372,.F.);
#13664=ORIENTED_EDGE('',*,*,#9872,.T.);
#13665=ORIENTED_EDGE('',*,*,#9373,.F.);
#13666=ORIENTED_EDGE('',*,*,#9873,.T.);
#13667=ORIENTED_EDGE('',*,*,#9663,.F.);
#13668=ORIENTED_EDGE('',*,*,#9874,.F.);
#13669=ORIENTED_EDGE('',*,*,#9382,.F.);
#13670=ORIENTED_EDGE('',*,*,#9875,.F.);
#13671=ORIENTED_EDGE('',*,*,#9672,.F.);
#13672=ORIENTED_EDGE('',*,*,#9875,.T.);
#13673=ORIENTED_EDGE('',*,*,#9381,.F.);
#13674=ORIENTED_EDGE('',*,*,#9876,.F.);
#13675=ORIENTED_EDGE('',*,*,#9673,.F.);
#13676=ORIENTED_EDGE('',*,*,#9874,.T.);
#13677=ORIENTED_EDGE('',*,*,#9671,.F.);
#13678=ORIENTED_EDGE('',*,*,#9877,.F.);
#13679=ORIENTED_EDGE('',*,*,#9383,.F.);
#13680=ORIENTED_EDGE('',*,*,#9876,.T.);
#13681=ORIENTED_EDGE('',*,*,#9380,.F.);
#13682=ORIENTED_EDGE('',*,*,#9878,.F.);
#13683=ORIENTED_EDGE('',*,*,#9668,.F.);
#13684=ORIENTED_EDGE('',*,*,#9877,.T.);
#13685=ORIENTED_EDGE('',*,*,#9670,.F.);
#13686=ORIENTED_EDGE('',*,*,#9879,.F.);
#13687=ORIENTED_EDGE('',*,*,#9378,.F.);
#13688=ORIENTED_EDGE('',*,*,#9878,.T.);
#13689=ORIENTED_EDGE('',*,*,#9379,.F.);
#13690=ORIENTED_EDGE('',*,*,#9879,.T.);
#13691=ORIENTED_EDGE('',*,*,#9669,.F.);
#13692=ORIENTED_EDGE('',*,*,#9880,.F.);
#13693=ORIENTED_EDGE('',*,*,#9388,.F.);
#13694=ORIENTED_EDGE('',*,*,#9881,.F.);
#13695=ORIENTED_EDGE('',*,*,#9678,.F.);
#13696=ORIENTED_EDGE('',*,*,#9881,.T.);
#13697=ORIENTED_EDGE('',*,*,#9387,.F.);
#13698=ORIENTED_EDGE('',*,*,#9882,.F.);
#13699=ORIENTED_EDGE('',*,*,#9679,.F.);
#13700=ORIENTED_EDGE('',*,*,#9880,.T.);
#13701=ORIENTED_EDGE('',*,*,#9677,.F.);
#13702=ORIENTED_EDGE('',*,*,#9883,.F.);
#13703=ORIENTED_EDGE('',*,*,#9389,.F.);
#13704=ORIENTED_EDGE('',*,*,#9882,.T.);
#13705=ORIENTED_EDGE('',*,*,#9386,.F.);
#13706=ORIENTED_EDGE('',*,*,#9884,.F.);
#13707=ORIENTED_EDGE('',*,*,#9674,.F.);
#13708=ORIENTED_EDGE('',*,*,#9883,.T.);
#13709=ORIENTED_EDGE('',*,*,#9676,.F.);
#13710=ORIENTED_EDGE('',*,*,#9885,.F.);
#13711=ORIENTED_EDGE('',*,*,#9384,.F.);
#13712=ORIENTED_EDGE('',*,*,#9884,.T.);
#13713=ORIENTED_EDGE('',*,*,#9385,.F.);
#13714=ORIENTED_EDGE('',*,*,#9885,.T.);
#13715=ORIENTED_EDGE('',*,*,#9675,.F.);
#13716=ORIENTED_EDGE('',*,*,#9886,.F.);
#13717=ORIENTED_EDGE('',*,*,#9394,.F.);
#13718=ORIENTED_EDGE('',*,*,#9887,.F.);
#13719=ORIENTED_EDGE('',*,*,#9684,.F.);
#13720=ORIENTED_EDGE('',*,*,#9887,.T.);
#13721=ORIENTED_EDGE('',*,*,#9393,.F.);
#13722=ORIENTED_EDGE('',*,*,#9888,.F.);
#13723=ORIENTED_EDGE('',*,*,#9685,.F.);
#13724=ORIENTED_EDGE('',*,*,#9886,.T.);
#13725=ORIENTED_EDGE('',*,*,#9683,.F.);
#13726=ORIENTED_EDGE('',*,*,#9889,.F.);
#13727=ORIENTED_EDGE('',*,*,#9395,.F.);
#13728=ORIENTED_EDGE('',*,*,#9888,.T.);
#13729=ORIENTED_EDGE('',*,*,#9392,.F.);
#13730=ORIENTED_EDGE('',*,*,#9890,.F.);
#13731=ORIENTED_EDGE('',*,*,#9680,.F.);
#13732=ORIENTED_EDGE('',*,*,#9889,.T.);
#13733=ORIENTED_EDGE('',*,*,#9682,.F.);
#13734=ORIENTED_EDGE('',*,*,#9891,.F.);
#13735=ORIENTED_EDGE('',*,*,#9390,.F.);
#13736=ORIENTED_EDGE('',*,*,#9890,.T.);
#13737=ORIENTED_EDGE('',*,*,#9391,.F.);
#13738=ORIENTED_EDGE('',*,*,#9891,.T.);
#13739=ORIENTED_EDGE('',*,*,#9681,.F.);
#13740=ORIENTED_EDGE('',*,*,#9892,.F.);
#13741=ORIENTED_EDGE('',*,*,#9400,.F.);
#13742=ORIENTED_EDGE('',*,*,#9893,.F.);
#13743=ORIENTED_EDGE('',*,*,#9690,.F.);
#13744=ORIENTED_EDGE('',*,*,#9893,.T.);
#13745=ORIENTED_EDGE('',*,*,#9399,.F.);
#13746=ORIENTED_EDGE('',*,*,#9894,.F.);
#13747=ORIENTED_EDGE('',*,*,#9691,.F.);
#13748=ORIENTED_EDGE('',*,*,#9892,.T.);
#13749=ORIENTED_EDGE('',*,*,#9689,.F.);
#13750=ORIENTED_EDGE('',*,*,#9895,.F.);
#13751=ORIENTED_EDGE('',*,*,#9401,.F.);
#13752=ORIENTED_EDGE('',*,*,#9894,.T.);
#13753=ORIENTED_EDGE('',*,*,#9398,.F.);
#13754=ORIENTED_EDGE('',*,*,#9896,.F.);
#13755=ORIENTED_EDGE('',*,*,#9686,.F.);
#13756=ORIENTED_EDGE('',*,*,#9895,.T.);
#13757=ORIENTED_EDGE('',*,*,#9688,.F.);
#13758=ORIENTED_EDGE('',*,*,#9897,.F.);
#13759=ORIENTED_EDGE('',*,*,#9396,.F.);
#13760=ORIENTED_EDGE('',*,*,#9896,.T.);
#13761=ORIENTED_EDGE('',*,*,#9397,.F.);
#13762=ORIENTED_EDGE('',*,*,#9897,.T.);
#13763=ORIENTED_EDGE('',*,*,#9687,.F.);
#13764=ORIENTED_EDGE('',*,*,#9898,.F.);
#13765=ORIENTED_EDGE('',*,*,#9409,.F.);
#13766=ORIENTED_EDGE('',*,*,#9408,.F.);
#13767=ORIENTED_EDGE('',*,*,#9899,.F.);
#13768=ORIENTED_EDGE('',*,*,#9696,.F.);
#13769=ORIENTED_EDGE('',*,*,#9899,.T.);
#13770=ORIENTED_EDGE('',*,*,#9407,.F.);
#13771=ORIENTED_EDGE('',*,*,#9900,.F.);
#13772=ORIENTED_EDGE('',*,*,#9697,.F.);
#13773=ORIENTED_EDGE('',*,*,#9898,.T.);
#13774=ORIENTED_EDGE('',*,*,#9695,.F.);
#13775=ORIENTED_EDGE('',*,*,#9901,.F.);
#13776=ORIENTED_EDGE('',*,*,#9411,.F.);
#13777=ORIENTED_EDGE('',*,*,#9410,.F.);
#13778=ORIENTED_EDGE('',*,*,#9900,.T.);
#13779=ORIENTED_EDGE('',*,*,#9406,.F.);
#13780=ORIENTED_EDGE('',*,*,#9405,.F.);
#13781=ORIENTED_EDGE('',*,*,#9902,.F.);
#13782=ORIENTED_EDGE('',*,*,#9692,.F.);
#13783=ORIENTED_EDGE('',*,*,#9901,.T.);
#13784=ORIENTED_EDGE('',*,*,#9694,.F.);
#13785=ORIENTED_EDGE('',*,*,#9903,.F.);
#13786=ORIENTED_EDGE('',*,*,#9402,.F.);
#13787=ORIENTED_EDGE('',*,*,#9902,.T.);
#13788=ORIENTED_EDGE('',*,*,#9404,.F.);
#13789=ORIENTED_EDGE('',*,*,#9403,.F.);
#13790=ORIENTED_EDGE('',*,*,#9903,.T.);
#13791=ORIENTED_EDGE('',*,*,#9693,.F.);
#13792=ORIENTED_EDGE('',*,*,#9904,.F.);
#13793=ORIENTED_EDGE('',*,*,#9419,.F.);
#13794=ORIENTED_EDGE('',*,*,#9418,.F.);
#13795=ORIENTED_EDGE('',*,*,#9905,.F.);
#13796=ORIENTED_EDGE('',*,*,#9702,.F.);
#13797=ORIENTED_EDGE('',*,*,#9905,.T.);
#13798=ORIENTED_EDGE('',*,*,#9417,.F.);
#13799=ORIENTED_EDGE('',*,*,#9906,.F.);
#13800=ORIENTED_EDGE('',*,*,#9703,.F.);
#13801=ORIENTED_EDGE('',*,*,#9904,.T.);
#13802=ORIENTED_EDGE('',*,*,#9701,.F.);
#13803=ORIENTED_EDGE('',*,*,#9907,.F.);
#13804=ORIENTED_EDGE('',*,*,#9421,.F.);
#13805=ORIENTED_EDGE('',*,*,#9420,.F.);
#13806=ORIENTED_EDGE('',*,*,#9906,.T.);
#13807=ORIENTED_EDGE('',*,*,#9416,.F.);
#13808=ORIENTED_EDGE('',*,*,#9415,.F.);
#13809=ORIENTED_EDGE('',*,*,#9908,.F.);
#13810=ORIENTED_EDGE('',*,*,#9698,.F.);
#13811=ORIENTED_EDGE('',*,*,#9907,.T.);
#13812=ORIENTED_EDGE('',*,*,#9700,.F.);
#13813=ORIENTED_EDGE('',*,*,#9909,.F.);
#13814=ORIENTED_EDGE('',*,*,#9412,.F.);
#13815=ORIENTED_EDGE('',*,*,#9908,.T.);
#13816=ORIENTED_EDGE('',*,*,#9414,.F.);
#13817=ORIENTED_EDGE('',*,*,#9413,.F.);
#13818=ORIENTED_EDGE('',*,*,#9909,.T.);
#13819=ORIENTED_EDGE('',*,*,#9699,.F.);
#13820=ORIENTED_EDGE('',*,*,#9910,.F.);
#13821=ORIENTED_EDGE('',*,*,#9429,.F.);
#13822=ORIENTED_EDGE('',*,*,#9911,.F.);
#13823=ORIENTED_EDGE('',*,*,#9708,.F.);
#13824=ORIENTED_EDGE('',*,*,#9911,.T.);
#13825=ORIENTED_EDGE('',*,*,#9428,.F.);
#13826=ORIENTED_EDGE('',*,*,#9912,.F.);
#13827=ORIENTED_EDGE('',*,*,#9709,.F.);
#13828=ORIENTED_EDGE('',*,*,#9910,.T.);
#13829=ORIENTED_EDGE('',*,*,#9707,.F.);
#13830=ORIENTED_EDGE('',*,*,#9913,.F.);
#13831=ORIENTED_EDGE('',*,*,#9433,.F.);
#13832=ORIENTED_EDGE('',*,*,#9432,.F.);
#13833=ORIENTED_EDGE('',*,*,#9431,.F.);
#13834=ORIENTED_EDGE('',*,*,#9430,.F.);
#13835=ORIENTED_EDGE('',*,*,#9912,.T.);
#13836=ORIENTED_EDGE('',*,*,#9427,.F.);
#13837=ORIENTED_EDGE('',*,*,#9426,.F.);
#13838=ORIENTED_EDGE('',*,*,#9914,.F.);
#13839=ORIENTED_EDGE('',*,*,#9704,.F.);
#13840=ORIENTED_EDGE('',*,*,#9913,.T.);
#13841=ORIENTED_EDGE('',*,*,#9706,.F.);
#13842=ORIENTED_EDGE('',*,*,#9915,.F.);
#13843=ORIENTED_EDGE('',*,*,#9423,.F.);
#13844=ORIENTED_EDGE('',*,*,#9422,.F.);
#13845=ORIENTED_EDGE('',*,*,#9914,.T.);
#13846=ORIENTED_EDGE('',*,*,#9425,.F.);
#13847=ORIENTED_EDGE('',*,*,#9424,.F.);
#13848=ORIENTED_EDGE('',*,*,#9915,.T.);
#13849=ORIENTED_EDGE('',*,*,#9705,.F.);
#13850=ORIENTED_EDGE('',*,*,#9916,.F.);
#13851=ORIENTED_EDGE('',*,*,#9439,.F.);
#13852=ORIENTED_EDGE('',*,*,#9438,.F.);
#13853=ORIENTED_EDGE('',*,*,#9917,.F.);
#13854=ORIENTED_EDGE('',*,*,#9714,.F.);
#13855=ORIENTED_EDGE('',*,*,#9917,.T.);
#13856=ORIENTED_EDGE('',*,*,#9437,.F.);
#13857=ORIENTED_EDGE('',*,*,#9918,.F.);
#13858=ORIENTED_EDGE('',*,*,#9715,.F.);
#13859=ORIENTED_EDGE('',*,*,#9916,.T.);
#13860=ORIENTED_EDGE('',*,*,#9713,.F.);
#13861=ORIENTED_EDGE('',*,*,#9919,.F.);
#13862=ORIENTED_EDGE('',*,*,#9441,.F.);
#13863=ORIENTED_EDGE('',*,*,#9440,.F.);
#13864=ORIENTED_EDGE('',*,*,#9918,.T.);
#13865=ORIENTED_EDGE('',*,*,#9436,.F.);
#13866=ORIENTED_EDGE('',*,*,#9920,.F.);
#13867=ORIENTED_EDGE('',*,*,#9710,.F.);
#13868=ORIENTED_EDGE('',*,*,#9919,.T.);
#13869=ORIENTED_EDGE('',*,*,#9712,.F.);
#13870=ORIENTED_EDGE('',*,*,#9921,.F.);
#13871=ORIENTED_EDGE('',*,*,#9434,.F.);
#13872=ORIENTED_EDGE('',*,*,#9920,.T.);
#13873=ORIENTED_EDGE('',*,*,#9435,.F.);
#13874=ORIENTED_EDGE('',*,*,#9921,.T.);
#13875=ORIENTED_EDGE('',*,*,#9711,.F.);
#13876=ORIENTED_EDGE('',*,*,#9922,.F.);
#13877=ORIENTED_EDGE('',*,*,#9451,.F.);
#13878=ORIENTED_EDGE('',*,*,#9450,.F.);
#13879=ORIENTED_EDGE('',*,*,#9923,.F.);
#13880=ORIENTED_EDGE('',*,*,#9720,.F.);
#13881=ORIENTED_EDGE('',*,*,#9923,.T.);
#13882=ORIENTED_EDGE('',*,*,#9449,.F.);
#13883=ORIENTED_EDGE('',*,*,#9924,.F.);
#13884=ORIENTED_EDGE('',*,*,#9721,.F.);
#13885=ORIENTED_EDGE('',*,*,#9922,.T.);
#13886=ORIENTED_EDGE('',*,*,#9719,.F.);
#13887=ORIENTED_EDGE('',*,*,#9925,.F.);
#13888=ORIENTED_EDGE('',*,*,#9452,.F.);
#13889=ORIENTED_EDGE('',*,*,#9924,.T.);
#13890=ORIENTED_EDGE('',*,*,#9448,.F.);
#13891=ORIENTED_EDGE('',*,*,#9447,.F.);
#13892=ORIENTED_EDGE('',*,*,#9446,.F.);
#13893=ORIENTED_EDGE('',*,*,#9445,.F.);
#13894=ORIENTED_EDGE('',*,*,#9926,.F.);
#13895=ORIENTED_EDGE('',*,*,#9716,.F.);
#13896=ORIENTED_EDGE('',*,*,#9925,.T.);
#13897=ORIENTED_EDGE('',*,*,#9718,.F.);
#13898=ORIENTED_EDGE('',*,*,#9927,.F.);
#13899=ORIENTED_EDGE('',*,*,#9442,.F.);
#13900=ORIENTED_EDGE('',*,*,#9926,.T.);
#13901=ORIENTED_EDGE('',*,*,#9444,.F.);
#13902=ORIENTED_EDGE('',*,*,#9443,.F.);
#13903=ORIENTED_EDGE('',*,*,#9927,.T.);
#13904=ORIENTED_EDGE('',*,*,#9717,.F.);
#13905=ORIENTED_EDGE('',*,*,#9928,.F.);
#13906=ORIENTED_EDGE('',*,*,#9246,.F.);
#13907=ORIENTED_EDGE('',*,*,#9112,.F.);
#13908=ORIENTED_EDGE('',*,*,#9929,.F.);
#13909=ORIENTED_EDGE('',*,*,#9724,.T.);
#13910=ORIENTED_EDGE('',*,*,#9929,.T.);
#13911=ORIENTED_EDGE('',*,*,#9111,.F.);
#13912=ORIENTED_EDGE('',*,*,#9930,.F.);
#13913=ORIENTED_EDGE('',*,*,#9725,.T.);
#13914=ORIENTED_EDGE('',*,*,#9928,.T.);
#13915=ORIENTED_EDGE('',*,*,#9729,.T.);
#13916=ORIENTED_EDGE('',*,*,#9931,.F.);
#13917=ORIENTED_EDGE('',*,*,#9247,.F.);
#13918=ORIENTED_EDGE('',*,*,#9930,.T.);
#13919=ORIENTED_EDGE('',*,*,#9110,.F.);
#13920=ORIENTED_EDGE('',*,*,#9932,.F.);
#13921=ORIENTED_EDGE('',*,*,#9726,.T.);
#13922=ORIENTED_EDGE('',*,*,#9931,.T.);
#13923=ORIENTED_EDGE('',*,*,#9728,.T.);
#13924=ORIENTED_EDGE('',*,*,#9933,.F.);
#13925=ORIENTED_EDGE('',*,*,#9108,.F.);
#13926=ORIENTED_EDGE('',*,*,#9248,.F.);
#13927=ORIENTED_EDGE('',*,*,#9932,.T.);
#13928=ORIENTED_EDGE('',*,*,#9109,.F.);
#13929=ORIENTED_EDGE('',*,*,#9933,.T.);
#13930=ORIENTED_EDGE('',*,*,#9727,.T.);
#13931=ORIENTED_EDGE('',*,*,#9934,.F.);
#13932=ORIENTED_EDGE('',*,*,#9249,.F.);
#13933=ORIENTED_EDGE('',*,*,#9106,.F.);
#13934=ORIENTED_EDGE('',*,*,#9935,.F.);
#13935=ORIENTED_EDGE('',*,*,#9730,.T.);
#13936=ORIENTED_EDGE('',*,*,#9935,.T.);
#13937=ORIENTED_EDGE('',*,*,#9105,.F.);
#13938=ORIENTED_EDGE('',*,*,#9936,.F.);
#13939=ORIENTED_EDGE('',*,*,#9731,.T.);
#13940=ORIENTED_EDGE('',*,*,#9934,.T.);
#13941=ORIENTED_EDGE('',*,*,#9735,.T.);
#13942=ORIENTED_EDGE('',*,*,#9937,.F.);
#13943=ORIENTED_EDGE('',*,*,#9250,.F.);
#13944=ORIENTED_EDGE('',*,*,#9936,.T.);
#13945=ORIENTED_EDGE('',*,*,#9104,.F.);
#13946=ORIENTED_EDGE('',*,*,#9938,.F.);
#13947=ORIENTED_EDGE('',*,*,#9732,.T.);
#13948=ORIENTED_EDGE('',*,*,#9937,.T.);
#13949=ORIENTED_EDGE('',*,*,#9734,.T.);
#13950=ORIENTED_EDGE('',*,*,#9939,.F.);
#13951=ORIENTED_EDGE('',*,*,#9102,.F.);
#13952=ORIENTED_EDGE('',*,*,#9251,.F.);
#13953=ORIENTED_EDGE('',*,*,#9938,.T.);
#13954=ORIENTED_EDGE('',*,*,#9103,.F.);
#13955=ORIENTED_EDGE('',*,*,#9939,.T.);
#13956=ORIENTED_EDGE('',*,*,#9733,.T.);
#13957=ORIENTED_EDGE('',*,*,#9940,.F.);
#13958=ORIENTED_EDGE('',*,*,#9252,.F.);
#13959=ORIENTED_EDGE('',*,*,#9100,.F.);
#13960=ORIENTED_EDGE('',*,*,#9941,.F.);
#13961=ORIENTED_EDGE('',*,*,#9736,.T.);
#13962=ORIENTED_EDGE('',*,*,#9941,.T.);
#13963=ORIENTED_EDGE('',*,*,#9099,.F.);
#13964=ORIENTED_EDGE('',*,*,#9942,.F.);
#13965=ORIENTED_EDGE('',*,*,#9737,.T.);
#13966=ORIENTED_EDGE('',*,*,#9940,.T.);
#13967=ORIENTED_EDGE('',*,*,#9741,.T.);
#13968=ORIENTED_EDGE('',*,*,#9943,.F.);
#13969=ORIENTED_EDGE('',*,*,#9253,.F.);
#13970=ORIENTED_EDGE('',*,*,#9942,.T.);
#13971=ORIENTED_EDGE('',*,*,#9098,.F.);
#13972=ORIENTED_EDGE('',*,*,#9944,.F.);
#13973=ORIENTED_EDGE('',*,*,#9738,.T.);
#13974=ORIENTED_EDGE('',*,*,#9943,.T.);
#13975=ORIENTED_EDGE('',*,*,#9740,.T.);
#13976=ORIENTED_EDGE('',*,*,#9945,.F.);
#13977=ORIENTED_EDGE('',*,*,#9096,.F.);
#13978=ORIENTED_EDGE('',*,*,#9254,.F.);
#13979=ORIENTED_EDGE('',*,*,#9944,.T.);
#13980=ORIENTED_EDGE('',*,*,#9097,.F.);
#13981=ORIENTED_EDGE('',*,*,#9945,.T.);
#13982=ORIENTED_EDGE('',*,*,#9739,.T.);
#13983=ORIENTED_EDGE('',*,*,#9946,.F.);
#13984=ORIENTED_EDGE('',*,*,#9255,.F.);
#13985=ORIENTED_EDGE('',*,*,#9094,.F.);
#13986=ORIENTED_EDGE('',*,*,#9947,.F.);
#13987=ORIENTED_EDGE('',*,*,#9742,.T.);
#13988=ORIENTED_EDGE('',*,*,#9947,.T.);
#13989=ORIENTED_EDGE('',*,*,#9093,.F.);
#13990=ORIENTED_EDGE('',*,*,#9948,.F.);
#13991=ORIENTED_EDGE('',*,*,#9743,.T.);
#13992=ORIENTED_EDGE('',*,*,#9946,.T.);
#13993=ORIENTED_EDGE('',*,*,#9747,.T.);
#13994=ORIENTED_EDGE('',*,*,#9949,.F.);
#13995=ORIENTED_EDGE('',*,*,#9256,.F.);
#13996=ORIENTED_EDGE('',*,*,#9948,.T.);
#13997=ORIENTED_EDGE('',*,*,#9092,.F.);
#13998=ORIENTED_EDGE('',*,*,#9950,.F.);
#13999=ORIENTED_EDGE('',*,*,#9744,.T.);
#14000=ORIENTED_EDGE('',*,*,#9949,.T.);
#14001=ORIENTED_EDGE('',*,*,#9746,.T.);
#14002=ORIENTED_EDGE('',*,*,#9951,.F.);
#14003=ORIENTED_EDGE('',*,*,#9090,.F.);
#14004=ORIENTED_EDGE('',*,*,#9257,.F.);
#14005=ORIENTED_EDGE('',*,*,#9950,.T.);
#14006=ORIENTED_EDGE('',*,*,#9091,.F.);
#14007=ORIENTED_EDGE('',*,*,#9951,.T.);
#14008=ORIENTED_EDGE('',*,*,#9745,.T.);
#14009=ORIENTED_EDGE('',*,*,#9952,.F.);
#14010=ORIENTED_EDGE('',*,*,#9231,.F.);
#14011=ORIENTED_EDGE('',*,*,#9142,.F.);
#14012=ORIENTED_EDGE('',*,*,#9953,.F.);
#14013=ORIENTED_EDGE('',*,*,#9748,.T.);
#14014=ORIENTED_EDGE('',*,*,#9953,.T.);
#14015=ORIENTED_EDGE('',*,*,#9141,.F.);
#14016=ORIENTED_EDGE('',*,*,#9954,.F.);
#14017=ORIENTED_EDGE('',*,*,#9749,.T.);
#14018=ORIENTED_EDGE('',*,*,#9952,.T.);
#14019=ORIENTED_EDGE('',*,*,#9753,.T.);
#14020=ORIENTED_EDGE('',*,*,#9955,.F.);
#14021=ORIENTED_EDGE('',*,*,#9232,.F.);
#14022=ORIENTED_EDGE('',*,*,#9954,.T.);
#14023=ORIENTED_EDGE('',*,*,#9140,.F.);
#14024=ORIENTED_EDGE('',*,*,#9956,.F.);
#14025=ORIENTED_EDGE('',*,*,#9750,.T.);
#14026=ORIENTED_EDGE('',*,*,#9955,.T.);
#14027=ORIENTED_EDGE('',*,*,#9752,.T.);
#14028=ORIENTED_EDGE('',*,*,#9957,.F.);
#14029=ORIENTED_EDGE('',*,*,#9138,.F.);
#14030=ORIENTED_EDGE('',*,*,#9233,.F.);
#14031=ORIENTED_EDGE('',*,*,#9956,.T.);
#14032=ORIENTED_EDGE('',*,*,#9139,.F.);
#14033=ORIENTED_EDGE('',*,*,#9957,.T.);
#14034=ORIENTED_EDGE('',*,*,#9751,.T.);
#14035=ORIENTED_EDGE('',*,*,#9958,.F.);
#14036=ORIENTED_EDGE('',*,*,#9261,.F.);
#14037=ORIENTED_EDGE('',*,*,#9082,.F.);
#14038=ORIENTED_EDGE('',*,*,#9959,.F.);
#14039=ORIENTED_EDGE('',*,*,#9754,.T.);
#14040=ORIENTED_EDGE('',*,*,#9959,.T.);
#14041=ORIENTED_EDGE('',*,*,#9081,.F.);
#14042=ORIENTED_EDGE('',*,*,#9960,.F.);
#14043=ORIENTED_EDGE('',*,*,#9755,.T.);
#14044=ORIENTED_EDGE('',*,*,#9958,.T.);
#14045=ORIENTED_EDGE('',*,*,#9759,.T.);
#14046=ORIENTED_EDGE('',*,*,#9961,.F.);
#14047=ORIENTED_EDGE('',*,*,#9262,.F.);
#14048=ORIENTED_EDGE('',*,*,#9960,.T.);
#14049=ORIENTED_EDGE('',*,*,#9080,.F.);
#14050=ORIENTED_EDGE('',*,*,#9962,.F.);
#14051=ORIENTED_EDGE('',*,*,#9756,.T.);
#14052=ORIENTED_EDGE('',*,*,#9961,.T.);
#14053=ORIENTED_EDGE('',*,*,#9758,.T.);
#14054=ORIENTED_EDGE('',*,*,#9963,.F.);
#14055=ORIENTED_EDGE('',*,*,#9078,.F.);
#14056=ORIENTED_EDGE('',*,*,#9263,.F.);
#14057=ORIENTED_EDGE('',*,*,#9962,.T.);
#14058=ORIENTED_EDGE('',*,*,#9079,.F.);
#14059=ORIENTED_EDGE('',*,*,#9963,.T.);
#14060=ORIENTED_EDGE('',*,*,#9757,.T.);
#14061=ORIENTED_EDGE('',*,*,#9964,.F.);
#14062=ORIENTED_EDGE('',*,*,#9284,.F.);
#14063=ORIENTED_EDGE('',*,*,#9283,.F.);
#14064=ORIENTED_EDGE('',*,*,#9042,.F.);
#14065=ORIENTED_EDGE('',*,*,#9965,.F.);
#14066=ORIENTED_EDGE('',*,*,#9760,.T.);
#14067=ORIENTED_EDGE('',*,*,#9965,.T.);
#14068=ORIENTED_EDGE('',*,*,#9041,.F.);
#14069=ORIENTED_EDGE('',*,*,#9040,.F.);
#14070=ORIENTED_EDGE('',*,*,#9966,.F.);
#14071=ORIENTED_EDGE('',*,*,#9761,.T.);
#14072=ORIENTED_EDGE('',*,*,#9964,.T.);
#14073=ORIENTED_EDGE('',*,*,#9765,.T.);
#14074=ORIENTED_EDGE('',*,*,#9967,.F.);
#14075=ORIENTED_EDGE('',*,*,#9285,.F.);
#14076=ORIENTED_EDGE('',*,*,#9966,.T.);
#14077=ORIENTED_EDGE('',*,*,#9039,.F.);
#14078=ORIENTED_EDGE('',*,*,#9968,.F.);
#14079=ORIENTED_EDGE('',*,*,#9762,.T.);
#14080=ORIENTED_EDGE('',*,*,#9967,.T.);
#14081=ORIENTED_EDGE('',*,*,#9764,.T.);
#14082=ORIENTED_EDGE('',*,*,#9969,.F.);
#14083=ORIENTED_EDGE('',*,*,#9036,.F.);
#14084=ORIENTED_EDGE('',*,*,#9287,.F.);
#14085=ORIENTED_EDGE('',*,*,#9286,.F.);
#14086=ORIENTED_EDGE('',*,*,#9968,.T.);
#14087=ORIENTED_EDGE('',*,*,#9038,.F.);
#14088=ORIENTED_EDGE('',*,*,#9037,.F.);
#14089=ORIENTED_EDGE('',*,*,#9969,.T.);
#14090=ORIENTED_EDGE('',*,*,#9763,.T.);
#14091=ORIENTED_EDGE('',*,*,#9970,.F.);
#14092=ORIENTED_EDGE('',*,*,#9258,.F.);
#14093=ORIENTED_EDGE('',*,*,#9088,.F.);
#14094=ORIENTED_EDGE('',*,*,#9971,.F.);
#14095=ORIENTED_EDGE('',*,*,#9766,.T.);
#14096=ORIENTED_EDGE('',*,*,#9971,.T.);
#14097=ORIENTED_EDGE('',*,*,#9087,.F.);
#14098=ORIENTED_EDGE('',*,*,#9972,.F.);
#14099=ORIENTED_EDGE('',*,*,#9767,.T.);
#14100=ORIENTED_EDGE('',*,*,#9970,.T.);
#14101=ORIENTED_EDGE('',*,*,#9771,.T.);
#14102=ORIENTED_EDGE('',*,*,#9973,.F.);
#14103=ORIENTED_EDGE('',*,*,#9259,.F.);
#14104=ORIENTED_EDGE('',*,*,#9972,.T.);
#14105=ORIENTED_EDGE('',*,*,#9086,.F.);
#14106=ORIENTED_EDGE('',*,*,#9974,.F.);
#14107=ORIENTED_EDGE('',*,*,#9768,.T.);
#14108=ORIENTED_EDGE('',*,*,#9973,.T.);
#14109=ORIENTED_EDGE('',*,*,#9770,.T.);
#14110=ORIENTED_EDGE('',*,*,#9975,.F.);
#14111=ORIENTED_EDGE('',*,*,#9084,.F.);
#14112=ORIENTED_EDGE('',*,*,#9260,.F.);
#14113=ORIENTED_EDGE('',*,*,#9974,.T.);
#14114=ORIENTED_EDGE('',*,*,#9085,.F.);
#14115=ORIENTED_EDGE('',*,*,#9975,.T.);
#14116=ORIENTED_EDGE('',*,*,#9769,.T.);
#14117=ORIENTED_EDGE('',*,*,#9976,.F.);
#14118=ORIENTED_EDGE('',*,*,#9243,.F.);
#14119=ORIENTED_EDGE('',*,*,#9118,.F.);
#14120=ORIENTED_EDGE('',*,*,#9977,.F.);
#14121=ORIENTED_EDGE('',*,*,#9772,.T.);
#14122=ORIENTED_EDGE('',*,*,#9977,.T.);
#14123=ORIENTED_EDGE('',*,*,#9117,.F.);
#14124=ORIENTED_EDGE('',*,*,#9978,.F.);
#14125=ORIENTED_EDGE('',*,*,#9773,.T.);
#14126=ORIENTED_EDGE('',*,*,#9976,.T.);
#14127=ORIENTED_EDGE('',*,*,#9777,.T.);
#14128=ORIENTED_EDGE('',*,*,#9979,.F.);
#14129=ORIENTED_EDGE('',*,*,#9244,.F.);
#14130=ORIENTED_EDGE('',*,*,#9978,.T.);
#14131=ORIENTED_EDGE('',*,*,#9116,.F.);
#14132=ORIENTED_EDGE('',*,*,#9980,.F.);
#14133=ORIENTED_EDGE('',*,*,#9774,.T.);
#14134=ORIENTED_EDGE('',*,*,#9979,.T.);
#14135=ORIENTED_EDGE('',*,*,#9776,.T.);
#14136=ORIENTED_EDGE('',*,*,#9981,.F.);
#14137=ORIENTED_EDGE('',*,*,#9114,.F.);
#14138=ORIENTED_EDGE('',*,*,#9245,.F.);
#14139=ORIENTED_EDGE('',*,*,#9980,.T.);
#14140=ORIENTED_EDGE('',*,*,#9115,.F.);
#14141=ORIENTED_EDGE('',*,*,#9981,.T.);
#14142=ORIENTED_EDGE('',*,*,#9775,.T.);
#14143=ORIENTED_EDGE('',*,*,#9982,.F.);
#14144=ORIENTED_EDGE('',*,*,#9240,.F.);
#14145=ORIENTED_EDGE('',*,*,#9124,.F.);
#14146=ORIENTED_EDGE('',*,*,#9983,.F.);
#14147=ORIENTED_EDGE('',*,*,#9778,.T.);
#14148=ORIENTED_EDGE('',*,*,#9983,.T.);
#14149=ORIENTED_EDGE('',*,*,#9123,.F.);
#14150=ORIENTED_EDGE('',*,*,#9984,.F.);
#14151=ORIENTED_EDGE('',*,*,#9779,.T.);
#14152=ORIENTED_EDGE('',*,*,#9982,.T.);
#14153=ORIENTED_EDGE('',*,*,#9783,.T.);
#14154=ORIENTED_EDGE('',*,*,#9985,.F.);
#14155=ORIENTED_EDGE('',*,*,#9241,.F.);
#14156=ORIENTED_EDGE('',*,*,#9984,.T.);
#14157=ORIENTED_EDGE('',*,*,#9122,.F.);
#14158=ORIENTED_EDGE('',*,*,#9986,.F.);
#14159=ORIENTED_EDGE('',*,*,#9780,.T.);
#14160=ORIENTED_EDGE('',*,*,#9985,.T.);
#14161=ORIENTED_EDGE('',*,*,#9782,.T.);
#14162=ORIENTED_EDGE('',*,*,#9987,.F.);
#14163=ORIENTED_EDGE('',*,*,#9120,.F.);
#14164=ORIENTED_EDGE('',*,*,#9242,.F.);
#14165=ORIENTED_EDGE('',*,*,#9986,.T.);
#14166=ORIENTED_EDGE('',*,*,#9121,.F.);
#14167=ORIENTED_EDGE('',*,*,#9987,.T.);
#14168=ORIENTED_EDGE('',*,*,#9781,.T.);
#14169=ORIENTED_EDGE('',*,*,#9988,.F.);
#14170=ORIENTED_EDGE('',*,*,#9237,.F.);
#14171=ORIENTED_EDGE('',*,*,#9130,.F.);
#14172=ORIENTED_EDGE('',*,*,#9989,.F.);
#14173=ORIENTED_EDGE('',*,*,#9784,.T.);
#14174=ORIENTED_EDGE('',*,*,#9989,.T.);
#14175=ORIENTED_EDGE('',*,*,#9129,.F.);
#14176=ORIENTED_EDGE('',*,*,#9990,.F.);
#14177=ORIENTED_EDGE('',*,*,#9785,.T.);
#14178=ORIENTED_EDGE('',*,*,#9988,.T.);
#14179=ORIENTED_EDGE('',*,*,#9789,.T.);
#14180=ORIENTED_EDGE('',*,*,#9991,.F.);
#14181=ORIENTED_EDGE('',*,*,#9238,.F.);
#14182=ORIENTED_EDGE('',*,*,#9990,.T.);
#14183=ORIENTED_EDGE('',*,*,#9128,.F.);
#14184=ORIENTED_EDGE('',*,*,#9992,.F.);
#14185=ORIENTED_EDGE('',*,*,#9786,.T.);
#14186=ORIENTED_EDGE('',*,*,#9991,.T.);
#14187=ORIENTED_EDGE('',*,*,#9788,.T.);
#14188=ORIENTED_EDGE('',*,*,#9993,.F.);
#14189=ORIENTED_EDGE('',*,*,#9126,.F.);
#14190=ORIENTED_EDGE('',*,*,#9239,.F.);
#14191=ORIENTED_EDGE('',*,*,#9992,.T.);
#14192=ORIENTED_EDGE('',*,*,#9127,.F.);
#14193=ORIENTED_EDGE('',*,*,#9993,.T.);
#14194=ORIENTED_EDGE('',*,*,#9787,.T.);
#14195=ORIENTED_EDGE('',*,*,#9994,.F.);
#14196=ORIENTED_EDGE('',*,*,#9234,.F.);
#14197=ORIENTED_EDGE('',*,*,#9136,.F.);
#14198=ORIENTED_EDGE('',*,*,#9995,.F.);
#14199=ORIENTED_EDGE('',*,*,#9790,.T.);
#14200=ORIENTED_EDGE('',*,*,#9995,.T.);
#14201=ORIENTED_EDGE('',*,*,#9135,.F.);
#14202=ORIENTED_EDGE('',*,*,#9996,.F.);
#14203=ORIENTED_EDGE('',*,*,#9791,.T.);
#14204=ORIENTED_EDGE('',*,*,#9994,.T.);
#14205=ORIENTED_EDGE('',*,*,#9795,.T.);
#14206=ORIENTED_EDGE('',*,*,#9997,.F.);
#14207=ORIENTED_EDGE('',*,*,#9235,.F.);
#14208=ORIENTED_EDGE('',*,*,#9996,.T.);
#14209=ORIENTED_EDGE('',*,*,#9134,.F.);
#14210=ORIENTED_EDGE('',*,*,#9998,.F.);
#14211=ORIENTED_EDGE('',*,*,#9792,.T.);
#14212=ORIENTED_EDGE('',*,*,#9997,.T.);
#14213=ORIENTED_EDGE('',*,*,#9794,.T.);
#14214=ORIENTED_EDGE('',*,*,#9999,.F.);
#14215=ORIENTED_EDGE('',*,*,#9132,.F.);
#14216=ORIENTED_EDGE('',*,*,#9236,.F.);
#14217=ORIENTED_EDGE('',*,*,#9998,.T.);
#14218=ORIENTED_EDGE('',*,*,#9133,.F.);
#14219=ORIENTED_EDGE('',*,*,#9999,.T.);
#14220=ORIENTED_EDGE('',*,*,#9793,.T.);
#14221=ORIENTED_EDGE('',*,*,#10000,.F.);
#14222=ORIENTED_EDGE('',*,*,#9279,.F.);
#14223=ORIENTED_EDGE('',*,*,#9278,.F.);
#14224=ORIENTED_EDGE('',*,*,#9050,.F.);
#14225=ORIENTED_EDGE('',*,*,#10001,.F.);
#14226=ORIENTED_EDGE('',*,*,#9796,.T.);
#14227=ORIENTED_EDGE('',*,*,#10001,.T.);
#14228=ORIENTED_EDGE('',*,*,#9049,.F.);
#14229=ORIENTED_EDGE('',*,*,#9048,.F.);
#14230=ORIENTED_EDGE('',*,*,#10002,.F.);
#14231=ORIENTED_EDGE('',*,*,#9797,.T.);
#14232=ORIENTED_EDGE('',*,*,#10000,.T.);
#14233=ORIENTED_EDGE('',*,*,#9801,.T.);
#14234=ORIENTED_EDGE('',*,*,#10003,.F.);
#14235=ORIENTED_EDGE('',*,*,#9280,.F.);
#14236=ORIENTED_EDGE('',*,*,#10002,.T.);
#14237=ORIENTED_EDGE('',*,*,#9047,.F.);
#14238=ORIENTED_EDGE('',*,*,#10004,.F.);
#14239=ORIENTED_EDGE('',*,*,#9798,.T.);
#14240=ORIENTED_EDGE('',*,*,#10003,.T.);
#14241=ORIENTED_EDGE('',*,*,#9800,.T.);
#14242=ORIENTED_EDGE('',*,*,#10005,.F.);
#14243=ORIENTED_EDGE('',*,*,#9044,.F.);
#14244=ORIENTED_EDGE('',*,*,#9282,.F.);
#14245=ORIENTED_EDGE('',*,*,#9281,.F.);
#14246=ORIENTED_EDGE('',*,*,#10004,.T.);
#14247=ORIENTED_EDGE('',*,*,#9046,.F.);
#14248=ORIENTED_EDGE('',*,*,#9045,.F.);
#14249=ORIENTED_EDGE('',*,*,#10005,.T.);
#14250=ORIENTED_EDGE('',*,*,#9799,.T.);
#14251=ORIENTED_EDGE('',*,*,#10006,.F.);
#14252=ORIENTED_EDGE('',*,*,#9274,.F.);
#14253=ORIENTED_EDGE('',*,*,#9273,.F.);
#14254=ORIENTED_EDGE('',*,*,#9058,.F.);
#14255=ORIENTED_EDGE('',*,*,#10007,.F.);
#14256=ORIENTED_EDGE('',*,*,#9802,.T.);
#14257=ORIENTED_EDGE('',*,*,#10007,.T.);
#14258=ORIENTED_EDGE('',*,*,#9057,.F.);
#14259=ORIENTED_EDGE('',*,*,#9056,.F.);
#14260=ORIENTED_EDGE('',*,*,#10008,.F.);
#14261=ORIENTED_EDGE('',*,*,#9803,.T.);
#14262=ORIENTED_EDGE('',*,*,#10006,.T.);
#14263=ORIENTED_EDGE('',*,*,#9807,.T.);
#14264=ORIENTED_EDGE('',*,*,#10009,.F.);
#14265=ORIENTED_EDGE('',*,*,#9275,.F.);
#14266=ORIENTED_EDGE('',*,*,#10008,.T.);
#14267=ORIENTED_EDGE('',*,*,#9055,.F.);
#14268=ORIENTED_EDGE('',*,*,#10010,.F.);
#14269=ORIENTED_EDGE('',*,*,#9804,.T.);
#14270=ORIENTED_EDGE('',*,*,#10009,.T.);
#14271=ORIENTED_EDGE('',*,*,#9806,.T.);
#14272=ORIENTED_EDGE('',*,*,#10011,.F.);
#14273=ORIENTED_EDGE('',*,*,#9052,.F.);
#14274=ORIENTED_EDGE('',*,*,#9277,.F.);
#14275=ORIENTED_EDGE('',*,*,#9276,.F.);
#14276=ORIENTED_EDGE('',*,*,#10010,.T.);
#14277=ORIENTED_EDGE('',*,*,#9054,.F.);
#14278=ORIENTED_EDGE('',*,*,#9053,.F.);
#14279=ORIENTED_EDGE('',*,*,#10011,.T.);
#14280=ORIENTED_EDGE('',*,*,#9805,.T.);
#14281=ORIENTED_EDGE('',*,*,#10012,.F.);
#14282=ORIENTED_EDGE('',*,*,#9269,.F.);
#14283=ORIENTED_EDGE('',*,*,#9268,.F.);
#14284=ORIENTED_EDGE('',*,*,#9069,.F.);
#14285=ORIENTED_EDGE('',*,*,#10013,.F.);
#14286=ORIENTED_EDGE('',*,*,#9808,.T.);
#14287=ORIENTED_EDGE('',*,*,#10013,.T.);
#14288=ORIENTED_EDGE('',*,*,#9068,.F.);
#14289=ORIENTED_EDGE('',*,*,#9067,.F.);
#14290=ORIENTED_EDGE('',*,*,#10014,.F.);
#14291=ORIENTED_EDGE('',*,*,#9809,.T.);
#14292=ORIENTED_EDGE('',*,*,#10012,.T.);
#14293=ORIENTED_EDGE('',*,*,#9813,.T.);
#14294=ORIENTED_EDGE('',*,*,#10015,.F.);
#14295=ORIENTED_EDGE('',*,*,#9271,.F.);
#14296=ORIENTED_EDGE('',*,*,#9270,.F.);
#14297=ORIENTED_EDGE('',*,*,#10014,.T.);
#14298=ORIENTED_EDGE('',*,*,#9066,.F.);
#14299=ORIENTED_EDGE('',*,*,#9065,.F.);
#14300=ORIENTED_EDGE('',*,*,#10016,.F.);
#14301=ORIENTED_EDGE('',*,*,#9810,.T.);
#14302=ORIENTED_EDGE('',*,*,#10015,.T.);
#14303=ORIENTED_EDGE('',*,*,#9812,.T.);
#14304=ORIENTED_EDGE('',*,*,#10017,.F.);
#14305=ORIENTED_EDGE('',*,*,#9060,.F.);
#14306=ORIENTED_EDGE('',*,*,#9272,.F.);
#14307=ORIENTED_EDGE('',*,*,#10016,.T.);
#14308=ORIENTED_EDGE('',*,*,#9064,.F.);
#14309=ORIENTED_EDGE('',*,*,#9063,.F.);
#14310=ORIENTED_EDGE('',*,*,#9062,.F.);
#14311=ORIENTED_EDGE('',*,*,#9061,.F.);
#14312=ORIENTED_EDGE('',*,*,#10017,.T.);
#14313=ORIENTED_EDGE('',*,*,#9811,.T.);
#14314=ORIENTED_EDGE('',*,*,#10018,.F.);
#14315=ORIENTED_EDGE('',*,*,#9264,.F.);
#14316=ORIENTED_EDGE('',*,*,#9076,.F.);
#14317=ORIENTED_EDGE('',*,*,#10019,.F.);
#14318=ORIENTED_EDGE('',*,*,#9814,.T.);
#14319=ORIENTED_EDGE('',*,*,#10019,.T.);
#14320=ORIENTED_EDGE('',*,*,#9075,.F.);
#14321=ORIENTED_EDGE('',*,*,#10020,.F.);
#14322=ORIENTED_EDGE('',*,*,#9815,.T.);
#14323=ORIENTED_EDGE('',*,*,#10018,.T.);
#14324=ORIENTED_EDGE('',*,*,#9819,.T.);
#14325=ORIENTED_EDGE('',*,*,#10021,.F.);
#14326=ORIENTED_EDGE('',*,*,#9265,.F.);
#14327=ORIENTED_EDGE('',*,*,#10020,.T.);
#14328=ORIENTED_EDGE('',*,*,#9074,.F.);
#14329=ORIENTED_EDGE('',*,*,#10022,.F.);
#14330=ORIENTED_EDGE('',*,*,#9816,.T.);
#14331=ORIENTED_EDGE('',*,*,#10021,.T.);
#14332=ORIENTED_EDGE('',*,*,#9818,.T.);
#14333=ORIENTED_EDGE('',*,*,#10023,.F.);
#14334=ORIENTED_EDGE('',*,*,#9071,.F.);
#14335=ORIENTED_EDGE('',*,*,#9267,.F.);
#14336=ORIENTED_EDGE('',*,*,#9266,.F.);
#14337=ORIENTED_EDGE('',*,*,#10022,.T.);
#14338=ORIENTED_EDGE('',*,*,#9073,.F.);
#14339=ORIENTED_EDGE('',*,*,#9072,.F.);
#14340=ORIENTED_EDGE('',*,*,#10023,.T.);
#14341=ORIENTED_EDGE('',*,*,#9817,.T.);
#14342=ORIENTED_EDGE('',*,*,#10024,.F.);
#14343=ORIENTED_EDGE('',*,*,#9148,.F.);
#14344=ORIENTED_EDGE('',*,*,#9147,.F.);
#14345=ORIENTED_EDGE('',*,*,#10025,.F.);
#14346=ORIENTED_EDGE('',*,*,#9820,.T.);
#14347=ORIENTED_EDGE('',*,*,#10025,.T.);
#14348=ORIENTED_EDGE('',*,*,#9146,.F.);
#14349=ORIENTED_EDGE('',*,*,#10026,.F.);
#14350=ORIENTED_EDGE('',*,*,#9821,.T.);
#14351=ORIENTED_EDGE('',*,*,#10024,.T.);
#14352=ORIENTED_EDGE('',*,*,#9825,.T.);
#14353=ORIENTED_EDGE('',*,*,#10027,.F.);
#14354=ORIENTED_EDGE('',*,*,#9149,.F.);
#14355=ORIENTED_EDGE('',*,*,#10026,.T.);
#14356=ORIENTED_EDGE('',*,*,#9145,.F.);
#14357=ORIENTED_EDGE('',*,*,#9144,.F.);
#14358=ORIENTED_EDGE('',*,*,#9230,.F.);
#14359=ORIENTED_EDGE('',*,*,#9229,.F.);
#14360=ORIENTED_EDGE('',*,*,#9228,.F.);
#14361=ORIENTED_EDGE('',*,*,#10028,.F.);
#14362=ORIENTED_EDGE('',*,*,#9822,.T.);
#14363=ORIENTED_EDGE('',*,*,#10027,.T.);
#14364=ORIENTED_EDGE('',*,*,#9824,.T.);
#14365=ORIENTED_EDGE('',*,*,#10029,.F.);
#14366=ORIENTED_EDGE('',*,*,#9225,.F.);
#14367=ORIENTED_EDGE('',*,*,#9150,.F.);
#14368=ORIENTED_EDGE('',*,*,#10028,.T.);
#14369=ORIENTED_EDGE('',*,*,#9227,.F.);
#14370=ORIENTED_EDGE('',*,*,#9226,.F.);
#14371=ORIENTED_EDGE('',*,*,#10029,.T.);
#14372=ORIENTED_EDGE('',*,*,#9823,.T.);
#14373=ORIENTED_EDGE('',*,*,#10030,.F.);
#14374=ORIENTED_EDGE('',*,*,#9310,.F.);
#14375=ORIENTED_EDGE('',*,*,#9309,.F.);
#14376=ORIENTED_EDGE('',*,*,#10031,.F.);
#14377=ORIENTED_EDGE('',*,*,#9172,.T.);
#14378=ORIENTED_EDGE('',*,*,#10031,.T.);
#14379=ORIENTED_EDGE('',*,*,#9308,.F.);
#14380=ORIENTED_EDGE('',*,*,#10032,.F.);
#14381=ORIENTED_EDGE('',*,*,#9173,.F.);
#14382=ORIENTED_EDGE('',*,*,#10030,.T.);
#14383=ORIENTED_EDGE('',*,*,#9171,.T.);
#14384=ORIENTED_EDGE('',*,*,#10033,.F.);
#14385=ORIENTED_EDGE('',*,*,#9312,.F.);
#14386=ORIENTED_EDGE('',*,*,#9311,.F.);
#14387=ORIENTED_EDGE('',*,*,#10032,.T.);
#14388=ORIENTED_EDGE('',*,*,#9307,.F.);
#14389=ORIENTED_EDGE('',*,*,#10034,.F.);
#14390=ORIENTED_EDGE('',*,*,#9174,.F.);
#14391=ORIENTED_EDGE('',*,*,#10033,.T.);
#14392=ORIENTED_EDGE('',*,*,#9170,.F.);
#14393=ORIENTED_EDGE('',*,*,#10035,.F.);
#14394=ORIENTED_EDGE('',*,*,#9314,.F.);
#14395=ORIENTED_EDGE('',*,*,#9313,.F.);
#14396=ORIENTED_EDGE('',*,*,#10034,.T.);
#14397=ORIENTED_EDGE('',*,*,#9306,.F.);
#14398=ORIENTED_EDGE('',*,*,#10036,.F.);
#14399=ORIENTED_EDGE('',*,*,#9175,.F.);
#14400=ORIENTED_EDGE('',*,*,#10035,.T.);
#14401=ORIENTED_EDGE('',*,*,#9169,.F.);
#14402=ORIENTED_EDGE('',*,*,#10037,.F.);
#14403=ORIENTED_EDGE('',*,*,#9316,.F.);
#14404=ORIENTED_EDGE('',*,*,#9315,.F.);
#14405=ORIENTED_EDGE('',*,*,#10036,.T.);
#14406=ORIENTED_EDGE('',*,*,#9305,.F.);
#14407=ORIENTED_EDGE('',*,*,#10038,.F.);
#14408=ORIENTED_EDGE('',*,*,#9176,.T.);
#14409=ORIENTED_EDGE('',*,*,#10037,.T.);
#14410=ORIENTED_EDGE('',*,*,#9619,.F.);
#14411=ORIENTED_EDGE('',*,*,#10039,.F.);
#14412=ORIENTED_EDGE('',*,*,#9317,.F.);
#14413=ORIENTED_EDGE('',*,*,#10038,.T.);
#14414=ORIENTED_EDGE('',*,*,#9304,.F.);
#14415=ORIENTED_EDGE('',*,*,#9303,.F.);
#14416=ORIENTED_EDGE('',*,*,#9302,.F.);
#14417=ORIENTED_EDGE('',*,*,#10040,.F.);
#14418=ORIENTED_EDGE('',*,*,#9177,.T.);
#14419=ORIENTED_EDGE('',*,*,#10039,.T.);
#14420=ORIENTED_EDGE('',*,*,#9618,.F.);
#14421=ORIENTED_EDGE('',*,*,#10041,.F.);
#14422=ORIENTED_EDGE('',*,*,#9318,.F.);
#14423=ORIENTED_EDGE('',*,*,#10040,.T.);
#14424=ORIENTED_EDGE('',*,*,#9301,.F.);
#14425=ORIENTED_EDGE('',*,*,#10042,.F.);
#14426=ORIENTED_EDGE('',*,*,#9178,.F.);
#14427=ORIENTED_EDGE('',*,*,#10041,.T.);
#14428=ORIENTED_EDGE('',*,*,#9617,.F.);
#14429=ORIENTED_EDGE('',*,*,#10043,.F.);
#14430=ORIENTED_EDGE('',*,*,#9319,.F.);
#14431=ORIENTED_EDGE('',*,*,#10042,.T.);
#14432=ORIENTED_EDGE('',*,*,#9300,.F.);
#14433=ORIENTED_EDGE('',*,*,#10044,.F.);
#14434=ORIENTED_EDGE('',*,*,#9179,.F.);
#14435=ORIENTED_EDGE('',*,*,#10043,.T.);
#14436=ORIENTED_EDGE('',*,*,#9616,.F.);
#14437=ORIENTED_EDGE('',*,*,#10045,.F.);
#14438=ORIENTED_EDGE('',*,*,#9320,.F.);
#14439=ORIENTED_EDGE('',*,*,#10044,.T.);
#14440=ORIENTED_EDGE('',*,*,#9299,.F.);
#14441=ORIENTED_EDGE('',*,*,#9298,.F.);
#14442=ORIENTED_EDGE('',*,*,#9297,.F.);
#14443=ORIENTED_EDGE('',*,*,#10046,.F.);
#14444=ORIENTED_EDGE('',*,*,#9180,.T.);
#14445=ORIENTED_EDGE('',*,*,#10045,.T.);
#14446=ORIENTED_EDGE('',*,*,#9615,.F.);
#14447=ORIENTED_EDGE('',*,*,#10047,.F.);
#14448=ORIENTED_EDGE('',*,*,#9321,.F.);
#14449=ORIENTED_EDGE('',*,*,#10046,.T.);
#14450=ORIENTED_EDGE('',*,*,#9296,.F.);
#14451=ORIENTED_EDGE('',*,*,#10048,.F.);
#14452=ORIENTED_EDGE('',*,*,#9181,.T.);
#14453=ORIENTED_EDGE('',*,*,#10047,.T.);
#14454=ORIENTED_EDGE('',*,*,#9614,.F.);
#14455=ORIENTED_EDGE('',*,*,#10049,.F.);
#14456=ORIENTED_EDGE('',*,*,#9322,.F.);
#14457=ORIENTED_EDGE('',*,*,#10048,.T.);
#14458=ORIENTED_EDGE('',*,*,#9295,.F.);
#14459=ORIENTED_EDGE('',*,*,#10050,.F.);
#14460=ORIENTED_EDGE('',*,*,#9182,.T.);
#14461=ORIENTED_EDGE('',*,*,#10049,.T.);
#14462=ORIENTED_EDGE('',*,*,#9613,.F.);
#14463=ORIENTED_EDGE('',*,*,#9167,.F.);
#14464=ORIENTED_EDGE('',*,*,#10051,.F.);
#14465=ORIENTED_EDGE('',*,*,#9323,.F.);
#14466=ORIENTED_EDGE('',*,*,#10050,.T.);
#14467=ORIENTED_EDGE('',*,*,#9294,.F.);
#14468=ORIENTED_EDGE('',*,*,#10052,.F.);
#14469=ORIENTED_EDGE('',*,*,#9183,.T.);
#14470=ORIENTED_EDGE('',*,*,#10051,.T.);
#14471=ORIENTED_EDGE('',*,*,#9166,.T.);
#14472=ORIENTED_EDGE('',*,*,#9206,.T.);
#14473=ORIENTED_EDGE('',*,*,#10053,.F.);
#14474=ORIENTED_EDGE('',*,*,#9324,.F.);
#14475=ORIENTED_EDGE('',*,*,#10052,.T.);
#14476=ORIENTED_EDGE('',*,*,#9293,.F.);
#14477=ORIENTED_EDGE('',*,*,#10054,.F.);
#14478=ORIENTED_EDGE('',*,*,#9184,.T.);
#14479=ORIENTED_EDGE('',*,*,#10053,.T.);
#14480=ORIENTED_EDGE('',*,*,#9205,.T.);
#14481=ORIENTED_EDGE('',*,*,#9196,.T.);
#14482=ORIENTED_EDGE('',*,*,#10055,.F.);
#14483=ORIENTED_EDGE('',*,*,#9022,.F.);
#14484=ORIENTED_EDGE('',*,*,#9325,.F.);
#14485=ORIENTED_EDGE('',*,*,#10054,.T.);
#14486=ORIENTED_EDGE('',*,*,#9292,.F.);
#14487=ORIENTED_EDGE('',*,*,#10056,.F.);
#14488=ORIENTED_EDGE('',*,*,#9185,.T.);
#14489=ORIENTED_EDGE('',*,*,#10055,.T.);
#14490=ORIENTED_EDGE('',*,*,#9195,.F.);
#14491=ORIENTED_EDGE('',*,*,#10057,.F.);
#14492=ORIENTED_EDGE('',*,*,#9024,.F.);
#14493=ORIENTED_EDGE('',*,*,#9023,.F.);
#14494=ORIENTED_EDGE('',*,*,#10056,.T.);
#14495=ORIENTED_EDGE('',*,*,#9291,.F.);
#14496=ORIENTED_EDGE('',*,*,#9290,.F.);
#14497=ORIENTED_EDGE('',*,*,#10058,.F.);
#14498=ORIENTED_EDGE('',*,*,#9186,.T.);
#14499=ORIENTED_EDGE('',*,*,#10057,.T.);
#14500=ORIENTED_EDGE('',*,*,#9194,.F.);
#14501=ORIENTED_EDGE('',*,*,#10059,.F.);
#14502=ORIENTED_EDGE('',*,*,#9025,.F.);
#14503=ORIENTED_EDGE('',*,*,#10058,.T.);
#14504=ORIENTED_EDGE('',*,*,#9289,.F.);
#14505=ORIENTED_EDGE('',*,*,#9288,.F.);
#14506=ORIENTED_EDGE('',*,*,#9034,.F.);
#14507=ORIENTED_EDGE('',*,*,#10060,.F.);
#14508=ORIENTED_EDGE('',*,*,#9187,.T.);
#14509=ORIENTED_EDGE('',*,*,#10059,.T.);
#14510=ORIENTED_EDGE('',*,*,#9193,.T.);
#14511=ORIENTED_EDGE('',*,*,#10061,.F.);
#14512=ORIENTED_EDGE('',*,*,#9026,.F.);
#14513=ORIENTED_EDGE('',*,*,#10060,.T.);
#14514=ORIENTED_EDGE('',*,*,#9033,.F.);
#14515=ORIENTED_EDGE('',*,*,#9032,.F.);
#14516=ORIENTED_EDGE('',*,*,#10062,.F.);
#14517=ORIENTED_EDGE('',*,*,#9188,.T.);
#14518=ORIENTED_EDGE('',*,*,#10061,.T.);
#14519=ORIENTED_EDGE('',*,*,#9192,.T.);
#14520=ORIENTED_EDGE('',*,*,#10063,.F.);
#14521=ORIENTED_EDGE('',*,*,#9027,.F.);
#14522=ORIENTED_EDGE('',*,*,#10062,.T.);
#14523=ORIENTED_EDGE('',*,*,#9031,.F.);
#14524=ORIENTED_EDGE('',*,*,#10064,.F.);
#14525=ORIENTED_EDGE('',*,*,#9189,.F.);
#14526=ORIENTED_EDGE('',*,*,#10063,.T.);
#14527=ORIENTED_EDGE('',*,*,#9191,.T.);
#14528=ORIENTED_EDGE('',*,*,#10065,.F.);
#14529=ORIENTED_EDGE('',*,*,#9028,.F.);
#14530=ORIENTED_EDGE('',*,*,#10064,.T.);
#14531=ORIENTED_EDGE('',*,*,#9030,.F.);
#14532=ORIENTED_EDGE('',*,*,#9029,.F.);
#14533=ORIENTED_EDGE('',*,*,#10065,.T.);
#14534=ORIENTED_EDGE('',*,*,#9190,.F.);
#14535=ORIENTED_EDGE('',*,*,#10066,.F.);
#14536=ORIENTED_EDGE('',*,*,#9453,.F.);
#14537=ORIENTED_EDGE('',*,*,#9020,.F.);
#14538=ORIENTED_EDGE('',*,*,#10067,.F.);
#14539=ORIENTED_EDGE('',*,*,#9161,.T.);
#14540=ORIENTED_EDGE('',*,*,#9208,.T.);
#14541=ORIENTED_EDGE('',*,*,#10067,.T.);
#14542=ORIENTED_EDGE('',*,*,#9019,.F.);
#14543=ORIENTED_EDGE('',*,*,#9018,.F.);
#14544=ORIENTED_EDGE('',*,*,#9017,.F.);
#14545=ORIENTED_EDGE('',*,*,#10068,.F.);
#14546=ORIENTED_EDGE('',*,*,#9162,.F.);
#14547=ORIENTED_EDGE('',*,*,#10066,.T.);
#14548=ORIENTED_EDGE('',*,*,#9207,.T.);
#14549=ORIENTED_EDGE('',*,*,#9164,.T.);
#14550=ORIENTED_EDGE('',*,*,#10069,.F.);
#14551=ORIENTED_EDGE('',*,*,#9015,.F.);
#14552=ORIENTED_EDGE('',*,*,#9014,.F.);
#14553=ORIENTED_EDGE('',*,*,#10068,.T.);
#14554=ORIENTED_EDGE('',*,*,#9016,.F.);
#14555=ORIENTED_EDGE('',*,*,#10069,.T.);
#14556=ORIENTED_EDGE('',*,*,#9163,.F.);
#14557=ORIENTED_EDGE('',*,*,#10070,.F.);
#14558=ORIENTED_EDGE('',*,*,#10071,.F.);
#14559=ORIENTED_EDGE('',*,*,#10072,.T.);
#14560=ORIENTED_EDGE('',*,*,#10073,.F.);
#14561=ORIENTED_EDGE('',*,*,#10074,.F.);
#14562=ORIENTED_EDGE('',*,*,#10075,.F.);
#14563=ORIENTED_EDGE('',*,*,#10076,.F.);
#14564=ORIENTED_EDGE('',*,*,#10077,.F.);
#14565=ORIENTED_EDGE('',*,*,#10078,.F.);
#14566=ORIENTED_EDGE('',*,*,#10079,.F.);
#14567=ORIENTED_EDGE('',*,*,#10080,.F.);
#14568=ORIENTED_EDGE('',*,*,#10081,.F.);
#14569=ORIENTED_EDGE('',*,*,#10082,.T.);
#14570=ORIENTED_EDGE('',*,*,#10083,.F.);
#14571=ORIENTED_EDGE('',*,*,#10084,.F.);
#14572=ORIENTED_EDGE('',*,*,#10085,.T.);
#14573=ORIENTED_EDGE('',*,*,#10086,.F.);
#14574=ORIENTED_EDGE('',*,*,#10087,.T.);
#14575=ORIENTED_EDGE('',*,*,#10088,.F.);
#14576=ORIENTED_EDGE('',*,*,#10089,.T.);
#14577=ORIENTED_EDGE('',*,*,#10090,.F.);
#14578=ORIENTED_EDGE('',*,*,#10091,.F.);
#14579=ORIENTED_EDGE('',*,*,#10092,.T.);
#14580=ORIENTED_EDGE('',*,*,#10093,.F.);
#14581=ORIENTED_EDGE('',*,*,#10094,.F.);
#14582=ORIENTED_EDGE('',*,*,#10095,.F.);
#14583=ORIENTED_EDGE('',*,*,#10096,.F.);
#14584=ORIENTED_EDGE('',*,*,#10097,.F.);
#14585=ORIENTED_EDGE('',*,*,#10098,.F.);
#14586=ORIENTED_EDGE('',*,*,#10099,.F.);
#14587=ORIENTED_EDGE('',*,*,#10100,.T.);
#14588=ORIENTED_EDGE('',*,*,#10101,.T.);
#14589=ORIENTED_EDGE('',*,*,#10102,.T.);
#14590=ORIENTED_EDGE('',*,*,#10103,.T.);
#14591=ORIENTED_EDGE('',*,*,#10104,.T.);
#14592=ORIENTED_EDGE('',*,*,#10105,.T.);
#14593=ORIENTED_EDGE('',*,*,#10106,.T.);
#14594=ORIENTED_EDGE('',*,*,#10107,.T.);
#14595=ORIENTED_EDGE('',*,*,#10108,.T.);
#14596=ORIENTED_EDGE('',*,*,#10109,.T.);
#14597=ORIENTED_EDGE('',*,*,#10099,.T.);
#14598=ORIENTED_EDGE('',*,*,#10109,.F.);
#14599=ORIENTED_EDGE('',*,*,#10110,.T.);
#14600=ORIENTED_EDGE('',*,*,#10111,.T.);
#14601=ORIENTED_EDGE('',*,*,#10112,.T.);
#14602=ORIENTED_EDGE('',*,*,#10113,.T.);
#14603=ORIENTED_EDGE('',*,*,#10114,.T.);
#14604=ORIENTED_EDGE('',*,*,#10115,.T.);
#14605=ORIENTED_EDGE('',*,*,#10116,.T.);
#14606=ORIENTED_EDGE('',*,*,#10117,.T.);
#14607=ORIENTED_EDGE('',*,*,#10118,.T.);
#14608=ORIENTED_EDGE('',*,*,#10119,.F.);
#14609=ORIENTED_EDGE('',*,*,#10117,.F.);
#14610=ORIENTED_EDGE('',*,*,#10120,.T.);
#14611=ORIENTED_EDGE('',*,*,#10106,.F.);
#14612=ORIENTED_EDGE('',*,*,#10121,.T.);
#14613=ORIENTED_EDGE('',*,*,#10104,.F.);
#14614=ORIENTED_EDGE('',*,*,#10122,.T.);
#14615=ORIENTED_EDGE('',*,*,#10111,.F.);
#14616=ORIENTED_EDGE('',*,*,#10123,.T.);
#14617=ORIENTED_EDGE('',*,*,#10124,.T.);
#14618=ORIENTED_EDGE('',*,*,#10083,.T.);
#14619=ORIENTED_EDGE('',*,*,#10115,.F.);
#14620=ORIENTED_EDGE('',*,*,#10125,.T.);
#14621=ORIENTED_EDGE('',*,*,#10100,.F.);
#14622=ORIENTED_EDGE('',*,*,#10126,.T.);
#14623=ORIENTED_EDGE('',*,*,#10113,.F.);
#14624=ORIENTED_EDGE('',*,*,#10127,.T.);
#14625=ORIENTED_EDGE('',*,*,#10102,.F.);
#14626=ORIENTED_EDGE('',*,*,#10128,.T.);
#14627=ORIENTED_EDGE('',*,*,#10112,.F.);
#14628=ORIENTED_EDGE('',*,*,#10122,.F.);
#14629=ORIENTED_EDGE('',*,*,#10103,.F.);
#14630=ORIENTED_EDGE('',*,*,#10127,.F.);
#14631=ORIENTED_EDGE('',*,*,#10114,.F.);
#14632=ORIENTED_EDGE('',*,*,#10128,.F.);
#14633=ORIENTED_EDGE('',*,*,#10101,.F.);
#14634=ORIENTED_EDGE('',*,*,#10125,.F.);
#14635=ORIENTED_EDGE('',*,*,#10116,.F.);
#14636=ORIENTED_EDGE('',*,*,#10126,.F.);
#14637=ORIENTED_EDGE('',*,*,#10107,.F.);
#14638=ORIENTED_EDGE('',*,*,#10120,.F.);
#14639=ORIENTED_EDGE('',*,*,#10118,.F.);
#14640=ORIENTED_EDGE('',*,*,#10121,.F.);
#14641=ORIENTED_EDGE('',*,*,#10105,.F.);
#14642=ORIENTED_EDGE('',*,*,#10123,.F.);
#14643=ORIENTED_EDGE('',*,*,#10119,.T.);
#14644=ORIENTED_EDGE('',*,*,#10129,.T.);
#14645=ORIENTED_EDGE('',*,*,#10130,.T.);
#14646=ORIENTED_EDGE('',*,*,#10131,.T.);
#14647=ORIENTED_EDGE('',*,*,#10129,.F.);
#14648=ORIENTED_EDGE('',*,*,#10132,.T.);
#14649=ORIENTED_EDGE('',*,*,#10133,.T.);
#14650=ORIENTED_EDGE('',*,*,#10132,.F.);
#14651=ORIENTED_EDGE('',*,*,#10134,.T.);
#14652=ORIENTED_EDGE('',*,*,#10130,.F.);
#14653=ORIENTED_EDGE('',*,*,#10131,.F.);
#14654=ORIENTED_EDGE('',*,*,#10134,.F.);
#14655=ORIENTED_EDGE('',*,*,#10135,.T.);
#14656=ORIENTED_EDGE('',*,*,#10136,.T.);
#14657=ORIENTED_EDGE('',*,*,#10137,.T.);
#14658=ORIENTED_EDGE('',*,*,#10136,.F.);
#14659=ORIENTED_EDGE('',*,*,#10138,.T.);
#14660=ORIENTED_EDGE('',*,*,#10081,.T.);
#14661=ORIENTED_EDGE('',*,*,#10080,.T.);
#14662=ORIENTED_EDGE('',*,*,#10079,.T.);
#14663=ORIENTED_EDGE('',*,*,#10139,.T.);
#14664=ORIENTED_EDGE('',*,*,#10073,.T.);
#14665=ORIENTED_EDGE('',*,*,#10140,.T.);
#14666=ORIENTED_EDGE('',*,*,#10074,.T.);
#14667=ORIENTED_EDGE('',*,*,#10139,.F.);
#14668=ORIENTED_EDGE('',*,*,#10078,.T.);
#14669=ORIENTED_EDGE('',*,*,#10077,.T.);
#14670=ORIENTED_EDGE('',*,*,#10076,.T.);
#14671=ORIENTED_EDGE('',*,*,#10141,.T.);
#14672=ORIENTED_EDGE('',*,*,#10142,.T.);
#14673=ORIENTED_EDGE('',*,*,#10143,.T.);
#14674=ORIENTED_EDGE('',*,*,#10088,.T.);
#14675=ORIENTED_EDGE('',*,*,#10087,.F.);
#14676=ORIENTED_EDGE('',*,*,#10086,.T.);
#14677=ORIENTED_EDGE('',*,*,#10085,.F.);
#14678=ORIENTED_EDGE('',*,*,#10144,.F.);
#14679=ORIENTED_EDGE('',*,*,#10145,.T.);
#14680=ORIENTED_EDGE('',*,*,#10091,.T.);
#14681=ORIENTED_EDGE('',*,*,#10090,.T.);
#14682=ORIENTED_EDGE('',*,*,#10089,.F.);
#14683=ORIENTED_EDGE('',*,*,#10143,.F.);
#14684=ORIENTED_EDGE('',*,*,#10146,.T.);
#14685=ORIENTED_EDGE('',*,*,#10147,.T.);
#14686=ORIENTED_EDGE('',*,*,#10071,.T.);
#14687=ORIENTED_EDGE('',*,*,#10148,.T.);
#14688=ORIENTED_EDGE('',*,*,#10149,.T.);
#14689=ORIENTED_EDGE('',*,*,#10150,.T.);
#14690=ORIENTED_EDGE('',*,*,#10151,.T.);
#14691=ORIENTED_EDGE('',*,*,#10152,.T.);
#14692=ORIENTED_EDGE('',*,*,#10153,.T.);
#14693=ORIENTED_EDGE('',*,*,#10154,.T.);
#14694=ORIENTED_EDGE('',*,*,#10155,.F.);
#14695=ORIENTED_EDGE('',*,*,#10098,.T.);
#14696=ORIENTED_EDGE('',*,*,#10097,.T.);
#14697=ORIENTED_EDGE('',*,*,#10096,.T.);
#14698=ORIENTED_EDGE('',*,*,#10156,.T.);
#14699=ORIENTED_EDGE('',*,*,#10155,.T.);
#14700=ORIENTED_EDGE('',*,*,#10156,.F.);
#14701=ORIENTED_EDGE('',*,*,#10095,.T.);
#14702=ORIENTED_EDGE('',*,*,#10094,.T.);
#14703=ORIENTED_EDGE('',*,*,#10093,.T.);
#14704=ORIENTED_EDGE('',*,*,#10157,.T.);
#14705=ORIENTED_EDGE('',*,*,#10084,.T.);
#14706=ORIENTED_EDGE('',*,*,#10157,.F.);
#14707=ORIENTED_EDGE('',*,*,#10092,.F.);
#14708=ORIENTED_EDGE('',*,*,#10145,.F.);
#14709=ORIENTED_EDGE('',*,*,#10144,.T.);
#14710=ORIENTED_EDGE('',*,*,#10075,.T.);
#14711=ORIENTED_EDGE('',*,*,#10124,.F.);
#14712=ORIENTED_EDGE('',*,*,#10082,.F.);
#14713=ORIENTED_EDGE('',*,*,#10141,.F.);
#14714=ORIENTED_EDGE('',*,*,#10149,.F.);
#14715=ORIENTED_EDGE('',*,*,#10154,.F.);
#14716=ORIENTED_EDGE('',*,*,#10153,.F.);
#14717=ORIENTED_EDGE('',*,*,#10152,.F.);
#14718=ORIENTED_EDGE('',*,*,#10158,.T.);
#14719=ORIENTED_EDGE('',*,*,#10142,.F.);
#14720=ORIENTED_EDGE('',*,*,#10146,.F.);
#14721=ORIENTED_EDGE('',*,*,#10158,.F.);
#14722=ORIENTED_EDGE('',*,*,#10151,.F.);
#14723=ORIENTED_EDGE('',*,*,#10150,.F.);
#14724=ORIENTED_EDGE('',*,*,#10070,.T.);
#14725=ORIENTED_EDGE('',*,*,#10140,.F.);
#14726=ORIENTED_EDGE('',*,*,#10072,.F.);
#14727=ORIENTED_EDGE('',*,*,#10147,.F.);
#14728=ORIENTED_EDGE('',*,*,#10148,.F.);
#14729=ORIENTED_EDGE('',*,*,#10138,.F.);
#14730=ORIENTED_EDGE('',*,*,#10159,.T.);
#14731=ORIENTED_EDGE('',*,*,#10135,.F.);
#14732=ORIENTED_EDGE('',*,*,#10159,.F.);
#14733=ORIENTED_EDGE('',*,*,#10137,.F.);
#14734=ORIENTED_EDGE('',*,*,#10160,.T.);
#14735=ORIENTED_EDGE('',*,*,#10133,.F.);
#14736=ORIENTED_EDGE('',*,*,#10160,.F.);
#14737=ORIENTED_EDGE('',*,*,#10110,.F.);
#14738=ORIENTED_EDGE('',*,*,#10161,.T.);
#14739=ORIENTED_EDGE('',*,*,#10108,.F.);
#14740=ORIENTED_EDGE('',*,*,#10161,.F.);
#14741=ORIENTED_EDGE('',*,*,#10162,.T.);
#14742=ORIENTED_EDGE('',*,*,#10163,.T.);
#14743=ORIENTED_EDGE('',*,*,#10164,.T.);
#14744=ORIENTED_EDGE('',*,*,#10165,.T.);
#14745=ORIENTED_EDGE('',*,*,#10166,.T.);
#14746=ORIENTED_EDGE('',*,*,#10167,.T.);
#14747=ORIENTED_EDGE('',*,*,#10168,.T.);
#14748=ORIENTED_EDGE('',*,*,#10169,.T.);
#14749=ORIENTED_EDGE('',*,*,#10170,.T.);
#14750=ORIENTED_EDGE('',*,*,#10171,.F.);
#14751=ORIENTED_EDGE('',*,*,#10172,.T.);
#14752=ORIENTED_EDGE('',*,*,#10173,.F.);
#14753=ORIENTED_EDGE('',*,*,#10174,.T.);
#14754=ORIENTED_EDGE('',*,*,#10175,.T.);
#14755=ORIENTED_EDGE('',*,*,#10176,.T.);
#14756=ORIENTED_EDGE('',*,*,#10177,.T.);
#14757=ORIENTED_EDGE('',*,*,#10178,.T.);
#14758=ORIENTED_EDGE('',*,*,#10179,.T.);
#14759=ORIENTED_EDGE('',*,*,#10180,.T.);
#14760=ORIENTED_EDGE('',*,*,#10181,.T.);
#14761=ORIENTED_EDGE('',*,*,#10182,.T.);
#14762=ORIENTED_EDGE('',*,*,#10183,.T.);
#14763=ORIENTED_EDGE('',*,*,#10184,.T.);
#14764=ORIENTED_EDGE('',*,*,#10185,.T.);
#14765=ORIENTED_EDGE('',*,*,#10186,.T.);
#14766=ORIENTED_EDGE('',*,*,#10187,.T.);
#14767=ORIENTED_EDGE('',*,*,#10188,.T.);
#14768=ORIENTED_EDGE('',*,*,#10189,.T.);
#14769=ORIENTED_EDGE('',*,*,#10190,.T.);
#14770=ORIENTED_EDGE('',*,*,#10191,.T.);
#14771=ORIENTED_EDGE('',*,*,#10192,.T.);
#14772=ORIENTED_EDGE('',*,*,#10193,.T.);
#14773=ORIENTED_EDGE('',*,*,#10194,.F.);
#14774=ORIENTED_EDGE('',*,*,#10195,.T.);
#14775=ORIENTED_EDGE('',*,*,#10196,.F.);
#14776=ORIENTED_EDGE('',*,*,#10197,.T.);
#14777=ORIENTED_EDGE('',*,*,#10198,.T.);
#14778=ORIENTED_EDGE('',*,*,#10199,.T.);
#14779=ORIENTED_EDGE('',*,*,#10200,.F.);
#14780=ORIENTED_EDGE('',*,*,#10201,.T.);
#14781=ORIENTED_EDGE('',*,*,#10202,.T.);
#14782=ORIENTED_EDGE('',*,*,#10203,.T.);
#14783=ORIENTED_EDGE('',*,*,#10198,.F.);
#14784=ORIENTED_EDGE('',*,*,#10204,.T.);
#14785=ORIENTED_EDGE('',*,*,#10205,.T.);
#14786=ORIENTED_EDGE('',*,*,#10206,.T.);
#14787=ORIENTED_EDGE('',*,*,#10202,.F.);
#14788=ORIENTED_EDGE('',*,*,#10207,.T.);
#14789=ORIENTED_EDGE('',*,*,#10208,.T.);
#14790=ORIENTED_EDGE('',*,*,#10209,.T.);
#14791=ORIENTED_EDGE('',*,*,#10205,.F.);
#14792=ORIENTED_EDGE('',*,*,#10210,.T.);
#14793=ORIENTED_EDGE('',*,*,#10211,.T.);
#14794=ORIENTED_EDGE('',*,*,#10212,.T.);
#14795=ORIENTED_EDGE('',*,*,#10208,.F.);
#14796=ORIENTED_EDGE('',*,*,#10213,.T.);
#14797=ORIENTED_EDGE('',*,*,#10214,.T.);
#14798=ORIENTED_EDGE('',*,*,#10215,.T.);
#14799=ORIENTED_EDGE('',*,*,#10211,.F.);
#14800=ORIENTED_EDGE('',*,*,#10216,.T.);
#14801=ORIENTED_EDGE('',*,*,#10217,.T.);
#14802=ORIENTED_EDGE('',*,*,#10218,.T.);
#14803=ORIENTED_EDGE('',*,*,#10214,.F.);
#14804=ORIENTED_EDGE('',*,*,#10219,.T.);
#14805=ORIENTED_EDGE('',*,*,#10220,.T.);
#14806=ORIENTED_EDGE('',*,*,#10221,.T.);
#14807=ORIENTED_EDGE('',*,*,#10217,.F.);
#14808=ORIENTED_EDGE('',*,*,#10222,.T.);
#14809=ORIENTED_EDGE('',*,*,#10223,.T.);
#14810=ORIENTED_EDGE('',*,*,#10224,.T.);
#14811=ORIENTED_EDGE('',*,*,#10220,.F.);
#14812=ORIENTED_EDGE('',*,*,#10225,.T.);
#14813=ORIENTED_EDGE('',*,*,#10226,.T.);
#14814=ORIENTED_EDGE('',*,*,#10227,.T.);
#14815=ORIENTED_EDGE('',*,*,#10228,.T.);
#14816=ORIENTED_EDGE('',*,*,#10229,.T.);
#14817=ORIENTED_EDGE('',*,*,#10230,.T.);
#14818=ORIENTED_EDGE('',*,*,#10231,.T.);
#14819=ORIENTED_EDGE('',*,*,#10232,.T.);
#14820=ORIENTED_EDGE('',*,*,#10233,.T.);
#14821=ORIENTED_EDGE('',*,*,#10234,.T.);
#14822=ORIENTED_EDGE('',*,*,#10235,.T.);
#14823=ORIENTED_EDGE('',*,*,#10230,.F.);
#14824=ORIENTED_EDGE('',*,*,#10236,.T.);
#14825=ORIENTED_EDGE('',*,*,#10237,.T.);
#14826=ORIENTED_EDGE('',*,*,#10238,.T.);
#14827=ORIENTED_EDGE('',*,*,#10234,.F.);
#14828=ORIENTED_EDGE('',*,*,#10239,.T.);
#14829=ORIENTED_EDGE('',*,*,#10240,.T.);
#14830=ORIENTED_EDGE('',*,*,#10241,.T.);
#14831=ORIENTED_EDGE('',*,*,#10237,.F.);
#14832=ORIENTED_EDGE('',*,*,#10242,.T.);
#14833=ORIENTED_EDGE('',*,*,#10200,.T.);
#14834=ORIENTED_EDGE('',*,*,#10243,.T.);
#14835=ORIENTED_EDGE('',*,*,#10240,.F.);
#14836=ORIENTED_EDGE('',*,*,#10244,.T.);
#14837=ORIENTED_EDGE('',*,*,#10245,.T.);
#14838=ORIENTED_EDGE('',*,*,#10246,.T.);
#14839=ORIENTED_EDGE('',*,*,#10247,.T.);
#14840=ORIENTED_EDGE('',*,*,#10248,.T.);
#14841=ORIENTED_EDGE('',*,*,#10247,.F.);
#14842=ORIENTED_EDGE('',*,*,#10249,.F.);
#14843=ORIENTED_EDGE('',*,*,#10163,.F.);
#14844=ORIENTED_EDGE('',*,*,#10250,.F.);
#14845=ORIENTED_EDGE('',*,*,#10207,.F.);
#14846=ORIENTED_EDGE('',*,*,#10250,.T.);
#14847=ORIENTED_EDGE('',*,*,#10162,.F.);
#14848=ORIENTED_EDGE('',*,*,#10251,.F.);
#14849=ORIENTED_EDGE('',*,*,#10210,.F.);
#14850=ORIENTED_EDGE('',*,*,#10252,.F.);
#14851=ORIENTED_EDGE('',*,*,#10188,.F.);
#14852=ORIENTED_EDGE('',*,*,#10253,.F.);
#14853=ORIENTED_EDGE('',*,*,#10209,.F.);
#14854=ORIENTED_EDGE('',*,*,#10253,.T.);
#14855=ORIENTED_EDGE('',*,*,#10187,.F.);
#14856=ORIENTED_EDGE('',*,*,#10254,.F.);
#14857=ORIENTED_EDGE('',*,*,#10206,.F.);
#14858=ORIENTED_EDGE('',*,*,#10249,.T.);
#14859=ORIENTED_EDGE('',*,*,#10204,.F.);
#14860=ORIENTED_EDGE('',*,*,#10255,.F.);
#14861=ORIENTED_EDGE('',*,*,#10164,.F.);
#14862=ORIENTED_EDGE('',*,*,#10251,.T.);
#14863=ORIENTED_EDGE('',*,*,#10178,.F.);
#14864=ORIENTED_EDGE('',*,*,#10256,.F.);
#14865=ORIENTED_EDGE('',*,*,#10213,.F.);
#14866=ORIENTED_EDGE('',*,*,#10252,.T.);
#14867=ORIENTED_EDGE('',*,*,#10212,.F.);
#14868=ORIENTED_EDGE('',*,*,#10257,.F.);
#14869=ORIENTED_EDGE('',*,*,#10189,.F.);
#14870=ORIENTED_EDGE('',*,*,#10254,.T.);
#14871=ORIENTED_EDGE('',*,*,#10186,.F.);
#14872=ORIENTED_EDGE('',*,*,#10258,.F.);
#14873=ORIENTED_EDGE('',*,*,#10203,.F.);
#14874=ORIENTED_EDGE('',*,*,#10255,.T.);
#14875=ORIENTED_EDGE('',*,*,#10201,.F.);
#14876=ORIENTED_EDGE('',*,*,#10259,.F.);
#14877=ORIENTED_EDGE('',*,*,#10165,.F.);
#14878=ORIENTED_EDGE('',*,*,#10256,.T.);
#14879=ORIENTED_EDGE('',*,*,#10177,.F.);
#14880=ORIENTED_EDGE('',*,*,#10260,.F.);
#14881=ORIENTED_EDGE('',*,*,#10216,.F.);
#14882=ORIENTED_EDGE('',*,*,#10257,.T.);
#14883=ORIENTED_EDGE('',*,*,#10215,.F.);
#14884=ORIENTED_EDGE('',*,*,#10261,.F.);
#14885=ORIENTED_EDGE('',*,*,#10190,.F.);
#14886=ORIENTED_EDGE('',*,*,#10258,.T.);
#14887=ORIENTED_EDGE('',*,*,#10185,.F.);
#14888=ORIENTED_EDGE('',*,*,#10262,.F.);
#14889=ORIENTED_EDGE('',*,*,#10199,.F.);
#14890=ORIENTED_EDGE('',*,*,#10259,.T.);
#14891=ORIENTED_EDGE('',*,*,#10244,.F.);
#14892=ORIENTED_EDGE('',*,*,#10263,.F.);
#14893=ORIENTED_EDGE('',*,*,#10166,.F.);
#14894=ORIENTED_EDGE('',*,*,#10260,.T.);
#14895=ORIENTED_EDGE('',*,*,#10176,.F.);
#14896=ORIENTED_EDGE('',*,*,#10264,.F.);
#14897=ORIENTED_EDGE('',*,*,#10219,.F.);
#14898=ORIENTED_EDGE('',*,*,#10261,.T.);
#14899=ORIENTED_EDGE('',*,*,#10218,.F.);
#14900=ORIENTED_EDGE('',*,*,#10265,.F.);
#14901=ORIENTED_EDGE('',*,*,#10191,.F.);
#14902=ORIENTED_EDGE('',*,*,#10262,.T.);
#14903=ORIENTED_EDGE('',*,*,#10184,.F.);
#14904=ORIENTED_EDGE('',*,*,#10266,.F.);
#14905=ORIENTED_EDGE('',*,*,#10243,.F.);
#14906=ORIENTED_EDGE('',*,*,#10263,.T.);
#14907=ORIENTED_EDGE('',*,*,#10242,.F.);
#14908=ORIENTED_EDGE('',*,*,#10267,.F.);
#14909=ORIENTED_EDGE('',*,*,#10167,.F.);
#14910=ORIENTED_EDGE('',*,*,#10264,.T.);
#14911=ORIENTED_EDGE('',*,*,#10175,.F.);
#14912=ORIENTED_EDGE('',*,*,#10268,.F.);
#14913=ORIENTED_EDGE('',*,*,#10222,.F.);
#14914=ORIENTED_EDGE('',*,*,#10265,.T.);
#14915=ORIENTED_EDGE('',*,*,#10221,.F.);
#14916=ORIENTED_EDGE('',*,*,#10269,.F.);
#14917=ORIENTED_EDGE('',*,*,#10192,.F.);
#14918=ORIENTED_EDGE('',*,*,#10266,.T.);
#14919=ORIENTED_EDGE('',*,*,#10183,.F.);
#14920=ORIENTED_EDGE('',*,*,#10270,.F.);
#14921=ORIENTED_EDGE('',*,*,#10241,.F.);
#14922=ORIENTED_EDGE('',*,*,#10267,.T.);
#14923=ORIENTED_EDGE('',*,*,#10239,.F.);
#14924=ORIENTED_EDGE('',*,*,#10271,.F.);
#14925=ORIENTED_EDGE('',*,*,#10168,.F.);
#14926=ORIENTED_EDGE('',*,*,#10268,.T.);
#14927=ORIENTED_EDGE('',*,*,#10174,.F.);
#14928=ORIENTED_EDGE('',*,*,#10272,.F.);
#14929=ORIENTED_EDGE('',*,*,#10225,.F.);
#14930=ORIENTED_EDGE('',*,*,#10273,.F.);
#14931=ORIENTED_EDGE('',*,*,#10223,.F.);
#14932=ORIENTED_EDGE('',*,*,#10274,.F.);
#14933=ORIENTED_EDGE('',*,*,#10228,.F.);
#14934=ORIENTED_EDGE('',*,*,#10269,.T.);
#14935=ORIENTED_EDGE('',*,*,#10224,.F.);
#14936=ORIENTED_EDGE('',*,*,#10275,.F.);
#14937=ORIENTED_EDGE('',*,*,#10193,.F.);
#14938=ORIENTED_EDGE('',*,*,#10270,.T.);
#14939=ORIENTED_EDGE('',*,*,#10182,.F.);
#14940=ORIENTED_EDGE('',*,*,#10276,.F.);
#14941=ORIENTED_EDGE('',*,*,#10238,.F.);
#14942=ORIENTED_EDGE('',*,*,#10271,.T.);
#14943=ORIENTED_EDGE('',*,*,#10236,.F.);
#14944=ORIENTED_EDGE('',*,*,#10277,.F.);
#14945=ORIENTED_EDGE('',*,*,#10169,.F.);
#14946=ORIENTED_EDGE('',*,*,#10272,.T.);
#14947=ORIENTED_EDGE('',*,*,#10173,.T.);
#14948=ORIENTED_EDGE('',*,*,#10278,.F.);
#14949=ORIENTED_EDGE('',*,*,#10274,.T.);
#14950=ORIENTED_EDGE('',*,*,#10275,.T.);
#14951=ORIENTED_EDGE('',*,*,#10273,.T.);
#14952=ORIENTED_EDGE('',*,*,#10279,.F.);
#14953=ORIENTED_EDGE('',*,*,#10194,.T.);
#14954=ORIENTED_EDGE('',*,*,#10276,.T.);
#14955=ORIENTED_EDGE('',*,*,#10181,.F.);
#14956=ORIENTED_EDGE('',*,*,#10280,.F.);
#14957=ORIENTED_EDGE('',*,*,#10235,.F.);
#14958=ORIENTED_EDGE('',*,*,#10277,.T.);
#14959=ORIENTED_EDGE('',*,*,#10233,.F.);
#14960=ORIENTED_EDGE('',*,*,#10281,.F.);
#14961=ORIENTED_EDGE('',*,*,#10170,.F.);
#14962=ORIENTED_EDGE('',*,*,#10278,.T.);
#14963=ORIENTED_EDGE('',*,*,#10172,.F.);
#14964=ORIENTED_EDGE('',*,*,#10282,.F.);
#14965=ORIENTED_EDGE('',*,*,#10229,.F.);
#14966=ORIENTED_EDGE('',*,*,#10279,.T.);
#14967=ORIENTED_EDGE('',*,*,#10227,.F.);
#14968=ORIENTED_EDGE('',*,*,#10283,.F.);
#14969=ORIENTED_EDGE('',*,*,#10195,.F.);
#14970=ORIENTED_EDGE('',*,*,#10280,.T.);
#14971=ORIENTED_EDGE('',*,*,#10180,.F.);
#14972=ORIENTED_EDGE('',*,*,#10284,.F.);
#14973=ORIENTED_EDGE('',*,*,#10231,.F.);
#14974=ORIENTED_EDGE('',*,*,#10171,.T.);
#14975=ORIENTED_EDGE('',*,*,#10281,.T.);
#14976=ORIENTED_EDGE('',*,*,#10285,.F.);
#14977=ORIENTED_EDGE('',*,*,#10282,.T.);
#14978=ORIENTED_EDGE('',*,*,#10196,.T.);
#14979=ORIENTED_EDGE('',*,*,#10283,.T.);
#14980=ORIENTED_EDGE('',*,*,#10286,.F.);
#14981=ORIENTED_EDGE('',*,*,#10284,.T.);
#14982=ORIENTED_EDGE('',*,*,#10285,.T.);
#14983=ORIENTED_EDGE('',*,*,#10232,.F.);
#14984=ORIENTED_EDGE('',*,*,#10286,.T.);
#14985=ORIENTED_EDGE('',*,*,#10226,.F.);
#14986=ORIENTED_EDGE('',*,*,#10248,.F.);
#14987=ORIENTED_EDGE('',*,*,#10287,.T.);
#14988=ORIENTED_EDGE('',*,*,#10197,.F.);
#14989=ORIENTED_EDGE('',*,*,#10287,.F.);
#14990=ORIENTED_EDGE('',*,*,#10245,.F.);
#14991=ORIENTED_EDGE('',*,*,#10246,.F.);
#14992=ORIENTED_EDGE('',*,*,#10288,.T.);
#14993=ORIENTED_EDGE('',*,*,#10179,.F.);
#14994=ORIENTED_EDGE('',*,*,#10288,.F.);
#14995=ORIENTED_EDGE('',*,*,#10289,.T.);
#14996=ORIENTED_EDGE('',*,*,#10290,.T.);
#14997=ORIENTED_EDGE('',*,*,#10291,.T.);
#14998=ORIENTED_EDGE('',*,*,#10292,.T.);
#14999=ORIENTED_EDGE('',*,*,#10293,.T.);
#15000=ORIENTED_EDGE('',*,*,#10294,.T.);
#15001=ORIENTED_EDGE('',*,*,#10295,.T.);
#15002=ORIENTED_EDGE('',*,*,#10296,.T.);
#15003=ORIENTED_EDGE('',*,*,#10297,.F.);
#15004=ORIENTED_EDGE('',*,*,#10298,.T.);
#15005=ORIENTED_EDGE('',*,*,#10299,.T.);
#15006=ORIENTED_EDGE('',*,*,#10300,.T.);
#15007=ORIENTED_EDGE('',*,*,#10301,.F.);
#15008=ORIENTED_EDGE('',*,*,#10302,.T.);
#15009=ORIENTED_EDGE('',*,*,#10297,.T.);
#15010=ORIENTED_EDGE('',*,*,#10303,.T.);
#15011=ORIENTED_EDGE('',*,*,#10304,.F.);
#15012=ORIENTED_EDGE('',*,*,#10305,.T.);
#15013=ORIENTED_EDGE('',*,*,#10301,.T.);
#15014=ORIENTED_EDGE('',*,*,#10306,.T.);
#15015=ORIENTED_EDGE('',*,*,#10307,.F.);
#15016=ORIENTED_EDGE('',*,*,#10308,.T.);
#15017=ORIENTED_EDGE('',*,*,#10304,.T.);
#15018=ORIENTED_EDGE('',*,*,#10309,.T.);
#15019=ORIENTED_EDGE('',*,*,#10310,.F.);
#15020=ORIENTED_EDGE('',*,*,#10311,.T.);
#15021=ORIENTED_EDGE('',*,*,#10307,.T.);
#15022=ORIENTED_EDGE('',*,*,#10312,.T.);
#15023=ORIENTED_EDGE('',*,*,#10313,.F.);
#15024=ORIENTED_EDGE('',*,*,#10314,.T.);
#15025=ORIENTED_EDGE('',*,*,#10310,.T.);
#15026=ORIENTED_EDGE('',*,*,#10315,.T.);
#15027=ORIENTED_EDGE('',*,*,#10316,.F.);
#15028=ORIENTED_EDGE('',*,*,#10317,.T.);
#15029=ORIENTED_EDGE('',*,*,#10313,.T.);
#15030=ORIENTED_EDGE('',*,*,#10318,.T.);
#15031=ORIENTED_EDGE('',*,*,#10319,.F.);
#15032=ORIENTED_EDGE('',*,*,#10320,.T.);
#15033=ORIENTED_EDGE('',*,*,#10316,.T.);
#15034=ORIENTED_EDGE('',*,*,#10321,.T.);
#15035=ORIENTED_EDGE('',*,*,#10322,.F.);
#15036=ORIENTED_EDGE('',*,*,#10323,.T.);
#15037=ORIENTED_EDGE('',*,*,#10319,.T.);
#15038=ORIENTED_EDGE('',*,*,#10324,.T.);
#15039=ORIENTED_EDGE('',*,*,#10325,.F.);
#15040=ORIENTED_EDGE('',*,*,#10326,.T.);
#15041=ORIENTED_EDGE('',*,*,#10322,.T.);
#15042=ORIENTED_EDGE('',*,*,#10327,.T.);
#15043=ORIENTED_EDGE('',*,*,#10328,.F.);
#15044=ORIENTED_EDGE('',*,*,#10329,.T.);
#15045=ORIENTED_EDGE('',*,*,#10325,.T.);
#15046=ORIENTED_EDGE('',*,*,#10330,.T.);
#15047=ORIENTED_EDGE('',*,*,#10331,.T.);
#15048=ORIENTED_EDGE('',*,*,#10332,.T.);
#15049=ORIENTED_EDGE('',*,*,#10328,.T.);
#15050=ORIENTED_EDGE('',*,*,#10333,.T.);
#15051=ORIENTED_EDGE('',*,*,#10334,.T.);
#15052=ORIENTED_EDGE('',*,*,#10335,.T.);
#15053=ORIENTED_EDGE('',*,*,#10336,.T.);
#15054=ORIENTED_EDGE('',*,*,#10337,.T.);
#15055=ORIENTED_EDGE('',*,*,#10338,.T.);
#15056=ORIENTED_EDGE('',*,*,#10339,.T.);
#15057=ORIENTED_EDGE('',*,*,#10340,.T.);
#15058=ORIENTED_EDGE('',*,*,#10341,.F.);
#15059=ORIENTED_EDGE('',*,*,#10342,.T.);
#15060=ORIENTED_EDGE('',*,*,#10343,.F.);
#15061=ORIENTED_EDGE('',*,*,#10344,.T.);
#15062=ORIENTED_EDGE('',*,*,#10345,.F.);
#15063=ORIENTED_EDGE('',*,*,#10346,.T.);
#15064=ORIENTED_EDGE('',*,*,#10347,.T.);
#15065=ORIENTED_EDGE('',*,*,#10348,.T.);
#15066=ORIENTED_EDGE('',*,*,#10349,.T.);
#15067=ORIENTED_EDGE('',*,*,#10350,.T.);
#15068=ORIENTED_EDGE('',*,*,#10351,.T.);
#15069=ORIENTED_EDGE('',*,*,#10352,.T.);
#15070=ORIENTED_EDGE('',*,*,#10353,.T.);
#15071=ORIENTED_EDGE('',*,*,#10354,.T.);
#15072=ORIENTED_EDGE('',*,*,#10355,.T.);
#15073=ORIENTED_EDGE('',*,*,#10356,.T.);
#15074=ORIENTED_EDGE('',*,*,#10357,.T.);
#15075=ORIENTED_EDGE('',*,*,#10358,.T.);
#15076=ORIENTED_EDGE('',*,*,#10359,.T.);
#15077=ORIENTED_EDGE('',*,*,#10360,.F.);
#15078=ORIENTED_EDGE('',*,*,#10361,.T.);
#15079=ORIENTED_EDGE('',*,*,#10362,.F.);
#15080=ORIENTED_EDGE('',*,*,#10363,.T.);
#15081=ORIENTED_EDGE('',*,*,#10364,.F.);
#15082=ORIENTED_EDGE('',*,*,#10365,.T.);
#15083=ORIENTED_EDGE('',*,*,#10366,.T.);
#15084=ORIENTED_EDGE('',*,*,#10367,.T.);
#15085=ORIENTED_EDGE('',*,*,#10368,.T.);
#15086=ORIENTED_EDGE('',*,*,#10369,.T.);
#15087=ORIENTED_EDGE('',*,*,#10370,.T.);
#15088=ORIENTED_EDGE('',*,*,#10371,.T.);
#15089=ORIENTED_EDGE('',*,*,#10372,.T.);
#15090=ORIENTED_EDGE('',*,*,#10373,.T.);
#15091=ORIENTED_EDGE('',*,*,#10374,.T.);
#15092=ORIENTED_EDGE('',*,*,#10375,.T.);
#15093=ORIENTED_EDGE('',*,*,#10376,.T.);
#15094=ORIENTED_EDGE('',*,*,#10377,.T.);
#15095=ORIENTED_EDGE('',*,*,#10378,.T.);
#15096=ORIENTED_EDGE('',*,*,#10379,.T.);
#15097=ORIENTED_EDGE('',*,*,#10378,.F.);
#15098=ORIENTED_EDGE('',*,*,#10380,.F.);
#15099=ORIENTED_EDGE('',*,*,#10371,.F.);
#15100=ORIENTED_EDGE('',*,*,#10381,.F.);
#15101=ORIENTED_EDGE('',*,*,#10314,.F.);
#15102=ORIENTED_EDGE('',*,*,#10381,.T.);
#15103=ORIENTED_EDGE('',*,*,#10370,.F.);
#15104=ORIENTED_EDGE('',*,*,#10382,.F.);
#15105=ORIENTED_EDGE('',*,*,#10311,.F.);
#15106=ORIENTED_EDGE('',*,*,#10383,.F.);
#15107=ORIENTED_EDGE('',*,*,#10353,.F.);
#15108=ORIENTED_EDGE('',*,*,#10384,.F.);
#15109=ORIENTED_EDGE('',*,*,#10312,.F.);
#15110=ORIENTED_EDGE('',*,*,#10384,.T.);
#15111=ORIENTED_EDGE('',*,*,#10352,.F.);
#15112=ORIENTED_EDGE('',*,*,#10385,.F.);
#15113=ORIENTED_EDGE('',*,*,#10315,.F.);
#15114=ORIENTED_EDGE('',*,*,#10380,.T.);
#15115=ORIENTED_EDGE('',*,*,#10317,.F.);
#15116=ORIENTED_EDGE('',*,*,#10386,.F.);
#15117=ORIENTED_EDGE('',*,*,#10372,.F.);
#15118=ORIENTED_EDGE('',*,*,#10382,.T.);
#15119=ORIENTED_EDGE('',*,*,#10369,.F.);
#15120=ORIENTED_EDGE('',*,*,#10387,.F.);
#15121=ORIENTED_EDGE('',*,*,#10308,.F.);
#15122=ORIENTED_EDGE('',*,*,#10383,.T.);
#15123=ORIENTED_EDGE('',*,*,#10309,.F.);
#15124=ORIENTED_EDGE('',*,*,#10388,.F.);
#15125=ORIENTED_EDGE('',*,*,#10354,.F.);
#15126=ORIENTED_EDGE('',*,*,#10385,.T.);
#15127=ORIENTED_EDGE('',*,*,#10351,.F.);
#15128=ORIENTED_EDGE('',*,*,#10389,.F.);
#15129=ORIENTED_EDGE('',*,*,#10318,.F.);
#15130=ORIENTED_EDGE('',*,*,#10386,.T.);
#15131=ORIENTED_EDGE('',*,*,#10320,.F.);
#15132=ORIENTED_EDGE('',*,*,#10390,.F.);
#15133=ORIENTED_EDGE('',*,*,#10373,.F.);
#15134=ORIENTED_EDGE('',*,*,#10387,.T.);
#15135=ORIENTED_EDGE('',*,*,#10368,.F.);
#15136=ORIENTED_EDGE('',*,*,#10391,.F.);
#15137=ORIENTED_EDGE('',*,*,#10305,.F.);
#15138=ORIENTED_EDGE('',*,*,#10388,.T.);
#15139=ORIENTED_EDGE('',*,*,#10306,.F.);
#15140=ORIENTED_EDGE('',*,*,#10392,.F.);
#15141=ORIENTED_EDGE('',*,*,#10355,.F.);
#15142=ORIENTED_EDGE('',*,*,#10389,.T.);
#15143=ORIENTED_EDGE('',*,*,#10350,.F.);
#15144=ORIENTED_EDGE('',*,*,#10393,.F.);
#15145=ORIENTED_EDGE('',*,*,#10321,.F.);
#15146=ORIENTED_EDGE('',*,*,#10390,.T.);
#15147=ORIENTED_EDGE('',*,*,#10323,.F.);
#15148=ORIENTED_EDGE('',*,*,#10394,.F.);
#15149=ORIENTED_EDGE('',*,*,#10374,.F.);
#15150=ORIENTED_EDGE('',*,*,#10391,.T.);
#15151=ORIENTED_EDGE('',*,*,#10367,.F.);
#15152=ORIENTED_EDGE('',*,*,#10395,.F.);
#15153=ORIENTED_EDGE('',*,*,#10302,.F.);
#15154=ORIENTED_EDGE('',*,*,#10392,.T.);
#15155=ORIENTED_EDGE('',*,*,#10303,.F.);
#15156=ORIENTED_EDGE('',*,*,#10396,.F.);
#15157=ORIENTED_EDGE('',*,*,#10338,.F.);
#15158=ORIENTED_EDGE('',*,*,#10393,.T.);
#15159=ORIENTED_EDGE('',*,*,#10349,.F.);
#15160=ORIENTED_EDGE('',*,*,#10397,.F.);
#15161=ORIENTED_EDGE('',*,*,#10324,.F.);
#15162=ORIENTED_EDGE('',*,*,#10394,.T.);
#15163=ORIENTED_EDGE('',*,*,#10326,.F.);
#15164=ORIENTED_EDGE('',*,*,#10398,.F.);
#15165=ORIENTED_EDGE('',*,*,#10357,.F.);
#15166=ORIENTED_EDGE('',*,*,#10395,.T.);
#15167=ORIENTED_EDGE('',*,*,#10366,.F.);
#15168=ORIENTED_EDGE('',*,*,#10399,.F.);
#15169=ORIENTED_EDGE('',*,*,#10298,.F.);
#15170=ORIENTED_EDGE('',*,*,#10400,.F.);
#15171=ORIENTED_EDGE('',*,*,#10299,.F.);
#15172=ORIENTED_EDGE('',*,*,#10401,.F.);
#15173=ORIENTED_EDGE('',*,*,#10293,.F.);
#15174=ORIENTED_EDGE('',*,*,#10396,.T.);
#15175=ORIENTED_EDGE('',*,*,#10300,.F.);
#15176=ORIENTED_EDGE('',*,*,#10402,.F.);
#15177=ORIENTED_EDGE('',*,*,#10339,.F.);
#15178=ORIENTED_EDGE('',*,*,#10397,.T.);
#15179=ORIENTED_EDGE('',*,*,#10348,.F.);
#15180=ORIENTED_EDGE('',*,*,#10403,.F.);
#15181=ORIENTED_EDGE('',*,*,#10327,.F.);
#15182=ORIENTED_EDGE('',*,*,#10398,.T.);
#15183=ORIENTED_EDGE('',*,*,#10329,.F.);
#15184=ORIENTED_EDGE('',*,*,#10404,.F.);
#15185=ORIENTED_EDGE('',*,*,#10358,.F.);
#15186=ORIENTED_EDGE('',*,*,#10401,.T.);
#15187=ORIENTED_EDGE('',*,*,#10399,.T.);
#15188=ORIENTED_EDGE('',*,*,#10405,.F.);
#15189=ORIENTED_EDGE('',*,*,#10402,.T.);
#15190=ORIENTED_EDGE('',*,*,#10400,.T.);
#15191=ORIENTED_EDGE('',*,*,#10406,.F.);
#15192=ORIENTED_EDGE('',*,*,#10403,.T.);
#15193=ORIENTED_EDGE('',*,*,#10347,.F.);
#15194=ORIENTED_EDGE('',*,*,#10407,.F.);
#15195=ORIENTED_EDGE('',*,*,#10330,.F.);
#15196=ORIENTED_EDGE('',*,*,#10404,.T.);
#15197=ORIENTED_EDGE('',*,*,#10332,.F.);
#15198=ORIENTED_EDGE('',*,*,#10408,.F.);
#15199=ORIENTED_EDGE('',*,*,#10359,.F.);
#15200=ORIENTED_EDGE('',*,*,#10405,.T.);
#15201=ORIENTED_EDGE('',*,*,#10365,.F.);
#15202=ORIENTED_EDGE('',*,*,#10409,.F.);
#15203=ORIENTED_EDGE('',*,*,#10294,.F.);
#15204=ORIENTED_EDGE('',*,*,#10410,.F.);
#15205=ORIENTED_EDGE('',*,*,#10295,.F.);
#15206=ORIENTED_EDGE('',*,*,#10411,.F.);
#15207=ORIENTED_EDGE('',*,*,#10289,.F.);
#15208=ORIENTED_EDGE('',*,*,#10406,.T.);
#15209=ORIENTED_EDGE('',*,*,#10296,.F.);
#15210=ORIENTED_EDGE('',*,*,#10412,.F.);
#15211=ORIENTED_EDGE('',*,*,#10340,.F.);
#15212=ORIENTED_EDGE('',*,*,#10407,.T.);
#15213=ORIENTED_EDGE('',*,*,#10346,.F.);
#15214=ORIENTED_EDGE('',*,*,#10413,.F.);
#15215=ORIENTED_EDGE('',*,*,#10333,.F.);
#15216=ORIENTED_EDGE('',*,*,#10414,.F.);
#15217=ORIENTED_EDGE('',*,*,#10331,.F.);
#15218=ORIENTED_EDGE('',*,*,#10415,.F.);
#15219=ORIENTED_EDGE('',*,*,#10336,.F.);
#15220=ORIENTED_EDGE('',*,*,#10408,.T.);
#15221=ORIENTED_EDGE('',*,*,#10414,.T.);
#15222=ORIENTED_EDGE('',*,*,#10416,.F.);
#15223=ORIENTED_EDGE('',*,*,#10360,.T.);
#15224=ORIENTED_EDGE('',*,*,#10409,.T.);
#15225=ORIENTED_EDGE('',*,*,#10364,.T.);
#15226=ORIENTED_EDGE('',*,*,#10417,.F.);
#15227=ORIENTED_EDGE('',*,*,#10411,.T.);
#15228=ORIENTED_EDGE('',*,*,#10412,.T.);
#15229=ORIENTED_EDGE('',*,*,#10410,.T.);
#15230=ORIENTED_EDGE('',*,*,#10418,.F.);
#15231=ORIENTED_EDGE('',*,*,#10341,.T.);
#15232=ORIENTED_EDGE('',*,*,#10413,.T.);
#15233=ORIENTED_EDGE('',*,*,#10345,.T.);
#15234=ORIENTED_EDGE('',*,*,#10419,.F.);
#15235=ORIENTED_EDGE('',*,*,#10415,.T.);
#15236=ORIENTED_EDGE('',*,*,#10416,.T.);
#15237=ORIENTED_EDGE('',*,*,#10335,.F.);
#15238=ORIENTED_EDGE('',*,*,#10420,.F.);
#15239=ORIENTED_EDGE('',*,*,#10361,.F.);
#15240=ORIENTED_EDGE('',*,*,#10417,.T.);
#15241=ORIENTED_EDGE('',*,*,#10363,.F.);
#15242=ORIENTED_EDGE('',*,*,#10421,.F.);
#15243=ORIENTED_EDGE('',*,*,#10290,.F.);
#15244=ORIENTED_EDGE('',*,*,#10418,.T.);
#15245=ORIENTED_EDGE('',*,*,#10292,.F.);
#15246=ORIENTED_EDGE('',*,*,#10422,.F.);
#15247=ORIENTED_EDGE('',*,*,#10342,.F.);
#15248=ORIENTED_EDGE('',*,*,#10419,.T.);
#15249=ORIENTED_EDGE('',*,*,#10344,.F.);
#15250=ORIENTED_EDGE('',*,*,#10423,.F.);
#15251=ORIENTED_EDGE('',*,*,#10337,.F.);
#15252=ORIENTED_EDGE('',*,*,#10362,.T.);
#15253=ORIENTED_EDGE('',*,*,#10420,.T.);
#15254=ORIENTED_EDGE('',*,*,#10424,.F.);
#15255=ORIENTED_EDGE('',*,*,#10421,.T.);
#15256=ORIENTED_EDGE('',*,*,#10343,.T.);
#15257=ORIENTED_EDGE('',*,*,#10422,.T.);
#15258=ORIENTED_EDGE('',*,*,#10425,.F.);
#15259=ORIENTED_EDGE('',*,*,#10423,.T.);
#15260=ORIENTED_EDGE('',*,*,#10424,.T.);
#15261=ORIENTED_EDGE('',*,*,#10334,.F.);
#15262=ORIENTED_EDGE('',*,*,#10425,.T.);
#15263=ORIENTED_EDGE('',*,*,#10291,.F.);
#15264=ORIENTED_EDGE('',*,*,#10379,.F.);
#15265=ORIENTED_EDGE('',*,*,#10426,.T.);
#15266=ORIENTED_EDGE('',*,*,#10375,.F.);
#15267=ORIENTED_EDGE('',*,*,#10426,.F.);
#15268=ORIENTED_EDGE('',*,*,#10376,.F.);
#15269=ORIENTED_EDGE('',*,*,#10377,.F.);
#15270=ORIENTED_EDGE('',*,*,#10427,.T.);
#15271=ORIENTED_EDGE('',*,*,#10356,.F.);
#15272=ORIENTED_EDGE('',*,*,#10427,.F.);
#15273=ORIENTED_EDGE('',*,*,#10428,.T.);
#15274=ORIENTED_EDGE('',*,*,#10429,.T.);
#15275=ORIENTED_EDGE('',*,*,#10430,.T.);
#15276=ORIENTED_EDGE('',*,*,#10429,.F.);
#15277=ORIENTED_EDGE('',*,*,#10430,.F.);
#15278=ORIENTED_EDGE('',*,*,#10431,.F.);
#15279=ORIENTED_EDGE('',*,*,#10432,.F.);
#15280=ORIENTED_EDGE('',*,*,#10433,.T.);
#15281=ORIENTED_EDGE('',*,*,#10434,.T.);
#15282=ORIENTED_EDGE('',*,*,#10435,.F.);
#15283=ORIENTED_EDGE('',*,*,#10436,.F.);
#15284=ORIENTED_EDGE('',*,*,#10437,.T.);
#15285=ORIENTED_EDGE('',*,*,#10432,.T.);
#15286=ORIENTED_EDGE('',*,*,#10438,.F.);
#15287=ORIENTED_EDGE('',*,*,#10439,.F.);
#15288=ORIENTED_EDGE('',*,*,#10440,.T.);
#15289=ORIENTED_EDGE('',*,*,#10436,.T.);
#15290=ORIENTED_EDGE('',*,*,#10441,.F.);
#15291=ORIENTED_EDGE('',*,*,#10434,.F.);
#15292=ORIENTED_EDGE('',*,*,#10442,.T.);
#15293=ORIENTED_EDGE('',*,*,#10439,.T.);
#15294=ORIENTED_EDGE('',*,*,#10433,.F.);
#15295=ORIENTED_EDGE('',*,*,#10437,.F.);
#15296=ORIENTED_EDGE('',*,*,#10440,.F.);
#15297=ORIENTED_EDGE('',*,*,#10442,.F.);
#15298=ORIENTED_EDGE('',*,*,#10428,.F.);
#15299=ORIENTED_EDGE('',*,*,#10431,.T.);
#15300=ORIENTED_EDGE('',*,*,#10441,.T.);
#15301=ORIENTED_EDGE('',*,*,#10438,.T.);
#15302=ORIENTED_EDGE('',*,*,#10435,.T.);
#15303=ORIENTED_EDGE('',*,*,#10443,.T.);
#15304=ORIENTED_EDGE('',*,*,#10444,.T.);
#15305=ORIENTED_EDGE('',*,*,#10445,.T.);
#15306=ORIENTED_EDGE('',*,*,#10446,.T.);
#15307=ORIENTED_EDGE('',*,*,#10447,.T.);
#15308=ORIENTED_EDGE('',*,*,#10448,.T.);
#15309=ORIENTED_EDGE('',*,*,#10447,.F.);
#15310=ORIENTED_EDGE('',*,*,#10449,.T.);
#15311=ORIENTED_EDGE('',*,*,#10450,.T.);
#15312=ORIENTED_EDGE('',*,*,#10450,.F.);
#15313=ORIENTED_EDGE('',*,*,#10451,.T.);
#15314=ORIENTED_EDGE('',*,*,#10444,.F.);
#15315=ORIENTED_EDGE('',*,*,#10451,.F.);
#15316=ORIENTED_EDGE('',*,*,#10448,.F.);
#15317=ORIENTED_EDGE('',*,*,#10452,.T.);
#15318=ORIENTED_EDGE('',*,*,#10449,.F.);
#15319=ORIENTED_EDGE('',*,*,#10452,.F.);
#15320=ORIENTED_EDGE('',*,*,#10445,.F.);
#15321=ORIENTED_EDGE('',*,*,#10446,.F.);
#15322=ORIENTED_EDGE('',*,*,#10453,.T.);
#15323=ORIENTED_EDGE('',*,*,#10443,.F.);
#15324=ORIENTED_EDGE('',*,*,#10453,.F.);
#15325=ORIENTED_EDGE('',*,*,#10454,.F.);
#15326=ORIENTED_EDGE('',*,*,#10455,.F.);
#15327=ORIENTED_EDGE('',*,*,#10456,.F.);
#15328=ORIENTED_EDGE('',*,*,#10457,.F.);
#15329=ORIENTED_EDGE('',*,*,#10458,.F.);
#15330=ORIENTED_EDGE('',*,*,#10459,.F.);
#15331=ORIENTED_EDGE('',*,*,#10460,.F.);
#15332=ORIENTED_EDGE('',*,*,#10461,.F.);
#15333=ORIENTED_EDGE('',*,*,#10462,.F.);
#15334=ORIENTED_EDGE('',*,*,#10463,.F.);
#15335=ORIENTED_EDGE('',*,*,#10464,.F.);
#15336=ORIENTED_EDGE('',*,*,#10465,.F.);
#15337=ORIENTED_EDGE('',*,*,#10466,.T.);
#15338=ORIENTED_EDGE('',*,*,#10467,.T.);
#15339=ORIENTED_EDGE('',*,*,#10468,.T.);
#15340=ORIENTED_EDGE('',*,*,#10466,.F.);
#15341=ORIENTED_EDGE('',*,*,#10469,.F.);
#15342=ORIENTED_EDGE('',*,*,#10470,.F.);
#15343=ORIENTED_EDGE('',*,*,#10471,.F.);
#15344=ORIENTED_EDGE('',*,*,#10472,.F.);
#15345=ORIENTED_EDGE('',*,*,#10473,.F.);
#15346=ORIENTED_EDGE('',*,*,#10474,.F.);
#15347=ORIENTED_EDGE('',*,*,#10475,.F.);
#15348=ORIENTED_EDGE('',*,*,#10476,.F.);
#15349=ORIENTED_EDGE('',*,*,#10477,.F.);
#15350=ORIENTED_EDGE('',*,*,#10478,.F.);
#15351=ORIENTED_EDGE('',*,*,#10479,.T.);
#15352=ORIENTED_EDGE('',*,*,#10467,.F.);
#15353=ORIENTED_EDGE('',*,*,#10468,.F.);
#15354=ORIENTED_EDGE('',*,*,#10480,.T.);
#15355=ORIENTED_EDGE('',*,*,#10478,.T.);
#15356=ORIENTED_EDGE('',*,*,#10480,.F.);
#15357=ORIENTED_EDGE('',*,*,#10481,.T.);
#15358=ORIENTED_EDGE('',*,*,#10482,.T.);
#15359=ORIENTED_EDGE('',*,*,#10483,.T.);
#15360=ORIENTED_EDGE('',*,*,#10484,.T.);
#15361=ORIENTED_EDGE('',*,*,#10483,.F.);
#15362=ORIENTED_EDGE('',*,*,#10484,.F.);
#15363=ORIENTED_EDGE('',*,*,#10485,.T.);
#15364=ORIENTED_EDGE('',*,*,#10481,.F.);
#15365=ORIENTED_EDGE('',*,*,#10485,.F.);
#15366=ORIENTED_EDGE('',*,*,#10454,.T.);
#15367=ORIENTED_EDGE('',*,*,#10486,.F.);
#15368=ORIENTED_EDGE('',*,*,#10487,.T.);
#15369=ORIENTED_EDGE('',*,*,#10488,.T.);
#15370=ORIENTED_EDGE('',*,*,#10455,.T.);
#15371=ORIENTED_EDGE('',*,*,#10488,.F.);
#15372=ORIENTED_EDGE('',*,*,#10489,.T.);
#15373=ORIENTED_EDGE('',*,*,#10490,.T.);
#15374=ORIENTED_EDGE('',*,*,#10456,.T.);
#15375=ORIENTED_EDGE('',*,*,#10490,.F.);
#15376=ORIENTED_EDGE('',*,*,#10491,.T.);
#15377=ORIENTED_EDGE('',*,*,#10492,.T.);
#15378=ORIENTED_EDGE('',*,*,#10457,.T.);
#15379=ORIENTED_EDGE('',*,*,#10492,.F.);
#15380=ORIENTED_EDGE('',*,*,#10493,.T.);
#15381=ORIENTED_EDGE('',*,*,#10494,.T.);
#15382=ORIENTED_EDGE('',*,*,#10458,.T.);
#15383=ORIENTED_EDGE('',*,*,#10494,.F.);
#15384=ORIENTED_EDGE('',*,*,#10495,.T.);
#15385=ORIENTED_EDGE('',*,*,#10496,.T.);
#15386=ORIENTED_EDGE('',*,*,#10459,.T.);
#15387=ORIENTED_EDGE('',*,*,#10496,.F.);
#15388=ORIENTED_EDGE('',*,*,#10497,.T.);
#15389=ORIENTED_EDGE('',*,*,#10498,.T.);
#15390=ORIENTED_EDGE('',*,*,#10460,.T.);
#15391=ORIENTED_EDGE('',*,*,#10498,.F.);
#15392=ORIENTED_EDGE('',*,*,#10499,.T.);
#15393=ORIENTED_EDGE('',*,*,#10500,.T.);
#15394=ORIENTED_EDGE('',*,*,#10461,.T.);
#15395=ORIENTED_EDGE('',*,*,#10500,.F.);
#15396=ORIENTED_EDGE('',*,*,#10501,.T.);
#15397=ORIENTED_EDGE('',*,*,#10502,.T.);
#15398=ORIENTED_EDGE('',*,*,#10462,.T.);
#15399=ORIENTED_EDGE('',*,*,#10502,.F.);
#15400=ORIENTED_EDGE('',*,*,#10503,.T.);
#15401=ORIENTED_EDGE('',*,*,#10504,.T.);
#15402=ORIENTED_EDGE('',*,*,#10463,.T.);
#15403=ORIENTED_EDGE('',*,*,#10504,.F.);
#15404=ORIENTED_EDGE('',*,*,#10505,.T.);
#15405=ORIENTED_EDGE('',*,*,#10506,.T.);
#15406=ORIENTED_EDGE('',*,*,#10464,.T.);
#15407=ORIENTED_EDGE('',*,*,#10506,.F.);
#15408=ORIENTED_EDGE('',*,*,#10507,.T.);
#15409=ORIENTED_EDGE('',*,*,#10508,.T.);
#15410=ORIENTED_EDGE('',*,*,#10469,.T.);
#15411=ORIENTED_EDGE('',*,*,#10465,.T.);
#15412=ORIENTED_EDGE('',*,*,#10508,.F.);
#15413=ORIENTED_EDGE('',*,*,#10509,.T.);
#15414=ORIENTED_EDGE('',*,*,#10510,.T.);
#15415=ORIENTED_EDGE('',*,*,#10470,.T.);
#15416=ORIENTED_EDGE('',*,*,#10510,.F.);
#15417=ORIENTED_EDGE('',*,*,#10511,.T.);
#15418=ORIENTED_EDGE('',*,*,#10512,.T.);
#15419=ORIENTED_EDGE('',*,*,#10471,.T.);
#15420=ORIENTED_EDGE('',*,*,#10512,.F.);
#15421=ORIENTED_EDGE('',*,*,#10513,.T.);
#15422=ORIENTED_EDGE('',*,*,#10514,.T.);
#15423=ORIENTED_EDGE('',*,*,#10472,.T.);
#15424=ORIENTED_EDGE('',*,*,#10514,.F.);
#15425=ORIENTED_EDGE('',*,*,#10515,.T.);
#15426=ORIENTED_EDGE('',*,*,#10516,.T.);
#15427=ORIENTED_EDGE('',*,*,#10473,.T.);
#15428=ORIENTED_EDGE('',*,*,#10516,.F.);
#15429=ORIENTED_EDGE('',*,*,#10517,.T.);
#15430=ORIENTED_EDGE('',*,*,#10518,.T.);
#15431=ORIENTED_EDGE('',*,*,#10474,.T.);
#15432=ORIENTED_EDGE('',*,*,#10518,.F.);
#15433=ORIENTED_EDGE('',*,*,#10519,.T.);
#15434=ORIENTED_EDGE('',*,*,#10520,.T.);
#15435=ORIENTED_EDGE('',*,*,#10475,.T.);
#15436=ORIENTED_EDGE('',*,*,#10520,.F.);
#15437=ORIENTED_EDGE('',*,*,#10521,.T.);
#15438=ORIENTED_EDGE('',*,*,#10522,.T.);
#15439=ORIENTED_EDGE('',*,*,#10476,.T.);
#15440=ORIENTED_EDGE('',*,*,#10522,.F.);
#15441=ORIENTED_EDGE('',*,*,#10523,.T.);
#15442=ORIENTED_EDGE('',*,*,#10524,.T.);
#15443=ORIENTED_EDGE('',*,*,#10477,.T.);
#15444=ORIENTED_EDGE('',*,*,#10524,.F.);
#15445=ORIENTED_EDGE('',*,*,#10525,.T.);
#15446=ORIENTED_EDGE('',*,*,#10486,.T.);
#15447=ORIENTED_EDGE('',*,*,#10487,.F.);
#15448=ORIENTED_EDGE('',*,*,#10525,.F.);
#15449=ORIENTED_EDGE('',*,*,#10523,.F.);
#15450=ORIENTED_EDGE('',*,*,#10521,.F.);
#15451=ORIENTED_EDGE('',*,*,#10519,.F.);
#15452=ORIENTED_EDGE('',*,*,#10517,.F.);
#15453=ORIENTED_EDGE('',*,*,#10515,.F.);
#15454=ORIENTED_EDGE('',*,*,#10513,.F.);
#15455=ORIENTED_EDGE('',*,*,#10511,.F.);
#15456=ORIENTED_EDGE('',*,*,#10509,.F.);
#15457=ORIENTED_EDGE('',*,*,#10507,.F.);
#15458=ORIENTED_EDGE('',*,*,#10505,.F.);
#15459=ORIENTED_EDGE('',*,*,#10503,.F.);
#15460=ORIENTED_EDGE('',*,*,#10501,.F.);
#15461=ORIENTED_EDGE('',*,*,#10499,.F.);
#15462=ORIENTED_EDGE('',*,*,#10497,.F.);
#15463=ORIENTED_EDGE('',*,*,#10495,.F.);
#15464=ORIENTED_EDGE('',*,*,#10493,.F.);
#15465=ORIENTED_EDGE('',*,*,#10491,.F.);
#15466=ORIENTED_EDGE('',*,*,#10489,.F.);
#15467=ORIENTED_EDGE('',*,*,#10479,.F.);
#15468=ORIENTED_EDGE('',*,*,#10526,.T.);
#15469=ORIENTED_EDGE('',*,*,#10482,.F.);
#15470=ORIENTED_EDGE('',*,*,#10526,.F.);
#15471=ORIENTED_EDGE('',*,*,#10527,.T.);
#15472=ORIENTED_EDGE('',*,*,#10528,.T.);
#15473=ORIENTED_EDGE('',*,*,#10529,.F.);
#15474=ORIENTED_EDGE('',*,*,#10530,.T.);
#15475=ORIENTED_EDGE('',*,*,#10529,.T.);
#15476=ORIENTED_EDGE('',*,*,#10531,.T.);
#15477=ORIENTED_EDGE('',*,*,#10527,.F.);
#15478=ORIENTED_EDGE('',*,*,#10532,.T.);
#15479=ORIENTED_EDGE('',*,*,#10533,.T.);
#15480=ORIENTED_EDGE('',*,*,#10534,.T.);
#15481=ORIENTED_EDGE('',*,*,#10535,.T.);
#15482=ORIENTED_EDGE('',*,*,#10536,.T.);
#15483=ORIENTED_EDGE('',*,*,#10537,.T.);
#15484=ORIENTED_EDGE('',*,*,#10538,.T.);
#15485=ORIENTED_EDGE('',*,*,#10539,.T.);
#15486=ORIENTED_EDGE('',*,*,#10540,.T.);
#15487=ORIENTED_EDGE('',*,*,#10541,.T.);
#15488=ORIENTED_EDGE('',*,*,#10542,.T.);
#15489=ORIENTED_EDGE('',*,*,#10543,.T.);
#15490=ORIENTED_EDGE('',*,*,#10544,.T.);
#15491=ORIENTED_EDGE('',*,*,#10545,.T.);
#15492=ORIENTED_EDGE('',*,*,#10546,.T.);
#15493=ORIENTED_EDGE('',*,*,#10547,.T.);
#15494=ORIENTED_EDGE('',*,*,#10548,.T.);
#15495=ORIENTED_EDGE('',*,*,#10549,.T.);
#15496=ORIENTED_EDGE('',*,*,#10547,.F.);
#15497=ORIENTED_EDGE('',*,*,#10550,.T.);
#15498=ORIENTED_EDGE('',*,*,#10551,.T.);
#15499=ORIENTED_EDGE('',*,*,#10552,.T.);
#15500=ORIENTED_EDGE('',*,*,#10553,.T.);
#15501=ORIENTED_EDGE('',*,*,#10554,.T.);
#15502=ORIENTED_EDGE('',*,*,#10552,.F.);
#15503=ORIENTED_EDGE('',*,*,#10555,.T.);
#15504=ORIENTED_EDGE('',*,*,#10556,.T.);
#15505=ORIENTED_EDGE('',*,*,#10557,.T.);
#15506=ORIENTED_EDGE('',*,*,#10558,.T.);
#15507=ORIENTED_EDGE('',*,*,#10559,.T.);
#15508=ORIENTED_EDGE('',*,*,#10557,.F.);
#15509=ORIENTED_EDGE('',*,*,#10560,.T.);
#15510=ORIENTED_EDGE('',*,*,#10561,.T.);
#15511=ORIENTED_EDGE('',*,*,#10562,.T.);
#15512=ORIENTED_EDGE('',*,*,#10563,.T.);
#15513=ORIENTED_EDGE('',*,*,#10564,.T.);
#15514=ORIENTED_EDGE('',*,*,#10562,.F.);
#15515=ORIENTED_EDGE('',*,*,#10565,.F.);
#15516=ORIENTED_EDGE('',*,*,#10539,.F.);
#15517=ORIENTED_EDGE('',*,*,#10566,.F.);
#15518=ORIENTED_EDGE('',*,*,#10528,.F.);
#15519=ORIENTED_EDGE('',*,*,#10566,.T.);
#15520=ORIENTED_EDGE('',*,*,#10540,.F.);
#15521=ORIENTED_EDGE('',*,*,#10565,.T.);
#15522=ORIENTED_EDGE('',*,*,#10531,.F.);
#15523=ORIENTED_EDGE('',*,*,#10541,.F.);
#15524=ORIENTED_EDGE('',*,*,#10567,.T.);
#15525=ORIENTED_EDGE('',*,*,#10548,.F.);
#15526=ORIENTED_EDGE('',*,*,#10549,.F.);
#15527=ORIENTED_EDGE('',*,*,#10567,.F.);
#15528=ORIENTED_EDGE('',*,*,#10542,.F.);
#15529=ORIENTED_EDGE('',*,*,#10568,.T.);
#15530=ORIENTED_EDGE('',*,*,#10553,.F.);
#15531=ORIENTED_EDGE('',*,*,#10554,.F.);
#15532=ORIENTED_EDGE('',*,*,#10568,.F.);
#15533=ORIENTED_EDGE('',*,*,#10543,.F.);
#15534=ORIENTED_EDGE('',*,*,#10569,.T.);
#15535=ORIENTED_EDGE('',*,*,#10558,.F.);
#15536=ORIENTED_EDGE('',*,*,#10559,.F.);
#15537=ORIENTED_EDGE('',*,*,#10569,.F.);
#15538=ORIENTED_EDGE('',*,*,#10544,.F.);
#15539=ORIENTED_EDGE('',*,*,#10570,.T.);
#15540=ORIENTED_EDGE('',*,*,#10563,.F.);
#15541=ORIENTED_EDGE('',*,*,#10564,.F.);
#15542=ORIENTED_EDGE('',*,*,#10570,.F.);
#15543=ORIENTED_EDGE('',*,*,#10571,.F.);
#15544=ORIENTED_EDGE('',*,*,#10530,.F.);
#15545=ORIENTED_EDGE('',*,*,#10572,.F.);
#15546=ORIENTED_EDGE('',*,*,#10533,.F.);
#15547=ORIENTED_EDGE('',*,*,#10572,.T.);
#15548=ORIENTED_EDGE('',*,*,#10532,.F.);
#15549=ORIENTED_EDGE('',*,*,#10571,.T.);
#15550=ORIENTED_EDGE('',*,*,#10534,.F.);
#15551=ORIENTED_EDGE('',*,*,#10545,.F.);
#15552=ORIENTED_EDGE('',*,*,#10546,.F.);
#15553=ORIENTED_EDGE('',*,*,#10573,.T.);
#15554=ORIENTED_EDGE('',*,*,#10535,.F.);
#15555=ORIENTED_EDGE('',*,*,#10573,.F.);
#15556=ORIENTED_EDGE('',*,*,#10550,.F.);
#15557=ORIENTED_EDGE('',*,*,#10551,.F.);
#15558=ORIENTED_EDGE('',*,*,#10574,.T.);
#15559=ORIENTED_EDGE('',*,*,#10536,.F.);
#15560=ORIENTED_EDGE('',*,*,#10574,.F.);
#15561=ORIENTED_EDGE('',*,*,#10555,.F.);
#15562=ORIENTED_EDGE('',*,*,#10556,.F.);
#15563=ORIENTED_EDGE('',*,*,#10575,.T.);
#15564=ORIENTED_EDGE('',*,*,#10537,.F.);
#15565=ORIENTED_EDGE('',*,*,#10575,.F.);
#15566=ORIENTED_EDGE('',*,*,#10560,.F.);
#15567=ORIENTED_EDGE('',*,*,#10561,.F.);
#15568=ORIENTED_EDGE('',*,*,#10576,.T.);
#15569=ORIENTED_EDGE('',*,*,#10538,.F.);
#15570=ORIENTED_EDGE('',*,*,#10576,.F.);
#15571=ORIENTED_EDGE('',*,*,#10577,.T.);
#15572=ORIENTED_EDGE('',*,*,#10578,.T.);
#15573=ORIENTED_EDGE('',*,*,#10579,.T.);
#15574=ORIENTED_EDGE('',*,*,#10580,.T.);
#15575=ORIENTED_EDGE('',*,*,#10581,.T.);
#15576=ORIENTED_EDGE('',*,*,#10582,.T.);
#15577=ORIENTED_EDGE('',*,*,#10583,.T.);
#15578=ORIENTED_EDGE('',*,*,#10584,.T.);
#15579=ORIENTED_EDGE('',*,*,#10585,.T.);
#15580=ORIENTED_EDGE('',*,*,#10586,.T.);
#15581=ORIENTED_EDGE('',*,*,#10587,.F.);
#15582=ORIENTED_EDGE('',*,*,#10588,.T.);
#15583=ORIENTED_EDGE('',*,*,#10587,.T.);
#15584=ORIENTED_EDGE('',*,*,#10589,.T.);
#15585=ORIENTED_EDGE('',*,*,#10590,.F.);
#15586=ORIENTED_EDGE('',*,*,#10591,.T.);
#15587=ORIENTED_EDGE('',*,*,#10590,.T.);
#15588=ORIENTED_EDGE('',*,*,#10592,.T.);
#15589=ORIENTED_EDGE('',*,*,#10593,.T.);
#15590=ORIENTED_EDGE('',*,*,#10594,.T.);
#15591=ORIENTED_EDGE('',*,*,#10595,.T.);
#15592=ORIENTED_EDGE('',*,*,#10596,.T.);
#15593=ORIENTED_EDGE('',*,*,#10597,.T.);
#15594=ORIENTED_EDGE('',*,*,#10598,.T.);
#15595=ORIENTED_EDGE('',*,*,#10599,.T.);
#15596=ORIENTED_EDGE('',*,*,#10600,.T.);
#15597=ORIENTED_EDGE('',*,*,#10601,.F.);
#15598=ORIENTED_EDGE('',*,*,#10602,.T.);
#15599=ORIENTED_EDGE('',*,*,#10601,.T.);
#15600=ORIENTED_EDGE('',*,*,#10603,.T.);
#15601=ORIENTED_EDGE('',*,*,#10577,.F.);
#15602=ORIENTED_EDGE('',*,*,#10604,.T.);
#15603=ORIENTED_EDGE('',*,*,#10605,.T.);
#15604=ORIENTED_EDGE('',*,*,#10606,.T.);
#15605=ORIENTED_EDGE('',*,*,#10607,.T.);
#15606=ORIENTED_EDGE('',*,*,#10608,.T.);
#15607=ORIENTED_EDGE('',*,*,#10609,.T.);
#15608=ORIENTED_EDGE('',*,*,#10610,.T.);
#15609=ORIENTED_EDGE('',*,*,#10611,.T.);
#15610=ORIENTED_EDGE('',*,*,#10612,.T.);
#15611=ORIENTED_EDGE('',*,*,#10613,.T.);
#15612=ORIENTED_EDGE('',*,*,#10614,.T.);
#15613=ORIENTED_EDGE('',*,*,#10615,.T.);
#15614=ORIENTED_EDGE('',*,*,#10616,.T.);
#15615=ORIENTED_EDGE('',*,*,#10617,.T.);
#15616=ORIENTED_EDGE('',*,*,#10618,.T.);
#15617=ORIENTED_EDGE('',*,*,#10619,.T.);
#15618=ORIENTED_EDGE('',*,*,#10620,.T.);
#15619=ORIENTED_EDGE('',*,*,#10621,.T.);
#15620=ORIENTED_EDGE('',*,*,#10622,.T.);
#15621=ORIENTED_EDGE('',*,*,#10623,.T.);
#15622=ORIENTED_EDGE('',*,*,#10624,.T.);
#15623=ORIENTED_EDGE('',*,*,#10625,.T.);
#15624=ORIENTED_EDGE('',*,*,#10626,.T.);
#15625=ORIENTED_EDGE('',*,*,#10627,.T.);
#15626=ORIENTED_EDGE('',*,*,#10628,.T.);
#15627=ORIENTED_EDGE('',*,*,#10629,.T.);
#15628=ORIENTED_EDGE('',*,*,#10630,.T.);
#15629=ORIENTED_EDGE('',*,*,#10631,.T.);
#15630=ORIENTED_EDGE('',*,*,#10629,.F.);
#15631=ORIENTED_EDGE('',*,*,#10632,.F.);
#15632=ORIENTED_EDGE('',*,*,#10614,.F.);
#15633=ORIENTED_EDGE('',*,*,#10633,.F.);
#15634=ORIENTED_EDGE('',*,*,#10595,.F.);
#15635=ORIENTED_EDGE('',*,*,#10634,.F.);
#15636=ORIENTED_EDGE('',*,*,#10632,.T.);
#15637=ORIENTED_EDGE('',*,*,#10635,.F.);
#15638=ORIENTED_EDGE('',*,*,#10636,.F.);
#15639=ORIENTED_EDGE('',*,*,#10633,.T.);
#15640=ORIENTED_EDGE('',*,*,#10637,.F.);
#15641=ORIENTED_EDGE('',*,*,#10635,.T.);
#15642=ORIENTED_EDGE('',*,*,#10598,.F.);
#15643=ORIENTED_EDGE('',*,*,#10638,.F.);
#15644=ORIENTED_EDGE('',*,*,#10599,.F.);
#15645=ORIENTED_EDGE('',*,*,#10634,.T.);
#15646=ORIENTED_EDGE('',*,*,#10602,.F.);
#15647=ORIENTED_EDGE('',*,*,#10639,.F.);
#15648=ORIENTED_EDGE('',*,*,#10606,.F.);
#15649=ORIENTED_EDGE('',*,*,#10605,.F.);
#15650=ORIENTED_EDGE('',*,*,#10637,.T.);
#15651=ORIENTED_EDGE('',*,*,#10613,.F.);
#15652=ORIENTED_EDGE('',*,*,#10640,.F.);
#15653=ORIENTED_EDGE('',*,*,#10594,.F.);
#15654=ORIENTED_EDGE('',*,*,#10636,.T.);
#15655=ORIENTED_EDGE('',*,*,#10593,.F.);
#15656=ORIENTED_EDGE('',*,*,#10641,.F.);
#15657=ORIENTED_EDGE('',*,*,#10596,.F.);
#15658=ORIENTED_EDGE('',*,*,#10642,.F.);
#15659=ORIENTED_EDGE('',*,*,#10597,.F.);
#15660=ORIENTED_EDGE('',*,*,#10643,.F.);
#15661=ORIENTED_EDGE('',*,*,#10623,.F.);
#15662=ORIENTED_EDGE('',*,*,#10638,.T.);
#15663=ORIENTED_EDGE('',*,*,#10642,.T.);
#15664=ORIENTED_EDGE('',*,*,#10644,.F.);
#15665=ORIENTED_EDGE('',*,*,#10639,.T.);
#15666=ORIENTED_EDGE('',*,*,#10604,.F.);
#15667=ORIENTED_EDGE('',*,*,#10645,.F.);
#15668=ORIENTED_EDGE('',*,*,#10607,.F.);
#15669=ORIENTED_EDGE('',*,*,#10640,.T.);
#15670=ORIENTED_EDGE('',*,*,#10612,.F.);
#15671=ORIENTED_EDGE('',*,*,#10646,.F.);
#15672=ORIENTED_EDGE('',*,*,#10591,.F.);
#15673=ORIENTED_EDGE('',*,*,#10643,.T.);
#15674=ORIENTED_EDGE('',*,*,#10641,.T.);
#15675=ORIENTED_EDGE('',*,*,#10647,.F.);
#15676=ORIENTED_EDGE('',*,*,#10644,.T.);
#15677=ORIENTED_EDGE('',*,*,#10622,.F.);
#15678=ORIENTED_EDGE('',*,*,#10621,.F.);
#15679=ORIENTED_EDGE('',*,*,#10648,.F.);
#15680=ORIENTED_EDGE('',*,*,#10600,.F.);
#15681=ORIENTED_EDGE('',*,*,#10645,.T.);
#15682=ORIENTED_EDGE('',*,*,#10580,.F.);
#15683=ORIENTED_EDGE('',*,*,#10649,.F.);
#15684=ORIENTED_EDGE('',*,*,#10609,.F.);
#15685=ORIENTED_EDGE('',*,*,#10608,.F.);
#15686=ORIENTED_EDGE('',*,*,#10650,.F.);
#15687=ORIENTED_EDGE('',*,*,#10610,.F.);
#15688=ORIENTED_EDGE('',*,*,#10651,.F.);
#15689=ORIENTED_EDGE('',*,*,#10652,.F.);
#15690=ORIENTED_EDGE('',*,*,#10583,.F.);
#15691=ORIENTED_EDGE('',*,*,#10646,.T.);
#15692=ORIENTED_EDGE('',*,*,#10611,.F.);
#15693=ORIENTED_EDGE('',*,*,#10653,.F.);
#15694=ORIENTED_EDGE('',*,*,#10588,.F.);
#15695=ORIENTED_EDGE('',*,*,#10647,.T.);
#15696=ORIENTED_EDGE('',*,*,#10592,.F.);
#15697=ORIENTED_EDGE('',*,*,#10654,.F.);
#15698=ORIENTED_EDGE('',*,*,#10624,.F.);
#15699=ORIENTED_EDGE('',*,*,#10648,.T.);
#15700=ORIENTED_EDGE('',*,*,#10620,.F.);
#15701=ORIENTED_EDGE('',*,*,#10655,.F.);
#15702=ORIENTED_EDGE('',*,*,#10603,.F.);
#15703=ORIENTED_EDGE('',*,*,#10652,.T.);
#15704=ORIENTED_EDGE('',*,*,#10656,.F.);
#15705=ORIENTED_EDGE('',*,*,#10656,.T.);
#15706=ORIENTED_EDGE('',*,*,#10651,.T.);
#15707=ORIENTED_EDGE('',*,*,#10649,.T.);
#15708=ORIENTED_EDGE('',*,*,#10657,.F.);
#15709=ORIENTED_EDGE('',*,*,#10653,.T.);
#15710=ORIENTED_EDGE('',*,*,#10650,.T.);
#15711=ORIENTED_EDGE('',*,*,#10658,.F.);
#15712=ORIENTED_EDGE('',*,*,#10654,.T.);
#15713=ORIENTED_EDGE('',*,*,#10589,.F.);
#15714=ORIENTED_EDGE('',*,*,#10659,.F.);
#15715=ORIENTED_EDGE('',*,*,#10625,.F.);
#15716=ORIENTED_EDGE('',*,*,#10655,.T.);
#15717=ORIENTED_EDGE('',*,*,#10619,.F.);
#15718=ORIENTED_EDGE('',*,*,#10618,.F.);
#15719=ORIENTED_EDGE('',*,*,#10660,.F.);
#15720=ORIENTED_EDGE('',*,*,#10578,.F.);
#15721=ORIENTED_EDGE('',*,*,#10657,.T.);
#15722=ORIENTED_EDGE('',*,*,#10579,.F.);
#15723=ORIENTED_EDGE('',*,*,#10661,.F.);
#15724=ORIENTED_EDGE('',*,*,#10584,.F.);
#15725=ORIENTED_EDGE('',*,*,#10658,.T.);
#15726=ORIENTED_EDGE('',*,*,#10582,.F.);
#15727=ORIENTED_EDGE('',*,*,#10662,.F.);
#15728=ORIENTED_EDGE('',*,*,#10585,.F.);
#15729=ORIENTED_EDGE('',*,*,#10659,.T.);
#15730=ORIENTED_EDGE('',*,*,#10586,.F.);
#15731=ORIENTED_EDGE('',*,*,#10663,.F.);
#15732=ORIENTED_EDGE('',*,*,#10616,.F.);
#15733=ORIENTED_EDGE('',*,*,#10661,.T.);
#15734=ORIENTED_EDGE('',*,*,#10660,.T.);
#15735=ORIENTED_EDGE('',*,*,#10664,.F.);
#15736=ORIENTED_EDGE('',*,*,#10663,.T.);
#15737=ORIENTED_EDGE('',*,*,#10662,.T.);
#15738=ORIENTED_EDGE('',*,*,#10665,.F.);
#15739=ORIENTED_EDGE('',*,*,#10664,.T.);
#15740=ORIENTED_EDGE('',*,*,#10617,.F.);
#15741=ORIENTED_EDGE('',*,*,#10665,.T.);
#15742=ORIENTED_EDGE('',*,*,#10581,.F.);
#15743=ORIENTED_EDGE('',*,*,#10627,.F.);
#15744=ORIENTED_EDGE('',*,*,#10628,.F.);
#15745=ORIENTED_EDGE('',*,*,#10666,.T.);
#15746=ORIENTED_EDGE('',*,*,#10626,.F.);
#15747=ORIENTED_EDGE('',*,*,#10666,.F.);
#15748=ORIENTED_EDGE('',*,*,#10615,.F.);
#15749=ORIENTED_EDGE('',*,*,#10667,.T.);
#15750=ORIENTED_EDGE('',*,*,#10630,.F.);
#15751=ORIENTED_EDGE('',*,*,#10631,.F.);
#15752=ORIENTED_EDGE('',*,*,#10667,.F.);
#15753=ORIENTED_EDGE('',*,*,#10668,.F.);
#15754=ORIENTED_EDGE('',*,*,#10669,.F.);
#15755=ORIENTED_EDGE('',*,*,#10670,.T.);
#15756=ORIENTED_EDGE('',*,*,#10671,.F.);
#15757=ORIENTED_EDGE('',*,*,#10672,.F.);
#15758=ORIENTED_EDGE('',*,*,#10673,.F.);
#15759=ORIENTED_EDGE('',*,*,#10674,.F.);
#15760=ORIENTED_EDGE('',*,*,#10675,.F.);
#15761=ORIENTED_EDGE('',*,*,#10676,.F.);
#15762=ORIENTED_EDGE('',*,*,#10677,.F.);
#15763=ORIENTED_EDGE('',*,*,#10678,.F.);
#15764=ORIENTED_EDGE('',*,*,#10679,.F.);
#15765=ORIENTED_EDGE('',*,*,#10680,.T.);
#15766=ORIENTED_EDGE('',*,*,#10681,.F.);
#15767=ORIENTED_EDGE('',*,*,#10682,.F.);
#15768=ORIENTED_EDGE('',*,*,#10683,.F.);
#15769=ORIENTED_EDGE('',*,*,#10684,.F.);
#15770=ORIENTED_EDGE('',*,*,#10685,.F.);
#15771=ORIENTED_EDGE('',*,*,#10686,.F.);
#15772=ORIENTED_EDGE('',*,*,#10687,.F.);
#15773=ORIENTED_EDGE('',*,*,#10688,.F.);
#15774=ORIENTED_EDGE('',*,*,#10689,.F.);
#15775=ORIENTED_EDGE('',*,*,#10690,.T.);
#15776=ORIENTED_EDGE('',*,*,#10691,.F.);
#15777=ORIENTED_EDGE('',*,*,#10692,.F.);
#15778=ORIENTED_EDGE('',*,*,#10693,.F.);
#15779=ORIENTED_EDGE('',*,*,#10694,.F.);
#15780=ORIENTED_EDGE('',*,*,#10695,.F.);
#15781=ORIENTED_EDGE('',*,*,#10696,.F.);
#15782=ORIENTED_EDGE('',*,*,#10697,.F.);
#15783=ORIENTED_EDGE('',*,*,#10698,.F.);
#15784=ORIENTED_EDGE('',*,*,#10699,.F.);
#15785=ORIENTED_EDGE('',*,*,#10700,.T.);
#15786=ORIENTED_EDGE('',*,*,#10701,.F.);
#15787=ORIENTED_EDGE('',*,*,#10702,.F.);
#15788=ORIENTED_EDGE('',*,*,#10703,.F.);
#15789=ORIENTED_EDGE('',*,*,#10704,.F.);
#15790=ORIENTED_EDGE('',*,*,#10705,.F.);
#15791=ORIENTED_EDGE('',*,*,#10706,.F.);
#15792=ORIENTED_EDGE('',*,*,#10707,.F.);
#15793=ORIENTED_EDGE('',*,*,#10708,.F.);
#15794=ORIENTED_EDGE('',*,*,#10709,.F.);
#15795=ORIENTED_EDGE('',*,*,#10710,.T.);
#15796=ORIENTED_EDGE('',*,*,#10711,.F.);
#15797=ORIENTED_EDGE('',*,*,#10712,.F.);
#15798=ORIENTED_EDGE('',*,*,#10713,.F.);
#15799=ORIENTED_EDGE('',*,*,#10714,.F.);
#15800=ORIENTED_EDGE('',*,*,#10715,.F.);
#15801=ORIENTED_EDGE('',*,*,#10716,.F.);
#15802=ORIENTED_EDGE('',*,*,#10717,.F.);
#15803=ORIENTED_EDGE('',*,*,#10718,.F.);
#15804=ORIENTED_EDGE('',*,*,#10719,.T.);
#15805=ORIENTED_EDGE('',*,*,#10720,.T.);
#15806=ORIENTED_EDGE('',*,*,#10721,.T.);
#15807=ORIENTED_EDGE('',*,*,#10722,.T.);
#15808=ORIENTED_EDGE('',*,*,#10723,.T.);
#15809=ORIENTED_EDGE('',*,*,#10724,.T.);
#15810=ORIENTED_EDGE('',*,*,#10725,.T.);
#15811=ORIENTED_EDGE('',*,*,#10726,.T.);
#15812=ORIENTED_EDGE('',*,*,#10725,.F.);
#15813=ORIENTED_EDGE('',*,*,#10727,.T.);
#15814=ORIENTED_EDGE('',*,*,#10728,.T.);
#15815=ORIENTED_EDGE('',*,*,#10729,.T.);
#15816=ORIENTED_EDGE('',*,*,#10730,.T.);
#15817=ORIENTED_EDGE('',*,*,#10731,.T.);
#15818=ORIENTED_EDGE('',*,*,#10732,.T.);
#15819=ORIENTED_EDGE('',*,*,#10733,.T.);
#15820=ORIENTED_EDGE('',*,*,#10734,.T.);
#15821=ORIENTED_EDGE('',*,*,#10735,.T.);
#15822=ORIENTED_EDGE('',*,*,#10736,.T.);
#15823=ORIENTED_EDGE('',*,*,#10737,.F.);
#15824=ORIENTED_EDGE('',*,*,#10738,.T.);
#15825=ORIENTED_EDGE('',*,*,#10739,.F.);
#15826=ORIENTED_EDGE('',*,*,#10740,.T.);
#15827=ORIENTED_EDGE('',*,*,#10741,.T.);
#15828=ORIENTED_EDGE('',*,*,#10742,.T.);
#15829=ORIENTED_EDGE('',*,*,#10743,.F.);
#15830=ORIENTED_EDGE('',*,*,#10744,.T.);
#15831=ORIENTED_EDGE('',*,*,#10745,.T.);
#15832=ORIENTED_EDGE('',*,*,#10746,.T.);
#15833=ORIENTED_EDGE('',*,*,#10747,.T.);
#15834=ORIENTED_EDGE('',*,*,#10748,.T.);
#15835=ORIENTED_EDGE('',*,*,#10724,.F.);
#15836=ORIENTED_EDGE('',*,*,#10749,.T.);
#15837=ORIENTED_EDGE('',*,*,#10750,.T.);
#15838=ORIENTED_EDGE('',*,*,#10751,.T.);
#15839=ORIENTED_EDGE('',*,*,#10752,.T.);
#15840=ORIENTED_EDGE('',*,*,#10753,.T.);
#15841=ORIENTED_EDGE('',*,*,#10737,.T.);
#15842=ORIENTED_EDGE('',*,*,#10754,.T.);
#15843=ORIENTED_EDGE('',*,*,#10755,.T.);
#15844=ORIENTED_EDGE('',*,*,#10756,.T.);
#15845=ORIENTED_EDGE('',*,*,#10757,.T.);
#15846=ORIENTED_EDGE('',*,*,#10758,.F.);
#15847=ORIENTED_EDGE('',*,*,#10759,.F.);
#15848=ORIENTED_EDGE('',*,*,#10760,.F.);
#15849=ORIENTED_EDGE('',*,*,#10761,.F.);
#15850=ORIENTED_EDGE('',*,*,#10762,.F.);
#15851=ORIENTED_EDGE('',*,*,#10763,.T.);
#15852=ORIENTED_EDGE('',*,*,#10764,.T.);
#15853=ORIENTED_EDGE('',*,*,#10765,.T.);
#15854=ORIENTED_EDGE('',*,*,#10763,.F.);
#15855=ORIENTED_EDGE('',*,*,#10766,.F.);
#15856=ORIENTED_EDGE('',*,*,#10709,.T.);
#15857=ORIENTED_EDGE('',*,*,#10767,.T.);
#15858=ORIENTED_EDGE('',*,*,#10699,.T.);
#15859=ORIENTED_EDGE('',*,*,#10768,.T.);
#15860=ORIENTED_EDGE('',*,*,#10689,.T.);
#15861=ORIENTED_EDGE('',*,*,#10769,.T.);
#15862=ORIENTED_EDGE('',*,*,#10679,.T.);
#15863=ORIENTED_EDGE('',*,*,#10770,.T.);
#15864=ORIENTED_EDGE('',*,*,#10669,.T.);
#15865=ORIENTED_EDGE('',*,*,#10771,.T.);
#15866=ORIENTED_EDGE('',*,*,#10772,.T.);
#15867=ORIENTED_EDGE('',*,*,#10773,.T.);
#15868=ORIENTED_EDGE('',*,*,#10774,.F.);
#15869=ORIENTED_EDGE('',*,*,#10775,.T.);
#15870=ORIENTED_EDGE('',*,*,#10776,.T.);
#15871=ORIENTED_EDGE('',*,*,#10777,.T.);
#15872=ORIENTED_EDGE('',*,*,#10772,.F.);
#15873=ORIENTED_EDGE('',*,*,#10778,.T.);
#15874=ORIENTED_EDGE('',*,*,#10779,.T.);
#15875=ORIENTED_EDGE('',*,*,#10780,.T.);
#15876=ORIENTED_EDGE('',*,*,#10781,.F.);
#15877=ORIENTED_EDGE('',*,*,#10782,.T.);
#15878=ORIENTED_EDGE('',*,*,#10781,.T.);
#15879=ORIENTED_EDGE('',*,*,#10783,.T.);
#15880=ORIENTED_EDGE('',*,*,#10784,.F.);
#15881=ORIENTED_EDGE('',*,*,#10785,.T.);
#15882=ORIENTED_EDGE('',*,*,#10784,.T.);
#15883=ORIENTED_EDGE('',*,*,#10786,.T.);
#15884=ORIENTED_EDGE('',*,*,#10776,.F.);
#15885=ORIENTED_EDGE('',*,*,#10787,.T.);
#15886=ORIENTED_EDGE('',*,*,#10788,.T.);
#15887=ORIENTED_EDGE('',*,*,#10789,.T.);
#15888=ORIENTED_EDGE('',*,*,#10790,.T.);
#15889=ORIENTED_EDGE('',*,*,#10791,.T.);
#15890=ORIENTED_EDGE('',*,*,#10792,.T.);
#15891=ORIENTED_EDGE('',*,*,#10793,.T.);
#15892=ORIENTED_EDGE('',*,*,#10794,.T.);
#15893=ORIENTED_EDGE('',*,*,#10795,.T.);
#15894=ORIENTED_EDGE('',*,*,#10796,.T.);
#15895=ORIENTED_EDGE('',*,*,#10797,.T.);
#15896=ORIENTED_EDGE('',*,*,#10798,.F.);
#15897=ORIENTED_EDGE('',*,*,#10799,.F.);
#15898=ORIENTED_EDGE('',*,*,#10800,.T.);
#15899=ORIENTED_EDGE('',*,*,#10801,.T.);
#15900=ORIENTED_EDGE('',*,*,#10802,.T.);
#15901=ORIENTED_EDGE('',*,*,#10803,.T.);
#15902=ORIENTED_EDGE('',*,*,#10804,.T.);
#15903=ORIENTED_EDGE('',*,*,#10805,.T.);
#15904=ORIENTED_EDGE('',*,*,#10806,.T.);
#15905=ORIENTED_EDGE('',*,*,#10807,.T.);
#15906=ORIENTED_EDGE('',*,*,#10808,.T.);
#15907=ORIENTED_EDGE('',*,*,#10809,.T.);
#15908=ORIENTED_EDGE('',*,*,#10810,.T.);
#15909=ORIENTED_EDGE('',*,*,#10811,.T.);
#15910=ORIENTED_EDGE('',*,*,#10812,.T.);
#15911=ORIENTED_EDGE('',*,*,#10813,.T.);
#15912=ORIENTED_EDGE('',*,*,#10814,.T.);
#15913=ORIENTED_EDGE('',*,*,#10815,.T.);
#15914=ORIENTED_EDGE('',*,*,#10816,.T.);
#15915=ORIENTED_EDGE('',*,*,#10817,.F.);
#15916=ORIENTED_EDGE('',*,*,#10818,.T.);
#15917=ORIENTED_EDGE('',*,*,#10817,.T.);
#15918=ORIENTED_EDGE('',*,*,#10819,.T.);
#15919=ORIENTED_EDGE('',*,*,#10815,.F.);
#15920=ORIENTED_EDGE('',*,*,#10820,.T.);
#15921=ORIENTED_EDGE('',*,*,#10818,.F.);
#15922=ORIENTED_EDGE('',*,*,#10820,.F.);
#15923=ORIENTED_EDGE('',*,*,#10821,.T.);
#15924=ORIENTED_EDGE('',*,*,#10822,.T.);
#15925=ORIENTED_EDGE('',*,*,#10823,.T.);
#15926=ORIENTED_EDGE('',*,*,#10824,.F.);
#15927=ORIENTED_EDGE('',*,*,#10825,.T.);
#15928=ORIENTED_EDGE('',*,*,#10826,.T.);
#15929=ORIENTED_EDGE('',*,*,#10827,.F.);
#15930=ORIENTED_EDGE('',*,*,#10734,.F.);
#15931=ORIENTED_EDGE('',*,*,#10828,.F.);
#15932=ORIENTED_EDGE('',*,*,#10829,.T.);
#15933=ORIENTED_EDGE('',*,*,#10830,.T.);
#15934=ORIENTED_EDGE('',*,*,#10831,.F.);
#15935=ORIENTED_EDGE('',*,*,#10832,.T.);
#15936=ORIENTED_EDGE('',*,*,#10833,.T.);
#15937=ORIENTED_EDGE('',*,*,#10834,.T.);
#15938=ORIENTED_EDGE('',*,*,#10835,.T.);
#15939=ORIENTED_EDGE('',*,*,#10836,.T.);
#15940=ORIENTED_EDGE('',*,*,#10837,.T.);
#15941=ORIENTED_EDGE('',*,*,#10838,.T.);
#15942=ORIENTED_EDGE('',*,*,#10836,.F.);
#15943=ORIENTED_EDGE('',*,*,#10839,.T.);
#15944=ORIENTED_EDGE('',*,*,#10840,.T.);
#15945=ORIENTED_EDGE('',*,*,#10841,.T.);
#15946=ORIENTED_EDGE('',*,*,#10842,.T.);
#15947=ORIENTED_EDGE('',*,*,#10843,.T.);
#15948=ORIENTED_EDGE('',*,*,#10844,.T.);
#15949=ORIENTED_EDGE('',*,*,#10779,.F.);
#15950=ORIENTED_EDGE('',*,*,#10845,.T.);
#15951=ORIENTED_EDGE('',*,*,#10846,.T.);
#15952=ORIENTED_EDGE('',*,*,#10847,.F.);
#15953=ORIENTED_EDGE('',*,*,#10848,.T.);
#15954=ORIENTED_EDGE('',*,*,#10849,.T.);
#15955=ORIENTED_EDGE('',*,*,#10850,.T.);
#15956=ORIENTED_EDGE('',*,*,#10851,.T.);
#15957=ORIENTED_EDGE('',*,*,#10852,.T.);
#15958=ORIENTED_EDGE('',*,*,#10853,.T.);
#15959=ORIENTED_EDGE('',*,*,#10854,.T.);
#15960=ORIENTED_EDGE('',*,*,#10855,.F.);
#15961=ORIENTED_EDGE('',*,*,#10856,.T.);
#15962=ORIENTED_EDGE('',*,*,#10857,.T.);
#15963=ORIENTED_EDGE('',*,*,#10774,.T.);
#15964=ORIENTED_EDGE('',*,*,#10761,.T.);
#15965=ORIENTED_EDGE('',*,*,#10858,.T.);
#15966=ORIENTED_EDGE('',*,*,#10859,.T.);
#15967=ORIENTED_EDGE('',*,*,#10860,.T.);
#15968=ORIENTED_EDGE('',*,*,#10861,.T.);
#15969=ORIENTED_EDGE('',*,*,#10862,.T.);
#15970=ORIENTED_EDGE('',*,*,#10863,.T.);
#15971=ORIENTED_EDGE('',*,*,#10864,.T.);
#15972=ORIENTED_EDGE('',*,*,#10758,.T.);
#15973=ORIENTED_EDGE('',*,*,#10865,.T.);
#15974=ORIENTED_EDGE('',*,*,#10866,.T.);
#15975=ORIENTED_EDGE('',*,*,#10867,.T.);
#15976=ORIENTED_EDGE('',*,*,#10868,.T.);
#15977=ORIENTED_EDGE('',*,*,#10869,.T.);
#15978=ORIENTED_EDGE('',*,*,#10870,.T.);
#15979=ORIENTED_EDGE('',*,*,#10871,.T.);
#15980=ORIENTED_EDGE('',*,*,#10872,.T.);
#15981=ORIENTED_EDGE('',*,*,#10760,.T.);
#15982=ORIENTED_EDGE('',*,*,#10873,.T.);
#15983=ORIENTED_EDGE('',*,*,#10874,.T.);
#15984=ORIENTED_EDGE('',*,*,#10875,.T.);
#15985=ORIENTED_EDGE('',*,*,#10876,.T.);
#15986=ORIENTED_EDGE('',*,*,#10877,.T.);
#15987=ORIENTED_EDGE('',*,*,#10766,.T.);
#15988=ORIENTED_EDGE('',*,*,#10762,.T.);
#15989=ORIENTED_EDGE('',*,*,#10878,.T.);
#15990=ORIENTED_EDGE('',*,*,#10879,.T.);
#15991=ORIENTED_EDGE('',*,*,#10880,.T.);
#15992=ORIENTED_EDGE('',*,*,#10881,.T.);
#15993=ORIENTED_EDGE('',*,*,#10882,.T.);
#15994=ORIENTED_EDGE('',*,*,#10873,.F.);
#15995=ORIENTED_EDGE('',*,*,#10759,.T.);
#15996=ORIENTED_EDGE('',*,*,#10883,.T.);
#15997=ORIENTED_EDGE('',*,*,#10884,.T.);
#15998=ORIENTED_EDGE('',*,*,#10885,.T.);
#15999=ORIENTED_EDGE('',*,*,#10677,.T.);
#16000=ORIENTED_EDGE('',*,*,#10676,.T.);
#16001=ORIENTED_EDGE('',*,*,#10675,.T.);
#16002=ORIENTED_EDGE('',*,*,#10674,.T.);
#16003=ORIENTED_EDGE('',*,*,#10673,.T.);
#16004=ORIENTED_EDGE('',*,*,#10672,.T.);
#16005=ORIENTED_EDGE('',*,*,#10671,.T.);
#16006=ORIENTED_EDGE('',*,*,#10886,.T.);
#16007=ORIENTED_EDGE('',*,*,#10687,.T.);
#16008=ORIENTED_EDGE('',*,*,#10686,.T.);
#16009=ORIENTED_EDGE('',*,*,#10685,.T.);
#16010=ORIENTED_EDGE('',*,*,#10684,.T.);
#16011=ORIENTED_EDGE('',*,*,#10683,.T.);
#16012=ORIENTED_EDGE('',*,*,#10682,.T.);
#16013=ORIENTED_EDGE('',*,*,#10681,.T.);
#16014=ORIENTED_EDGE('',*,*,#10887,.T.);
#16015=ORIENTED_EDGE('',*,*,#10697,.T.);
#16016=ORIENTED_EDGE('',*,*,#10696,.T.);
#16017=ORIENTED_EDGE('',*,*,#10695,.T.);
#16018=ORIENTED_EDGE('',*,*,#10694,.T.);
#16019=ORIENTED_EDGE('',*,*,#10693,.T.);
#16020=ORIENTED_EDGE('',*,*,#10692,.T.);
#16021=ORIENTED_EDGE('',*,*,#10691,.T.);
#16022=ORIENTED_EDGE('',*,*,#10888,.T.);
#16023=ORIENTED_EDGE('',*,*,#10707,.T.);
#16024=ORIENTED_EDGE('',*,*,#10706,.T.);
#16025=ORIENTED_EDGE('',*,*,#10705,.T.);
#16026=ORIENTED_EDGE('',*,*,#10704,.T.);
#16027=ORIENTED_EDGE('',*,*,#10703,.T.);
#16028=ORIENTED_EDGE('',*,*,#10702,.T.);
#16029=ORIENTED_EDGE('',*,*,#10701,.T.);
#16030=ORIENTED_EDGE('',*,*,#10889,.T.);
#16031=ORIENTED_EDGE('',*,*,#10717,.T.);
#16032=ORIENTED_EDGE('',*,*,#10716,.T.);
#16033=ORIENTED_EDGE('',*,*,#10715,.T.);
#16034=ORIENTED_EDGE('',*,*,#10714,.T.);
#16035=ORIENTED_EDGE('',*,*,#10713,.T.);
#16036=ORIENTED_EDGE('',*,*,#10712,.T.);
#16037=ORIENTED_EDGE('',*,*,#10711,.T.);
#16038=ORIENTED_EDGE('',*,*,#10890,.T.);
#16039=ORIENTED_EDGE('',*,*,#10891,.T.);
#16040=ORIENTED_EDGE('',*,*,#10892,.T.);
#16041=ORIENTED_EDGE('',*,*,#10893,.T.);
#16042=ORIENTED_EDGE('',*,*,#10894,.T.);
#16043=ORIENTED_EDGE('',*,*,#10895,.T.);
#16044=ORIENTED_EDGE('',*,*,#10731,.F.);
#16045=ORIENTED_EDGE('',*,*,#10827,.T.);
#16046=ORIENTED_EDGE('',*,*,#10733,.F.);
#16047=ORIENTED_EDGE('',*,*,#10896,.T.);
#16048=ORIENTED_EDGE('',*,*,#10897,.T.);
#16049=ORIENTED_EDGE('',*,*,#10828,.T.);
#16050=ORIENTED_EDGE('',*,*,#10898,.T.);
#16051=ORIENTED_EDGE('',*,*,#10899,.T.);
#16052=ORIENTED_EDGE('',*,*,#10900,.T.);
#16053=ORIENTED_EDGE('',*,*,#10901,.T.);
#16054=ORIENTED_EDGE('',*,*,#10902,.T.);
#16055=ORIENTED_EDGE('',*,*,#10903,.T.);
#16056=ORIENTED_EDGE('',*,*,#10904,.T.);
#16057=ORIENTED_EDGE('',*,*,#10905,.T.);
#16058=ORIENTED_EDGE('',*,*,#10906,.T.);
#16059=ORIENTED_EDGE('',*,*,#10907,.T.);
#16060=ORIENTED_EDGE('',*,*,#10908,.T.);
#16061=ORIENTED_EDGE('',*,*,#10909,.T.);
#16062=ORIENTED_EDGE('',*,*,#10910,.T.);
#16063=ORIENTED_EDGE('',*,*,#10911,.F.);
#16064=ORIENTED_EDGE('',*,*,#10912,.F.);
#16065=ORIENTED_EDGE('',*,*,#10913,.T.);
#16066=ORIENTED_EDGE('',*,*,#10914,.T.);
#16067=ORIENTED_EDGE('',*,*,#10915,.F.);
#16068=ORIENTED_EDGE('',*,*,#10916,.T.);
#16069=ORIENTED_EDGE('',*,*,#10917,.T.);
#16070=ORIENTED_EDGE('',*,*,#10918,.T.);
#16071=ORIENTED_EDGE('',*,*,#10913,.F.);
#16072=ORIENTED_EDGE('',*,*,#10919,.T.);
#16073=ORIENTED_EDGE('',*,*,#10915,.T.);
#16074=ORIENTED_EDGE('',*,*,#10920,.T.);
#16075=ORIENTED_EDGE('',*,*,#10921,.T.);
#16076=ORIENTED_EDGE('',*,*,#10922,.T.);
#16077=ORIENTED_EDGE('',*,*,#10923,.F.);
#16078=ORIENTED_EDGE('',*,*,#10924,.T.);
#16079=ORIENTED_EDGE('',*,*,#10925,.T.);
#16080=ORIENTED_EDGE('',*,*,#10926,.T.);
#16081=ORIENTED_EDGE('',*,*,#10861,.F.);
#16082=ORIENTED_EDGE('',*,*,#10927,.F.);
#16083=ORIENTED_EDGE('',*,*,#10928,.T.);
#16084=ORIENTED_EDGE('',*,*,#10923,.T.);
#16085=ORIENTED_EDGE('',*,*,#10860,.F.);
#16086=ORIENTED_EDGE('',*,*,#10929,.T.);
#16087=ORIENTED_EDGE('',*,*,#10930,.T.);
#16088=ORIENTED_EDGE('',*,*,#10931,.T.);
#16089=ORIENTED_EDGE('',*,*,#10927,.T.);
#16090=ORIENTED_EDGE('',*,*,#10859,.F.);
#16091=ORIENTED_EDGE('',*,*,#10932,.T.);
#16092=ORIENTED_EDGE('',*,*,#10933,.T.);
#16093=ORIENTED_EDGE('',*,*,#10934,.T.);
#16094=ORIENTED_EDGE('',*,*,#10935,.T.);
#16095=ORIENTED_EDGE('',*,*,#10936,.F.);
#16096=ORIENTED_EDGE('',*,*,#10866,.F.);
#16097=ORIENTED_EDGE('',*,*,#10936,.T.);
#16098=ORIENTED_EDGE('',*,*,#10937,.T.);
#16099=ORIENTED_EDGE('',*,*,#10938,.F.);
#16100=ORIENTED_EDGE('',*,*,#10867,.F.);
#16101=ORIENTED_EDGE('',*,*,#10938,.T.);
#16102=ORIENTED_EDGE('',*,*,#10939,.T.);
#16103=ORIENTED_EDGE('',*,*,#10940,.T.);
#16104=ORIENTED_EDGE('',*,*,#10941,.T.);
#16105=ORIENTED_EDGE('',*,*,#10942,.T.);
#16106=ORIENTED_EDGE('',*,*,#10863,.F.);
#16107=ORIENTED_EDGE('',*,*,#10943,.T.);
#16108=ORIENTED_EDGE('',*,*,#10944,.T.);
#16109=ORIENTED_EDGE('',*,*,#10945,.T.);
#16110=ORIENTED_EDGE('',*,*,#10881,.F.);
#16111=ORIENTED_EDGE('',*,*,#10946,.F.);
#16112=ORIENTED_EDGE('',*,*,#10942,.F.);
#16113=ORIENTED_EDGE('',*,*,#10883,.F.);
#16114=ORIENTED_EDGE('',*,*,#10864,.F.);
#16115=ORIENTED_EDGE('',*,*,#10946,.T.);
#16116=ORIENTED_EDGE('',*,*,#10947,.T.);
#16117=ORIENTED_EDGE('',*,*,#10948,.T.);
#16118=ORIENTED_EDGE('',*,*,#10949,.T.);
#16119=ORIENTED_EDGE('',*,*,#10929,.F.);
#16120=ORIENTED_EDGE('',*,*,#10950,.F.);
#16121=ORIENTED_EDGE('',*,*,#10871,.F.);
#16122=ORIENTED_EDGE('',*,*,#10870,.F.);
#16123=ORIENTED_EDGE('',*,*,#10858,.F.);
#16124=ORIENTED_EDGE('',*,*,#10872,.F.);
#16125=ORIENTED_EDGE('',*,*,#10950,.T.);
#16126=ORIENTED_EDGE('',*,*,#10951,.T.);
#16127=ORIENTED_EDGE('',*,*,#10952,.T.);
#16128=ORIENTED_EDGE('',*,*,#10953,.T.);
#16129=ORIENTED_EDGE('',*,*,#10880,.F.);
#16130=ORIENTED_EDGE('',*,*,#10879,.F.);
#16131=ORIENTED_EDGE('',*,*,#10954,.F.);
#16132=ORIENTED_EDGE('',*,*,#10926,.F.);
#16133=ORIENTED_EDGE('',*,*,#10878,.F.);
#16134=ORIENTED_EDGE('',*,*,#10862,.F.);
#16135=ORIENTED_EDGE('',*,*,#10954,.T.);
#16136=ORIENTED_EDGE('',*,*,#10865,.F.);
#16137=ORIENTED_EDGE('',*,*,#10877,.F.);
#16138=ORIENTED_EDGE('',*,*,#10955,.F.);
#16139=ORIENTED_EDGE('',*,*,#10956,.T.);
#16140=ORIENTED_EDGE('',*,*,#10957,.T.);
#16141=ORIENTED_EDGE('',*,*,#10958,.T.);
#16142=ORIENTED_EDGE('',*,*,#10932,.F.);
#16143=ORIENTED_EDGE('',*,*,#10955,.T.);
#16144=ORIENTED_EDGE('',*,*,#10876,.F.);
#16145=ORIENTED_EDGE('',*,*,#10823,.F.);
#16146=ORIENTED_EDGE('',*,*,#10959,.T.);
#16147=ORIENTED_EDGE('',*,*,#10754,.F.);
#16148=ORIENTED_EDGE('',*,*,#10960,.F.);
#16149=ORIENTED_EDGE('',*,*,#10824,.T.);
#16150=ORIENTED_EDGE('',*,*,#10960,.T.);
#16151=ORIENTED_EDGE('',*,*,#10961,.F.);
#16152=ORIENTED_EDGE('',*,*,#10962,.F.);
#16153=ORIENTED_EDGE('',*,*,#10757,.F.);
#16154=ORIENTED_EDGE('',*,*,#10963,.T.);
#16155=ORIENTED_EDGE('',*,*,#10891,.F.);
#16156=ORIENTED_EDGE('',*,*,#10961,.T.);
#16157=ORIENTED_EDGE('',*,*,#10962,.T.);
#16158=ORIENTED_EDGE('',*,*,#10890,.F.);
#16159=ORIENTED_EDGE('',*,*,#10964,.F.);
#16160=ORIENTED_EDGE('',*,*,#10825,.F.);
#16161=ORIENTED_EDGE('',*,*,#10892,.F.);
#16162=ORIENTED_EDGE('',*,*,#10965,.T.);
#16163=ORIENTED_EDGE('',*,*,#10744,.F.);
#16164=ORIENTED_EDGE('',*,*,#10966,.F.);
#16165=ORIENTED_EDGE('',*,*,#10964,.T.);
#16166=ORIENTED_EDGE('',*,*,#10893,.F.);
#16167=ORIENTED_EDGE('',*,*,#10967,.F.);
#16168=ORIENTED_EDGE('',*,*,#10894,.F.);
#16169=ORIENTED_EDGE('',*,*,#10826,.F.);
#16170=ORIENTED_EDGE('',*,*,#10966,.T.);
#16171=ORIENTED_EDGE('',*,*,#10743,.T.);
#16172=ORIENTED_EDGE('',*,*,#10968,.F.);
#16173=ORIENTED_EDGE('',*,*,#10967,.T.);
#16174=ORIENTED_EDGE('',*,*,#10968,.T.);
#16175=ORIENTED_EDGE('',*,*,#10742,.F.);
#16176=ORIENTED_EDGE('',*,*,#10969,.F.);
#16177=ORIENTED_EDGE('',*,*,#10895,.F.);
#16178=ORIENTED_EDGE('',*,*,#10969,.T.);
#16179=ORIENTED_EDGE('',*,*,#10741,.F.);
#16180=ORIENTED_EDGE('',*,*,#10970,.F.);
#16181=ORIENTED_EDGE('',*,*,#10732,.F.);
#16182=ORIENTED_EDGE('',*,*,#10970,.T.);
#16183=ORIENTED_EDGE('',*,*,#10740,.F.);
#16184=ORIENTED_EDGE('',*,*,#10971,.F.);
#16185=ORIENTED_EDGE('',*,*,#10896,.F.);
#16186=ORIENTED_EDGE('',*,*,#10971,.T.);
#16187=ORIENTED_EDGE('',*,*,#10739,.T.);
#16188=ORIENTED_EDGE('',*,*,#10972,.F.);
#16189=ORIENTED_EDGE('',*,*,#10973,.F.);
#16190=ORIENTED_EDGE('',*,*,#10738,.F.);
#16191=ORIENTED_EDGE('',*,*,#10753,.F.);
#16192=ORIENTED_EDGE('',*,*,#10974,.F.);
#16193=ORIENTED_EDGE('',*,*,#10727,.F.);
#16194=ORIENTED_EDGE('',*,*,#10972,.T.);
#16195=ORIENTED_EDGE('',*,*,#10973,.T.);
#16196=ORIENTED_EDGE('',*,*,#10730,.F.);
#16197=ORIENTED_EDGE('',*,*,#10975,.F.);
#16198=ORIENTED_EDGE('',*,*,#10829,.F.);
#16199=ORIENTED_EDGE('',*,*,#10897,.F.);
#16200=ORIENTED_EDGE('',*,*,#10974,.T.);
#16201=ORIENTED_EDGE('',*,*,#10752,.F.);
#16202=ORIENTED_EDGE('',*,*,#10976,.F.);
#16203=ORIENTED_EDGE('',*,*,#10728,.F.);
#16204=ORIENTED_EDGE('',*,*,#10975,.T.);
#16205=ORIENTED_EDGE('',*,*,#10729,.F.);
#16206=ORIENTED_EDGE('',*,*,#10977,.F.);
#16207=ORIENTED_EDGE('',*,*,#10830,.F.);
#16208=ORIENTED_EDGE('',*,*,#10977,.T.);
#16209=ORIENTED_EDGE('',*,*,#10976,.T.);
#16210=ORIENTED_EDGE('',*,*,#10978,.F.);
#16211=ORIENTED_EDGE('',*,*,#10831,.T.);
#16212=ORIENTED_EDGE('',*,*,#10751,.F.);
#16213=ORIENTED_EDGE('',*,*,#10979,.T.);
#16214=ORIENTED_EDGE('',*,*,#10821,.F.);
#16215=ORIENTED_EDGE('',*,*,#10978,.T.);
#16216=ORIENTED_EDGE('',*,*,#10958,.F.);
#16217=ORIENTED_EDGE('',*,*,#10980,.T.);
#16218=ORIENTED_EDGE('',*,*,#10903,.F.);
#16219=ORIENTED_EDGE('',*,*,#10981,.F.);
#16220=ORIENTED_EDGE('',*,*,#10982,.F.);
#16221=ORIENTED_EDGE('',*,*,#10782,.F.);
#16222=ORIENTED_EDGE('',*,*,#10983,.F.);
#16223=ORIENTED_EDGE('',*,*,#10792,.F.);
#16224=ORIENTED_EDGE('',*,*,#10904,.F.);
#16225=ORIENTED_EDGE('',*,*,#10984,.T.);
#16226=ORIENTED_EDGE('',*,*,#10985,.T.);
#16227=ORIENTED_EDGE('',*,*,#10839,.F.);
#16228=ORIENTED_EDGE('',*,*,#10986,.F.);
#16229=ORIENTED_EDGE('',*,*,#10981,.T.);
#16230=ORIENTED_EDGE('',*,*,#10902,.F.);
#16231=ORIENTED_EDGE('',*,*,#10901,.F.);
#16232=ORIENTED_EDGE('',*,*,#10987,.F.);
#16233=ORIENTED_EDGE('',*,*,#10935,.F.);
#16234=ORIENTED_EDGE('',*,*,#10934,.F.);
#16235=ORIENTED_EDGE('',*,*,#10933,.F.);
#16236=ORIENTED_EDGE('',*,*,#10983,.T.);
#16237=ORIENTED_EDGE('',*,*,#10785,.F.);
#16238=ORIENTED_EDGE('',*,*,#10988,.F.);
#16239=ORIENTED_EDGE('',*,*,#10793,.F.);
#16240=ORIENTED_EDGE('',*,*,#10982,.T.);
#16241=ORIENTED_EDGE('',*,*,#10791,.F.);
#16242=ORIENTED_EDGE('',*,*,#10989,.F.);
#16243=ORIENTED_EDGE('',*,*,#10845,.F.);
#16244=ORIENTED_EDGE('',*,*,#10990,.F.);
#16245=ORIENTED_EDGE('',*,*,#10846,.F.);
#16246=ORIENTED_EDGE('',*,*,#10991,.F.);
#16247=ORIENTED_EDGE('',*,*,#10917,.F.);
#16248=ORIENTED_EDGE('',*,*,#10847,.T.);
#16249=ORIENTED_EDGE('',*,*,#10990,.T.);
#16250=ORIENTED_EDGE('',*,*,#10992,.F.);
#16251=ORIENTED_EDGE('',*,*,#10986,.T.);
#16252=ORIENTED_EDGE('',*,*,#10987,.T.);
#16253=ORIENTED_EDGE('',*,*,#10900,.F.);
#16254=ORIENTED_EDGE('',*,*,#10993,.F.);
#16255=ORIENTED_EDGE('',*,*,#10937,.F.);
#16256=ORIENTED_EDGE('',*,*,#10988,.T.);
#16257=ORIENTED_EDGE('',*,*,#10787,.F.);
#16258=ORIENTED_EDGE('',*,*,#10994,.F.);
#16259=ORIENTED_EDGE('',*,*,#10794,.F.);
#16260=ORIENTED_EDGE('',*,*,#10991,.T.);
#16261=ORIENTED_EDGE('',*,*,#10989,.T.);
#16262=ORIENTED_EDGE('',*,*,#10995,.F.);
#16263=ORIENTED_EDGE('',*,*,#10992,.T.);
#16264=ORIENTED_EDGE('',*,*,#10919,.F.);
#16265=ORIENTED_EDGE('',*,*,#10996,.F.);
#16266=ORIENTED_EDGE('',*,*,#10905,.F.);
#16267=ORIENTED_EDGE('',*,*,#10993,.T.);
#16268=ORIENTED_EDGE('',*,*,#10899,.F.);
#16269=ORIENTED_EDGE('',*,*,#10898,.F.);
#16270=ORIENTED_EDGE('',*,*,#10997,.F.);
#16271=ORIENTED_EDGE('',*,*,#10941,.F.);
#16272=ORIENTED_EDGE('',*,*,#10940,.F.);
#16273=ORIENTED_EDGE('',*,*,#10939,.F.);
#16274=ORIENTED_EDGE('',*,*,#10994,.T.);
#16275=ORIENTED_EDGE('',*,*,#10778,.F.);
#16276=ORIENTED_EDGE('',*,*,#10998,.F.);
#16277=ORIENTED_EDGE('',*,*,#10795,.F.);
#16278=ORIENTED_EDGE('',*,*,#10995,.T.);
#16279=ORIENTED_EDGE('',*,*,#10790,.F.);
#16280=ORIENTED_EDGE('',*,*,#10999,.F.);
#16281=ORIENTED_EDGE('',*,*,#10918,.F.);
#16282=ORIENTED_EDGE('',*,*,#10996,.T.);
#16283=ORIENTED_EDGE('',*,*,#10916,.F.);
#16284=ORIENTED_EDGE('',*,*,#11000,.F.);
#16285=ORIENTED_EDGE('',*,*,#10906,.F.);
#16286=ORIENTED_EDGE('',*,*,#10909,.F.);
#16287=ORIENTED_EDGE('',*,*,#11001,.T.);
#16288=ORIENTED_EDGE('',*,*,#10943,.F.);
#16289=ORIENTED_EDGE('',*,*,#10997,.T.);
#16290=ORIENTED_EDGE('',*,*,#10998,.T.);
#16291=ORIENTED_EDGE('',*,*,#10775,.F.);
#16292=ORIENTED_EDGE('',*,*,#11002,.F.);
#16293=ORIENTED_EDGE('',*,*,#10796,.F.);
#16294=ORIENTED_EDGE('',*,*,#10999,.T.);
#16295=ORIENTED_EDGE('',*,*,#10789,.F.);
#16296=ORIENTED_EDGE('',*,*,#11003,.F.);
#16297=ORIENTED_EDGE('',*,*,#10914,.F.);
#16298=ORIENTED_EDGE('',*,*,#11000,.T.);
#16299=ORIENTED_EDGE('',*,*,#10922,.F.);
#16300=ORIENTED_EDGE('',*,*,#11004,.F.);
#16301=ORIENTED_EDGE('',*,*,#10907,.F.);
#16302=ORIENTED_EDGE('',*,*,#11005,.T.);
#16303=ORIENTED_EDGE('',*,*,#11006,.T.);
#16304=ORIENTED_EDGE('',*,*,#10908,.F.);
#16305=ORIENTED_EDGE('',*,*,#11007,.F.);
#16306=ORIENTED_EDGE('',*,*,#10854,.F.);
#16307=ORIENTED_EDGE('',*,*,#11002,.T.);
#16308=ORIENTED_EDGE('',*,*,#10857,.F.);
#16309=ORIENTED_EDGE('',*,*,#11008,.F.);
#16310=ORIENTED_EDGE('',*,*,#10797,.F.);
#16311=ORIENTED_EDGE('',*,*,#11003,.T.);
#16312=ORIENTED_EDGE('',*,*,#10788,.F.);
#16313=ORIENTED_EDGE('',*,*,#11009,.F.);
#16314=ORIENTED_EDGE('',*,*,#10920,.F.);
#16315=ORIENTED_EDGE('',*,*,#11007,.T.);
#16316=ORIENTED_EDGE('',*,*,#11004,.T.);
#16317=ORIENTED_EDGE('',*,*,#11010,.F.);
#16318=ORIENTED_EDGE('',*,*,#10855,.T.);
#16319=ORIENTED_EDGE('',*,*,#11009,.T.);
#16320=ORIENTED_EDGE('',*,*,#11008,.T.);
#16321=ORIENTED_EDGE('',*,*,#11011,.F.);
#16322=ORIENTED_EDGE('',*,*,#11010,.T.);
#16323=ORIENTED_EDGE('',*,*,#10921,.F.);
#16324=ORIENTED_EDGE('',*,*,#11011,.T.);
#16325=ORIENTED_EDGE('',*,*,#10856,.F.);
#16326=ORIENTED_EDGE('',*,*,#11012,.F.);
#16327=ORIENTED_EDGE('',*,*,#10723,.F.);
#16328=ORIENTED_EDGE('',*,*,#11013,.T.);
#16329=ORIENTED_EDGE('',*,*,#10832,.F.);
#16330=ORIENTED_EDGE('',*,*,#11013,.F.);
#16331=ORIENTED_EDGE('',*,*,#10722,.F.);
#16332=ORIENTED_EDGE('',*,*,#10833,.F.);
#16333=ORIENTED_EDGE('',*,*,#11014,.T.);
#16334=ORIENTED_EDGE('',*,*,#10837,.F.);
#16335=ORIENTED_EDGE('',*,*,#10838,.F.);
#16336=ORIENTED_EDGE('',*,*,#11014,.F.);
#16337=ORIENTED_EDGE('',*,*,#10810,.F.);
#16338=ORIENTED_EDGE('',*,*,#11015,.T.);
#16339=ORIENTED_EDGE('',*,*,#10951,.F.);
#16340=ORIENTED_EDGE('',*,*,#11016,.F.);
#16341=ORIENTED_EDGE('',*,*,#11017,.T.);
#16342=ORIENTED_EDGE('',*,*,#11018,.T.);
#16343=ORIENTED_EDGE('',*,*,#10809,.F.);
#16344=ORIENTED_EDGE('',*,*,#11019,.F.);
#16345=ORIENTED_EDGE('',*,*,#10844,.F.);
#16346=ORIENTED_EDGE('',*,*,#11016,.T.);
#16347=ORIENTED_EDGE('',*,*,#10925,.F.);
#16348=ORIENTED_EDGE('',*,*,#10924,.F.);
#16349=ORIENTED_EDGE('',*,*,#11020,.F.);
#16350=ORIENTED_EDGE('',*,*,#10811,.F.);
#16351=ORIENTED_EDGE('',*,*,#11019,.T.);
#16352=ORIENTED_EDGE('',*,*,#10808,.F.);
#16353=ORIENTED_EDGE('',*,*,#11021,.F.);
#16354=ORIENTED_EDGE('',*,*,#10780,.F.);
#16355=ORIENTED_EDGE('',*,*,#11020,.T.);
#16356=ORIENTED_EDGE('',*,*,#10928,.F.);
#16357=ORIENTED_EDGE('',*,*,#11022,.F.);
#16358=ORIENTED_EDGE('',*,*,#10812,.F.);
#16359=ORIENTED_EDGE('',*,*,#11021,.T.);
#16360=ORIENTED_EDGE('',*,*,#10807,.F.);
#16361=ORIENTED_EDGE('',*,*,#11023,.F.);
#16362=ORIENTED_EDGE('',*,*,#10783,.F.);
#16363=ORIENTED_EDGE('',*,*,#11022,.T.);
#16364=ORIENTED_EDGE('',*,*,#10931,.F.);
#16365=ORIENTED_EDGE('',*,*,#10930,.F.);
#16366=ORIENTED_EDGE('',*,*,#11024,.F.);
#16367=ORIENTED_EDGE('',*,*,#10801,.F.);
#16368=ORIENTED_EDGE('',*,*,#11023,.T.);
#16369=ORIENTED_EDGE('',*,*,#10806,.F.);
#16370=ORIENTED_EDGE('',*,*,#11025,.F.);
#16371=ORIENTED_EDGE('',*,*,#10786,.F.);
#16372=ORIENTED_EDGE('',*,*,#10949,.F.);
#16373=ORIENTED_EDGE('',*,*,#11026,.T.);
#16374=ORIENTED_EDGE('',*,*,#10802,.F.);
#16375=ORIENTED_EDGE('',*,*,#11024,.T.);
#16376=ORIENTED_EDGE('',*,*,#11025,.T.);
#16377=ORIENTED_EDGE('',*,*,#10805,.F.);
#16378=ORIENTED_EDGE('',*,*,#11027,.F.);
#16379=ORIENTED_EDGE('',*,*,#10777,.F.);
#16380=ORIENTED_EDGE('',*,*,#10803,.F.);
#16381=ORIENTED_EDGE('',*,*,#11028,.T.);
#16382=ORIENTED_EDGE('',*,*,#11029,.T.);
#16383=ORIENTED_EDGE('',*,*,#10848,.F.);
#16384=ORIENTED_EDGE('',*,*,#11030,.F.);
#16385=ORIENTED_EDGE('',*,*,#11027,.T.);
#16386=ORIENTED_EDGE('',*,*,#10804,.F.);
#16387=ORIENTED_EDGE('',*,*,#11030,.T.);
#16388=ORIENTED_EDGE('',*,*,#10773,.F.);
#16389=ORIENTED_EDGE('',*,*,#11031,.F.);
#16390=ORIENTED_EDGE('',*,*,#10816,.F.);
#16391=ORIENTED_EDGE('',*,*,#11032,.F.);
#16392=ORIENTED_EDGE('',*,*,#10813,.F.);
#16393=ORIENTED_EDGE('',*,*,#11032,.T.);
#16394=ORIENTED_EDGE('',*,*,#10819,.F.);
#16395=ORIENTED_EDGE('',*,*,#11031,.T.);
#16396=ORIENTED_EDGE('',*,*,#10814,.F.);
#16397=ORIENTED_EDGE('',*,*,#10834,.F.);
#16398=ORIENTED_EDGE('',*,*,#10835,.F.);
#16399=ORIENTED_EDGE('',*,*,#11033,.T.);
#16400=ORIENTED_EDGE('',*,*,#10800,.F.);
#16401=ORIENTED_EDGE('',*,*,#11033,.F.);
#16402=ORIENTED_EDGE('',*,*,#10726,.F.);
#16403=ORIENTED_EDGE('',*,*,#11034,.T.);
#16404=ORIENTED_EDGE('',*,*,#10910,.F.);
#16405=ORIENTED_EDGE('',*,*,#11034,.F.);
#16406=ORIENTED_EDGE('',*,*,#10965,.F.);
#16407=ORIENTED_EDGE('',*,*,#10963,.F.);
#16408=ORIENTED_EDGE('',*,*,#11035,.F.);
#16409=ORIENTED_EDGE('',*,*,#11036,.F.);
#16410=ORIENTED_EDGE('',*,*,#10822,.F.);
#16411=ORIENTED_EDGE('',*,*,#11037,.F.);
#16412=ORIENTED_EDGE('',*,*,#10720,.F.);
#16413=ORIENTED_EDGE('',*,*,#10959,.F.);
#16414=ORIENTED_EDGE('',*,*,#11036,.T.);
#16415=ORIENTED_EDGE('',*,*,#11038,.F.);
#16416=ORIENTED_EDGE('',*,*,#11037,.T.);
#16417=ORIENTED_EDGE('',*,*,#10979,.F.);
#16418=ORIENTED_EDGE('',*,*,#11039,.F.);
#16419=ORIENTED_EDGE('',*,*,#11038,.T.);
#16420=ORIENTED_EDGE('',*,*,#10719,.F.);
#16421=ORIENTED_EDGE('',*,*,#11040,.F.);
#16422=ORIENTED_EDGE('',*,*,#10755,.F.);
#16423=ORIENTED_EDGE('',*,*,#11035,.T.);
#16424=ORIENTED_EDGE('',*,*,#10756,.F.);
#16425=ORIENTED_EDGE('',*,*,#11041,.F.);
#16426=ORIENTED_EDGE('',*,*,#10735,.F.);
#16427=ORIENTED_EDGE('',*,*,#10750,.F.);
#16428=ORIENTED_EDGE('',*,*,#11042,.F.);
#16429=ORIENTED_EDGE('',*,*,#10721,.F.);
#16430=ORIENTED_EDGE('',*,*,#11039,.T.);
#16431=ORIENTED_EDGE('',*,*,#11040,.T.);
#16432=ORIENTED_EDGE('',*,*,#10718,.T.);
#16433=ORIENTED_EDGE('',*,*,#11043,.F.);
#16434=ORIENTED_EDGE('',*,*,#11041,.T.);
#16435=ORIENTED_EDGE('',*,*,#10749,.F.);
#16436=ORIENTED_EDGE('',*,*,#10736,.F.);
#16437=ORIENTED_EDGE('',*,*,#11043,.T.);
#16438=ORIENTED_EDGE('',*,*,#11012,.T.);
#16439=ORIENTED_EDGE('',*,*,#11042,.T.);
#16440=ORIENTED_EDGE('',*,*,#10708,.T.);
#16441=ORIENTED_EDGE('',*,*,#10889,.F.);
#16442=ORIENTED_EDGE('',*,*,#10710,.F.);
#16443=ORIENTED_EDGE('',*,*,#10767,.F.);
#16444=ORIENTED_EDGE('',*,*,#10698,.T.);
#16445=ORIENTED_EDGE('',*,*,#10888,.F.);
#16446=ORIENTED_EDGE('',*,*,#10700,.F.);
#16447=ORIENTED_EDGE('',*,*,#10768,.F.);
#16448=ORIENTED_EDGE('',*,*,#10688,.T.);
#16449=ORIENTED_EDGE('',*,*,#10887,.F.);
#16450=ORIENTED_EDGE('',*,*,#10690,.F.);
#16451=ORIENTED_EDGE('',*,*,#10769,.F.);
#16452=ORIENTED_EDGE('',*,*,#10678,.T.);
#16453=ORIENTED_EDGE('',*,*,#10886,.F.);
#16454=ORIENTED_EDGE('',*,*,#10680,.F.);
#16455=ORIENTED_EDGE('',*,*,#10770,.F.);
#16456=ORIENTED_EDGE('',*,*,#10668,.T.);
#16457=ORIENTED_EDGE('',*,*,#10885,.F.);
#16458=ORIENTED_EDGE('',*,*,#10670,.F.);
#16459=ORIENTED_EDGE('',*,*,#10771,.F.);
#16460=ORIENTED_EDGE('',*,*,#11015,.F.);
#16461=ORIENTED_EDGE('',*,*,#11018,.F.);
#16462=ORIENTED_EDGE('',*,*,#11044,.F.);
#16463=ORIENTED_EDGE('',*,*,#11044,.T.);
#16464=ORIENTED_EDGE('',*,*,#11017,.F.);
#16465=ORIENTED_EDGE('',*,*,#11045,.F.);
#16466=ORIENTED_EDGE('',*,*,#10952,.F.);
#16467=ORIENTED_EDGE('',*,*,#11045,.T.);
#16468=ORIENTED_EDGE('',*,*,#10843,.F.);
#16469=ORIENTED_EDGE('',*,*,#11046,.F.);
#16470=ORIENTED_EDGE('',*,*,#10953,.F.);
#16471=ORIENTED_EDGE('',*,*,#11046,.T.);
#16472=ORIENTED_EDGE('',*,*,#10842,.F.);
#16473=ORIENTED_EDGE('',*,*,#11047,.F.);
#16474=ORIENTED_EDGE('',*,*,#10874,.F.);
#16475=ORIENTED_EDGE('',*,*,#11047,.T.);
#16476=ORIENTED_EDGE('',*,*,#10841,.F.);
#16477=ORIENTED_EDGE('',*,*,#11048,.F.);
#16478=ORIENTED_EDGE('',*,*,#10875,.F.);
#16479=ORIENTED_EDGE('',*,*,#11048,.T.);
#16480=ORIENTED_EDGE('',*,*,#10840,.F.);
#16481=ORIENTED_EDGE('',*,*,#11049,.F.);
#16482=ORIENTED_EDGE('',*,*,#10956,.F.);
#16483=ORIENTED_EDGE('',*,*,#11049,.T.);
#16484=ORIENTED_EDGE('',*,*,#10985,.F.);
#16485=ORIENTED_EDGE('',*,*,#11050,.F.);
#16486=ORIENTED_EDGE('',*,*,#10957,.F.);
#16487=ORIENTED_EDGE('',*,*,#10984,.F.);
#16488=ORIENTED_EDGE('',*,*,#10980,.F.);
#16489=ORIENTED_EDGE('',*,*,#11050,.T.);
#16490=ORIENTED_EDGE('',*,*,#11001,.F.);
#16491=ORIENTED_EDGE('',*,*,#11006,.F.);
#16492=ORIENTED_EDGE('',*,*,#11051,.F.);
#16493=ORIENTED_EDGE('',*,*,#11051,.T.);
#16494=ORIENTED_EDGE('',*,*,#11005,.F.);
#16495=ORIENTED_EDGE('',*,*,#11052,.F.);
#16496=ORIENTED_EDGE('',*,*,#10944,.F.);
#16497=ORIENTED_EDGE('',*,*,#11052,.T.);
#16498=ORIENTED_EDGE('',*,*,#10853,.F.);
#16499=ORIENTED_EDGE('',*,*,#11053,.F.);
#16500=ORIENTED_EDGE('',*,*,#10945,.F.);
#16501=ORIENTED_EDGE('',*,*,#11053,.T.);
#16502=ORIENTED_EDGE('',*,*,#10852,.F.);
#16503=ORIENTED_EDGE('',*,*,#11054,.F.);
#16504=ORIENTED_EDGE('',*,*,#10882,.F.);
#16505=ORIENTED_EDGE('',*,*,#11054,.T.);
#16506=ORIENTED_EDGE('',*,*,#10851,.F.);
#16507=ORIENTED_EDGE('',*,*,#11055,.F.);
#16508=ORIENTED_EDGE('',*,*,#10868,.F.);
#16509=ORIENTED_EDGE('',*,*,#11055,.T.);
#16510=ORIENTED_EDGE('',*,*,#10850,.F.);
#16511=ORIENTED_EDGE('',*,*,#11056,.F.);
#16512=ORIENTED_EDGE('',*,*,#10869,.F.);
#16513=ORIENTED_EDGE('',*,*,#11056,.T.);
#16514=ORIENTED_EDGE('',*,*,#10849,.F.);
#16515=ORIENTED_EDGE('',*,*,#11057,.F.);
#16516=ORIENTED_EDGE('',*,*,#10947,.F.);
#16517=ORIENTED_EDGE('',*,*,#11057,.T.);
#16518=ORIENTED_EDGE('',*,*,#11029,.F.);
#16519=ORIENTED_EDGE('',*,*,#11058,.F.);
#16520=ORIENTED_EDGE('',*,*,#10948,.F.);
#16521=ORIENTED_EDGE('',*,*,#11028,.F.);
#16522=ORIENTED_EDGE('',*,*,#11026,.F.);
#16523=ORIENTED_EDGE('',*,*,#11058,.T.);
#16524=ORIENTED_EDGE('',*,*,#10912,.T.);
#16525=ORIENTED_EDGE('',*,*,#11059,.T.);
#16526=ORIENTED_EDGE('',*,*,#10748,.F.);
#16527=ORIENTED_EDGE('',*,*,#11059,.F.);
#16528=ORIENTED_EDGE('',*,*,#10911,.T.);
#16529=ORIENTED_EDGE('',*,*,#11060,.T.);
#16530=ORIENTED_EDGE('',*,*,#10747,.F.);
#16531=ORIENTED_EDGE('',*,*,#11060,.F.);
#16532=ORIENTED_EDGE('',*,*,#10799,.T.);
#16533=ORIENTED_EDGE('',*,*,#11061,.T.);
#16534=ORIENTED_EDGE('',*,*,#10746,.F.);
#16535=ORIENTED_EDGE('',*,*,#11061,.F.);
#16536=ORIENTED_EDGE('',*,*,#10798,.T.);
#16537=ORIENTED_EDGE('',*,*,#11062,.T.);
#16538=ORIENTED_EDGE('',*,*,#10745,.F.);
#16539=ORIENTED_EDGE('',*,*,#11062,.F.);
#16540=ORIENTED_EDGE('',*,*,#10884,.F.);
#16541=ORIENTED_EDGE('',*,*,#11063,.T.);
#16542=ORIENTED_EDGE('',*,*,#10764,.F.);
#16543=ORIENTED_EDGE('',*,*,#10765,.F.);
#16544=ORIENTED_EDGE('',*,*,#11063,.F.);
#16545=ORIENTED_EDGE('',*,*,#11064,.T.);
#16546=ORIENTED_EDGE('',*,*,#11065,.F.);
#16547=ORIENTED_EDGE('',*,*,#11065,.T.);
#16548=ORIENTED_EDGE('',*,*,#11066,.F.);
#16549=ORIENTED_EDGE('',*,*,#11067,.F.);
#16550=ORIENTED_EDGE('',*,*,#11068,.T.);
#16551=ORIENTED_EDGE('',*,*,#11066,.T.);
#16552=ORIENTED_EDGE('',*,*,#11068,.F.);
#16553=ORIENTED_EDGE('',*,*,#11064,.F.);
#16554=ORIENTED_EDGE('',*,*,#11067,.T.);
#16555=PLANE('',#17837);
#16556=PLANE('',#18113);
#16557=PLANE('',#18413);
#16558=PLANE('',#18416);
#16559=PLANE('',#18470);
#16560=PLANE('',#18472);
#16561=PLANE('',#18474);
#16562=PLANE('',#18531);
#16563=PLANE('',#18533);
#16564=PLANE('',#18535);
#16565=PLANE('',#18536);
#16566=PLANE('',#18548);
#16567=PLANE('',#18551);
#16568=PLANE('',#18750);
#16569=PLANE('',#18762);
#16570=PLANE('',#18764);
#16571=PLANE('',#18785);
#16572=PLANE('',#18793);
#16573=PLANE('',#18800);
#16574=PLANE('',#18801);
#16575=PLANE('',#18813);
#16576=PLANE('',#18818);
#16577=PLANE('',#18823);
#16578=PLANE('',#18824);
#16579=PLANE('',#18825);
#16580=PLANE('',#18826);
#16581=PLANE('',#18827);
#16582=PLANE('',#18828);
#16583=PLANE('',#18829);
#16584=PLANE('',#18830);
#16585=PLANE('',#18831);
#16586=PLANE('',#18835);
#16587=PLANE('',#18836);
#16588=PLANE('',#18837);
#16589=PLANE('',#18838);
#16590=PLANE('',#18839);
#16591=PLANE('',#18926);
#16592=PLANE('',#18927);
#16593=PLANE('',#18928);
#16594=PLANE('',#18929);
#16595=PLANE('',#18930);
#16596=PLANE('',#18931);
#16597=PLANE('',#18932);
#16598=PLANE('',#18933);
#16599=PLANE('',#18934);
#16600=PLANE('',#18935);
#16601=PLANE('',#18936);
#16602=PLANE('',#18937);
#16603=PLANE('',#18938);
#16604=PLANE('',#18939);
#16605=PLANE('',#18940);
#16606=PLANE('',#18946);
#16607=PLANE('',#19052);
#16608=PLANE('',#19056);
#16609=PLANE('',#19060);
#16610=PLANE('',#19061);
#16611=PLANE('',#19062);
#16612=PLANE('',#19064);
#16613=PLANE('',#19071);
#16614=PLANE('',#19105);
#16615=PLANE('',#19109);
#16616=PLANE('',#19115);
#16617=PLANE('',#19116);
#16618=PLANE('',#19117);
#16619=PLANE('',#19118);
#16620=PLANE('',#19119);
#16621=PLANE('',#19120);
#16622=PLANE('',#19121);
#16623=PLANE('',#19122);
#16624=PLANE('',#19123);
#16625=PLANE('',#19124);
#16626=PLANE('',#19125);
#16627=PLANE('',#19126);
#16628=PLANE('',#19127);
#16629=PLANE('',#19128);
#16630=PLANE('',#19129);
#16631=PLANE('',#19130);
#16632=PLANE('',#19131);
#16633=PLANE('',#19132);
#16634=PLANE('',#19133);
#16635=PLANE('',#19134);
#16636=PLANE('',#19135);
#16637=PLANE('',#19145);
#16638=PLANE('',#19152);
#16639=PLANE('',#19203);
#16640=PLANE('',#19204);
#16641=PLANE('',#19208);
#16642=PLANE('',#19209);
#16643=PLANE('',#19216);
#16644=PLANE('',#19222);
#16645=PLANE('',#19307);
#16646=PLANE('',#19337);
#16647=PLANE('',#19341);
#16648=PLANE('',#19345);
#16649=PLANE('',#19353);
#16650=PLANE('',#19365);
#16651=PLANE('',#19377);
#16652=PLANE('',#19385);
#16653=PLANE('',#19387);
#16654=PLANE('',#19389);
#16655=PLANE('',#19403);
#16656=PLANE('',#19411);
#16657=PLANE('',#19412);
#16658=PLANE('',#19581);
#16659=PLANE('',#19585);
#16660=ADVANCED_FACE('',(#3544,#3477),#16555,.F.);
#16661=ADVANCED_FACE('',(#3545),#3001,.T.);
#16662=ADVANCED_FACE('',(#3546),#3002,.T.);
#16663=ADVANCED_FACE('',(#3547),#3003,.T.);
#16664=ADVANCED_FACE('',(#3548),#3004,.T.);
#16665=ADVANCED_FACE('',(#3549),#3005,.T.);
#16666=ADVANCED_FACE('',(#3550),#3006,.T.);
#16667=ADVANCED_FACE('',(#3551),#3007,.T.);
#16668=ADVANCED_FACE('',(#3552),#3008,.T.);
#16669=ADVANCED_FACE('',(#3553),#3009,.T.);
#16670=ADVANCED_FACE('',(#3554),#3010,.T.);
#16671=ADVANCED_FACE('',(#3555),#3011,.T.);
#16672=ADVANCED_FACE('',(#3556),#3012,.T.);
#16673=ADVANCED_FACE('',(#3557),#3013,.T.);
#16674=ADVANCED_FACE('',(#3558),#3014,.T.);
#16675=ADVANCED_FACE('',(#3559),#3015,.T.);
#16676=ADVANCED_FACE('',(#3560),#3016,.T.);
#16677=ADVANCED_FACE('',(#3561),#3017,.T.);
#16678=ADVANCED_FACE('',(#3562),#3018,.T.);
#16679=ADVANCED_FACE('',(#3563),#3019,.T.);
#16680=ADVANCED_FACE('',(#3564),#3020,.T.);
#16681=ADVANCED_FACE('',(#3565),#3021,.T.);
#16682=ADVANCED_FACE('',(#3566),#3022,.T.);
#16683=ADVANCED_FACE('',(#3567),#3023,.T.);
#16684=ADVANCED_FACE('',(#3568),#3024,.T.);
#16685=ADVANCED_FACE('',(#3569),#3025,.T.);
#16686=ADVANCED_FACE('',(#3570),#3026,.T.);
#16687=ADVANCED_FACE('',(#3571),#3027,.T.);
#16688=ADVANCED_FACE('',(#3572),#3028,.T.);
#16689=ADVANCED_FACE('',(#3573),#3029,.T.);
#16690=ADVANCED_FACE('',(#3574),#3030,.T.);
#16691=ADVANCED_FACE('',(#3575),#3031,.T.);
#16692=ADVANCED_FACE('',(#3576),#3032,.T.);
#16693=ADVANCED_FACE('',(#3577),#3033,.T.);
#16694=ADVANCED_FACE('',(#3578),#3034,.T.);
#16695=ADVANCED_FACE('',(#3579),#3035,.T.);
#16696=ADVANCED_FACE('',(#3580),#3036,.T.);
#16697=ADVANCED_FACE('',(#3581),#3037,.T.);
#16698=ADVANCED_FACE('',(#3582),#3038,.T.);
#16699=ADVANCED_FACE('',(#3583),#3039,.T.);
#16700=ADVANCED_FACE('',(#3584),#3040,.T.);
#16701=ADVANCED_FACE('',(#3585),#3041,.T.);
#16702=ADVANCED_FACE('',(#3586),#3042,.T.);
#16703=ADVANCED_FACE('',(#3587),#3043,.T.);
#16704=ADVANCED_FACE('',(#3588),#3044,.T.);
#16705=ADVANCED_FACE('',(#3589),#3045,.T.);
#16706=ADVANCED_FACE('',(#3590,#3478),#16556,.F.);
#16707=ADVANCED_FACE('',(#3591),#3046,.T.);
#16708=ADVANCED_FACE('',(#3592),#3047,.T.);
#16709=ADVANCED_FACE('',(#3593),#3048,.T.);
#16710=ADVANCED_FACE('',(#3594),#3049,.T.);
#16711=ADVANCED_FACE('',(#3595),#3050,.T.);
#16712=ADVANCED_FACE('',(#3596),#3051,.T.);
#16713=ADVANCED_FACE('',(#3597),#3052,.T.);
#16714=ADVANCED_FACE('',(#3598),#3053,.T.);
#16715=ADVANCED_FACE('',(#3599),#3054,.T.);
#16716=ADVANCED_FACE('',(#3600),#3055,.T.);
#16717=ADVANCED_FACE('',(#3601),#3056,.T.);
#16718=ADVANCED_FACE('',(#3602),#3057,.T.);
#16719=ADVANCED_FACE('',(#3603),#3058,.T.);
#16720=ADVANCED_FACE('',(#3604),#3059,.T.);
#16721=ADVANCED_FACE('',(#3605),#3060,.T.);
#16722=ADVANCED_FACE('',(#3606),#3061,.T.);
#16723=ADVANCED_FACE('',(#3607),#3062,.T.);
#16724=ADVANCED_FACE('',(#3608),#3063,.T.);
#16725=ADVANCED_FACE('',(#3609),#3064,.T.);
#16726=ADVANCED_FACE('',(#3610),#3065,.T.);
#16727=ADVANCED_FACE('',(#3611),#3066,.T.);
#16728=ADVANCED_FACE('',(#3612),#3067,.T.);
#16729=ADVANCED_FACE('',(#3613),#3068,.T.);
#16730=ADVANCED_FACE('',(#3614),#3069,.T.);
#16731=ADVANCED_FACE('',(#3615),#3070,.T.);
#16732=ADVANCED_FACE('',(#3616),#3071,.T.);
#16733=ADVANCED_FACE('',(#3617),#3072,.T.);
#16734=ADVANCED_FACE('',(#3618),#3073,.T.);
#16735=ADVANCED_FACE('',(#3619),#3074,.T.);
#16736=ADVANCED_FACE('',(#3620),#3075,.T.);
#16737=ADVANCED_FACE('',(#3621),#3076,.T.);
#16738=ADVANCED_FACE('',(#3622),#3077,.T.);
#16739=ADVANCED_FACE('',(#3623),#3078,.T.);
#16740=ADVANCED_FACE('',(#3624),#3079,.T.);
#16741=ADVANCED_FACE('',(#3625),#3080,.T.);
#16742=ADVANCED_FACE('',(#3626),#3081,.T.);
#16743=ADVANCED_FACE('',(#3627),#3082,.T.);
#16744=ADVANCED_FACE('',(#3628),#3083,.T.);
#16745=ADVANCED_FACE('',(#3629),#3084,.T.);
#16746=ADVANCED_FACE('',(#3630),#3085,.T.);
#16747=ADVANCED_FACE('',(#3631),#3086,.T.);
#16748=ADVANCED_FACE('',(#3632),#3087,.T.);
#16749=ADVANCED_FACE('',(#3633),#3088,.T.);
#16750=ADVANCED_FACE('',(#3634),#3089,.T.);
#16751=ADVANCED_FACE('',(#3635),#3090,.T.);
#16752=ADVANCED_FACE('',(#3636),#3091,.T.);
#16753=ADVANCED_FACE('',(#3637),#3092,.T.);
#16754=ADVANCED_FACE('',(#3638),#3093,.T.);
#16755=ADVANCED_FACE('',(#3639),#3094,.T.);
#16756=ADVANCED_FACE('',(#3640),#3095,.T.);
#16757=ADVANCED_FACE('',(#3641),#3096,.T.);
#16758=ADVANCED_FACE('',(#3642),#3097,.T.);
#16759=ADVANCED_FACE('',(#3643),#3098,.T.);
#16760=ADVANCED_FACE('',(#3644),#3099,.T.);
#16761=ADVANCED_FACE('',(#3645),#3100,.T.);
#16762=ADVANCED_FACE('',(#3646),#3101,.T.);
#16763=ADVANCED_FACE('',(#3647),#3102,.T.);
#16764=ADVANCED_FACE('',(#3648),#3103,.T.);
#16765=ADVANCED_FACE('',(#3649),#3104,.T.);
#16766=ADVANCED_FACE('',(#3650),#3105,.T.);
#16767=ADVANCED_FACE('',(#3651),#3106,.T.);
#16768=ADVANCED_FACE('',(#3652),#3107,.T.);
#16769=ADVANCED_FACE('',(#3653),#3108,.T.);
#16770=ADVANCED_FACE('',(#3654),#3109,.T.);
#16771=ADVANCED_FACE('',(#3655),#3110,.T.);
#16772=ADVANCED_FACE('',(#3656),#3111,.T.);
#16773=ADVANCED_FACE('',(#3657),#3112,.T.);
#16774=ADVANCED_FACE('',(#3658),#3113,.T.);
#16775=ADVANCED_FACE('',(#3659),#3114,.T.);
#16776=ADVANCED_FACE('',(#3660),#3115,.T.);
#16777=ADVANCED_FACE('',(#3661),#3116,.T.);
#16778=ADVANCED_FACE('',(#3662),#3117,.T.);
#16779=ADVANCED_FACE('',(#3663),#3118,.T.);
#16780=ADVANCED_FACE('',(#3664),#3119,.T.);
#16781=ADVANCED_FACE('',(#3665),#3120,.T.);
#16782=ADVANCED_FACE('',(#3666),#3121,.T.);
#16783=ADVANCED_FACE('',(#3667),#3122,.T.);
#16784=ADVANCED_FACE('',(#3668),#3123,.T.);
#16785=ADVANCED_FACE('',(#3669),#3124,.T.);
#16786=ADVANCED_FACE('',(#3670),#3125,.T.);
#16787=ADVANCED_FACE('',(#3671),#3126,.T.);
#16788=ADVANCED_FACE('',(#3672),#3127,.T.);
#16789=ADVANCED_FACE('',(#3673),#3128,.T.);
#16790=ADVANCED_FACE('',(#3674),#3129,.T.);
#16791=ADVANCED_FACE('',(#3675),#3130,.T.);
#16792=ADVANCED_FACE('',(#3676),#3131,.T.);
#16793=ADVANCED_FACE('',(#3677),#3132,.T.);
#16794=ADVANCED_FACE('',(#3678),#3133,.T.);
#16795=ADVANCED_FACE('',(#3679),#3134,.T.);
#16796=ADVANCED_FACE('',(#3680),#3135,.T.);
#16797=ADVANCED_FACE('',(#3681),#3136,.T.);
#16798=ADVANCED_FACE('',(#3682),#3137,.T.);
#16799=ADVANCED_FACE('',(#3683),#3138,.T.);
#16800=ADVANCED_FACE('',(#3684),#3139,.T.);
#16801=ADVANCED_FACE('',(#3685),#3140,.T.);
#16802=ADVANCED_FACE('',(#3686),#3141,.T.);
#16803=ADVANCED_FACE('',(#3687),#3142,.T.);
#16804=ADVANCED_FACE('',(#3688),#3143,.T.);
#16805=ADVANCED_FACE('',(#3689),#3144,.T.);
#16806=ADVANCED_FACE('',(#3690),#3145,.T.);
#16807=ADVANCED_FACE('',(#3691),#3146,.T.);
#16808=ADVANCED_FACE('',(#3692),#3147,.T.);
#16809=ADVANCED_FACE('',(#3693),#3148,.T.);
#16810=ADVANCED_FACE('',(#3694),#3149,.T.);
#16811=ADVANCED_FACE('',(#3695),#3150,.T.);
#16812=ADVANCED_FACE('',(#3696),#3151,.T.);
#16813=ADVANCED_FACE('',(#3697),#3152,.T.);
#16814=ADVANCED_FACE('',(#3698),#3153,.T.);
#16815=ADVANCED_FACE('',(#3699),#3154,.T.);
#16816=ADVANCED_FACE('',(#3700),#3155,.T.);
#16817=ADVANCED_FACE('',(#3701),#3156,.T.);
#16818=ADVANCED_FACE('',(#3702),#3157,.T.);
#16819=ADVANCED_FACE('',(#3703),#3158,.T.);
#16820=ADVANCED_FACE('',(#3704),#3159,.T.);
#16821=ADVANCED_FACE('',(#3705),#3160,.T.);
#16822=ADVANCED_FACE('',(#3706),#3161,.T.);
#16823=ADVANCED_FACE('',(#3707),#3162,.T.);
#16824=ADVANCED_FACE('',(#3708),#3163,.T.);
#16825=ADVANCED_FACE('',(#3709),#3164,.T.);
#16826=ADVANCED_FACE('',(#3710),#3165,.T.);
#16827=ADVANCED_FACE('',(#3711),#3166,.T.);
#16828=ADVANCED_FACE('',(#3712),#3167,.T.);
#16829=ADVANCED_FACE('',(#3713),#3168,.T.);
#16830=ADVANCED_FACE('',(#3714),#3169,.T.);
#16831=ADVANCED_FACE('',(#3715),#3170,.T.);
#16832=ADVANCED_FACE('',(#3716),#3171,.T.);
#16833=ADVANCED_FACE('',(#3717),#3172,.T.);
#16834=ADVANCED_FACE('',(#3718),#3173,.T.);
#16835=ADVANCED_FACE('',(#3719),#3174,.T.);
#16836=ADVANCED_FACE('',(#3720),#3175,.T.);
#16837=ADVANCED_FACE('',(#3721),#3176,.T.);
#16838=ADVANCED_FACE('',(#3722),#3177,.T.);
#16839=ADVANCED_FACE('',(#3723),#3178,.T.);
#16840=ADVANCED_FACE('',(#3724),#3179,.T.);
#16841=ADVANCED_FACE('',(#3725),#3180,.T.);
#16842=ADVANCED_FACE('',(#3726),#3181,.T.);
#16843=ADVANCED_FACE('',(#3727),#3182,.T.);
#16844=ADVANCED_FACE('',(#3728),#3183,.T.);
#16845=ADVANCED_FACE('',(#3729),#3184,.T.);
#16846=ADVANCED_FACE('',(#3730),#3185,.F.);
#16847=ADVANCED_FACE('',(#3731),#1530,.T.);
#16848=ADVANCED_FACE('',(#3732),#323,.T.);
#16849=ADVANCED_FACE('',(#3733),#3186,.F.);
#16850=ADVANCED_FACE('',(#3734),#3187,.T.);
#16851=ADVANCED_FACE('',(#3735),#3188,.T.);
#16852=ADVANCED_FACE('',(#3736),#3189,.T.);
#16853=ADVANCED_FACE('',(#3737,#3479),#16557,.F.);
#16854=ADVANCED_FACE('',(#3738,#3480),#16558,.T.);
#16855=ADVANCED_FACE('',(#3739),#3190,.T.);
#16856=ADVANCED_FACE('',(#3740),#3191,.T.);
#16857=ADVANCED_FACE('',(#3741),#3192,.T.);
#16858=ADVANCED_FACE('',(#3742),#3193,.T.);
#16859=ADVANCED_FACE('',(#3743),#3194,.T.);
#16860=ADVANCED_FACE('',(#3744),#3195,.T.);
#16861=ADVANCED_FACE('',(#3745),#3196,.T.);
#16862=ADVANCED_FACE('',(#3746),#3197,.T.);
#16863=ADVANCED_FACE('',(#3747),#3198,.T.);
#16864=ADVANCED_FACE('',(#3748),#3199,.T.);
#16865=ADVANCED_FACE('',(#3749),#3200,.T.);
#16866=ADVANCED_FACE('',(#3750),#3201,.T.);
#16867=ADVANCED_FACE('',(#3751),#3202,.T.);
#16868=ADVANCED_FACE('',(#3752),#324,.T.);
#16869=ADVANCED_FACE('',(#3753,#3481),#16559,.F.);
#16870=ADVANCED_FACE('',(#3754),#16560,.F.);
#16871=ADVANCED_FACE('',(#3755),#16561,.T.);
#16872=ADVANCED_FACE('',(#3756),#3203,.T.);
#16873=ADVANCED_FACE('',(#3757),#171,.T.);
#16874=ADVANCED_FACE('',(#3758),#172,.T.);
#16875=ADVANCED_FACE('',(#3759),#3204,.T.);
#16876=ADVANCED_FACE('',(#3760),#173,.F.);
#16877=ADVANCED_FACE('',(#3761),#174,.F.);
#16878=ADVANCED_FACE('',(#3762),#175,.T.);
#16879=ADVANCED_FACE('',(#3763),#176,.T.);
#16880=ADVANCED_FACE('',(#3764),#177,.T.);
#16881=ADVANCED_FACE('',(#3765),#178,.T.);
#16882=ADVANCED_FACE('',(#3766),#179,.T.);
#16883=ADVANCED_FACE('',(#3767),#180,.T.);
#16884=ADVANCED_FACE('',(#3768),#181,.T.);
#16885=ADVANCED_FACE('',(#3769),#182,.T.);
#16886=ADVANCED_FACE('',(#3770),#183,.T.);
#16887=ADVANCED_FACE('',(#3771),#184,.T.);
#16888=ADVANCED_FACE('',(#3772),#185,.T.);
#16889=ADVANCED_FACE('',(#3773),#186,.T.);
#16890=ADVANCED_FACE('',(#3774),#187,.T.);
#16891=ADVANCED_FACE('',(#3775),#188,.T.);
#16892=ADVANCED_FACE('',(#3776),#189,.T.);
#16893=ADVANCED_FACE('',(#3777),#190,.T.);
#16894=ADVANCED_FACE('',(#3778),#191,.T.);
#16895=ADVANCED_FACE('',(#3779),#1531,.T.);
#16896=ADVANCED_FACE('',(#3780),#142,.T.);
#16897=ADVANCED_FACE('',(#3781),#325,.F.);
#16898=ADVANCED_FACE('',(#3782),#326,.T.);
#16899=ADVANCED_FACE('',(#3783),#327,.T.);
#16900=ADVANCED_FACE('',(#3784,#3482,#3483),#328,.T.);
#16901=ADVANCED_FACE('',(#3785),#329,.T.);
#16902=ADVANCED_FACE('',(#3786),#3205,.T.);
#16903=ADVANCED_FACE('',(#3787,#3484,#3485,#3486,#3487,#3488,#3489,#3490,
#3491,#3492,#3493,#3494,#3495,#3496,#3497,#3498,#3499,#3500),#330,.T.);
#16904=ADVANCED_FACE('',(#3788),#331,.T.);
#16905=ADVANCED_FACE('',(#3789),#332,.T.);
#16906=ADVANCED_FACE('',(#3790),#1532,.T.);
#16907=ADVANCED_FACE('',(#3791),#131,.T.);
#16908=ADVANCED_FACE('',(#3792),#16562,.F.);
#16909=ADVANCED_FACE('',(#3793),#16563,.F.);
#16910=ADVANCED_FACE('',(#3794),#16564,.F.);
#16911=ADVANCED_FACE('',(#3795),#16565,.F.);
#16912=ADVANCED_FACE('',(#3796),#3206,.T.);
#16913=ADVANCED_FACE('',(#3797),#333,.F.);
#16914=ADVANCED_FACE('',(#3798),#3207,.T.);
#16915=ADVANCED_FACE('',(#3799),#3208,.F.);
#16916=ADVANCED_FACE('',(#3800),#3209,.F.);
#16917=ADVANCED_FACE('',(#3801),#3210,.T.);
#16918=ADVANCED_FACE('',(#3802),#16566,.F.);
#16919=ADVANCED_FACE('',(#3803),#3211,.F.);
#16920=ADVANCED_FACE('',(#3804),#3212,.F.);
#16921=ADVANCED_FACE('',(#3805),#16567,.F.);
#16922=ADVANCED_FACE('',(#3806),#3213,.T.);
#16923=ADVANCED_FACE('',(#3807),#3214,.T.);
#16924=ADVANCED_FACE('',(#3808),#3215,.T.);
#16925=ADVANCED_FACE('',(#3809),#3216,.T.);
#16926=ADVANCED_FACE('',(#3810),#1533,.T.);
#16927=ADVANCED_FACE('',(#3811),#192,.F.);
#16928=ADVANCED_FACE('',(#3812),#193,.F.);
#16929=ADVANCED_FACE('',(#3813),#1534,.T.);
#16930=ADVANCED_FACE('',(#3814),#1535,.T.);
#16931=ADVANCED_FACE('',(#3815),#194,.T.);
#16932=ADVANCED_FACE('',(#3816),#195,.T.);
#16933=ADVANCED_FACE('',(#3817),#1536,.T.);
#16934=ADVANCED_FACE('',(#3818),#1537,.T.);
#16935=ADVANCED_FACE('',(#3819),#196,.F.);
#16936=ADVANCED_FACE('',(#3820),#197,.F.);
#16937=ADVANCED_FACE('',(#3821),#1538,.T.);
#16938=ADVANCED_FACE('',(#3822),#1539,.T.);
#16939=ADVANCED_FACE('',(#3823),#198,.T.);
#16940=ADVANCED_FACE('',(#3824),#199,.T.);
#16941=ADVANCED_FACE('',(#3825),#1540,.T.);
#16942=ADVANCED_FACE('',(#3826),#143,.T.);
#16943=ADVANCED_FACE('',(#3827),#200,.T.);
#16944=ADVANCED_FACE('',(#3828),#3217,.T.);
#16945=ADVANCED_FACE('',(#3829),#1541,.T.);
#16946=ADVANCED_FACE('',(#3830),#3218,.T.);
#16947=ADVANCED_FACE('',(#3831),#1542,.T.);
#16948=ADVANCED_FACE('',(#3832),#132,.T.);
#16949=ADVANCED_FACE('',(#3833),#133,.T.);
#16950=ADVANCED_FACE('',(#3834),#1543,.T.);
#16951=ADVANCED_FACE('',(#3835),#144,.T.);
#16952=ADVANCED_FACE('',(#3836),#134,.T.);
#16953=ADVANCED_FACE('',(#3837),#1544,.T.);
#16954=ADVANCED_FACE('',(#3838),#145,.T.);
#16955=ADVANCED_FACE('',(#3839),#201,.T.);
#16956=ADVANCED_FACE('',(#3840),#146,.T.);
#16957=ADVANCED_FACE('',(#3841),#135,.T.);
#16958=ADVANCED_FACE('',(#3842),#1545,.T.);
#16959=ADVANCED_FACE('',(#3843),#3219,.T.);
#16960=ADVANCED_FACE('',(#3844),#1546,.T.);
#16961=ADVANCED_FACE('',(#3845),#3220,.T.);
#16962=ADVANCED_FACE('',(#3846),#147,.T.);
#16963=ADVANCED_FACE('',(#3847),#202,.T.);
#16964=ADVANCED_FACE('',(#3848),#148,.T.);
#16965=ADVANCED_FACE('',(#3849),#203,.T.);
#16966=ADVANCED_FACE('',(#3850),#1547,.T.);
#16967=ADVANCED_FACE('',(#3851),#1548,.T.);
#16968=ADVANCED_FACE('',(#3852),#204,.T.);
#16969=ADVANCED_FACE('',(#3853),#136,.T.);
#16970=ADVANCED_FACE('',(#3854),#334,.T.);
#16971=ADVANCED_FACE('',(#3855),#3221,.T.);
#16972=ADVANCED_FACE('',(#3856),#3222,.T.);
#16973=ADVANCED_FACE('',(#3857),#3223,.T.);
#16974=ADVANCED_FACE('',(#3858),#3224,.T.);
#16975=ADVANCED_FACE('',(#3859),#3225,.T.);
#16976=ADVANCED_FACE('',(#3860),#3226,.T.);
#16977=ADVANCED_FACE('',(#3861),#3227,.T.);
#16978=ADVANCED_FACE('',(#3862),#3228,.T.);
#16979=ADVANCED_FACE('',(#3863),#3229,.T.);
#16980=ADVANCED_FACE('',(#3864),#3230,.T.);
#16981=ADVANCED_FACE('',(#3865),#3231,.T.);
#16982=ADVANCED_FACE('',(#3866),#3232,.T.);
#16983=ADVANCED_FACE('',(#3867),#3233,.T.);
#16984=ADVANCED_FACE('',(#3868),#3234,.T.);
#16985=ADVANCED_FACE('',(#3869),#3235,.T.);
#16986=ADVANCED_FACE('',(#3870),#3236,.T.);
#16987=ADVANCED_FACE('',(#3871),#3237,.T.);
#16988=ADVANCED_FACE('',(#3872),#137,.T.);
#16989=ADVANCED_FACE('',(#3873),#138,.T.);
#16990=ADVANCED_FACE('',(#3874),#3238,.T.);
#16991=ADVANCED_FACE('',(#3875),#3239,.T.);
#16992=ADVANCED_FACE('',(#3876),#3240,.T.);
#16993=ADVANCED_FACE('',(#3877),#3241,.T.);
#16994=ADVANCED_FACE('',(#3878),#3242,.T.);
#16995=ADVANCED_FACE('',(#3879),#3243,.T.);
#16996=ADVANCED_FACE('',(#3880),#3244,.T.);
#16997=ADVANCED_FACE('',(#3881),#3245,.T.);
#16998=ADVANCED_FACE('',(#3882),#3246,.T.);
#16999=ADVANCED_FACE('',(#3883),#3247,.T.);
#17000=ADVANCED_FACE('',(#3884),#3248,.T.);
#17001=ADVANCED_FACE('',(#3885),#3249,.T.);
#17002=ADVANCED_FACE('',(#3886),#3250,.T.);
#17003=ADVANCED_FACE('',(#3887),#3251,.T.);
#17004=ADVANCED_FACE('',(#3888),#3252,.T.);
#17005=ADVANCED_FACE('',(#3889),#3253,.T.);
#17006=ADVANCED_FACE('',(#3890),#3254,.T.);
#17007=ADVANCED_FACE('',(#3891),#139,.F.);
#17008=ADVANCED_FACE('',(#3892),#140,.F.);
#17009=ADVANCED_FACE('',(#3893),#1549,.T.);
#17010=ADVANCED_FACE('',(#3894),#3255,.T.);
#17011=ADVANCED_FACE('',(#3895),#1550,.T.);
#17012=ADVANCED_FACE('',(#3896),#1551,.T.);
#17013=ADVANCED_FACE('',(#3897),#3256,.T.);
#17014=ADVANCED_FACE('',(#3898),#205,.T.);
#17015=ADVANCED_FACE('',(#3899),#1552,.T.);
#17016=ADVANCED_FACE('',(#3900),#3257,.T.);
#17017=ADVANCED_FACE('',(#3901),#1553,.T.);
#17018=ADVANCED_FACE('',(#3902),#1554,.T.);
#17019=ADVANCED_FACE('',(#3903),#3258,.T.);
#17020=ADVANCED_FACE('',(#3904),#1555,.T.);
#17021=ADVANCED_FACE('',(#3905),#1556,.T.);
#17022=ADVANCED_FACE('',(#3906),#3259,.T.);
#17023=ADVANCED_FACE('',(#3907),#1557,.T.);
#17024=ADVANCED_FACE('',(#3908),#1558,.T.);
#17025=ADVANCED_FACE('',(#3909),#3260,.T.);
#17026=ADVANCED_FACE('',(#3910),#1559,.T.);
#17027=ADVANCED_FACE('',(#3911),#1560,.T.);
#17028=ADVANCED_FACE('',(#3912),#3261,.T.);
#17029=ADVANCED_FACE('',(#3913),#1561,.T.);
#17030=ADVANCED_FACE('',(#3914),#1562,.T.);
#17031=ADVANCED_FACE('',(#3915),#3262,.T.);
#17032=ADVANCED_FACE('',(#3916),#1563,.T.);
#17033=ADVANCED_FACE('',(#3917),#1564,.T.);
#17034=ADVANCED_FACE('',(#3918),#3263,.T.);
#17035=ADVANCED_FACE('',(#3919),#1565,.T.);
#17036=ADVANCED_FACE('',(#3920),#1566,.T.);
#17037=ADVANCED_FACE('',(#3921),#3264,.T.);
#17038=ADVANCED_FACE('',(#3922),#1567,.T.);
#17039=ADVANCED_FACE('',(#3923),#1568,.T.);
#17040=ADVANCED_FACE('',(#3924),#3265,.T.);
#17041=ADVANCED_FACE('',(#3925),#1569,.T.);
#17042=ADVANCED_FACE('',(#3926),#1570,.T.);
#17043=ADVANCED_FACE('',(#3927),#3266,.T.);
#17044=ADVANCED_FACE('',(#3928),#1571,.T.);
#17045=ADVANCED_FACE('',(#3929),#1572,.T.);
#17046=ADVANCED_FACE('',(#3930),#3267,.T.);
#17047=ADVANCED_FACE('',(#3931),#1573,.T.);
#17048=ADVANCED_FACE('',(#3932),#1574,.T.);
#17049=ADVANCED_FACE('',(#3933),#3268,.T.);
#17050=ADVANCED_FACE('',(#3934),#1575,.T.);
#17051=ADVANCED_FACE('',(#3935),#1576,.T.);
#17052=ADVANCED_FACE('',(#3936),#3269,.T.);
#17053=ADVANCED_FACE('',(#3937),#1577,.T.);
#17054=ADVANCED_FACE('',(#3938),#1578,.T.);
#17055=ADVANCED_FACE('',(#3939),#3270,.T.);
#17056=ADVANCED_FACE('',(#3940),#1579,.T.);
#17057=ADVANCED_FACE('',(#3941),#1580,.T.);
#17058=ADVANCED_FACE('',(#3942),#3271,.T.);
#17059=ADVANCED_FACE('',(#3943),#1581,.T.);
#17060=ADVANCED_FACE('',(#3944),#1582,.T.);
#17061=ADVANCED_FACE('',(#3945),#3272,.T.);
#17062=ADVANCED_FACE('',(#3946),#1583,.T.);
#17063=ADVANCED_FACE('',(#3947),#1584,.T.);
#17064=ADVANCED_FACE('',(#3948),#3273,.T.);
#17065=ADVANCED_FACE('',(#3949),#1585,.T.);
#17066=ADVANCED_FACE('',(#3950),#1586,.T.);
#17067=ADVANCED_FACE('',(#3951),#3274,.T.);
#17068=ADVANCED_FACE('',(#3952),#1587,.T.);
#17069=ADVANCED_FACE('',(#3953),#1588,.T.);
#17070=ADVANCED_FACE('',(#3954),#3275,.T.);
#17071=ADVANCED_FACE('',(#3955),#1589,.T.);
#17072=ADVANCED_FACE('',(#3956),#1590,.T.);
#17073=ADVANCED_FACE('',(#3957),#3276,.T.);
#17074=ADVANCED_FACE('',(#3958),#1591,.T.);
#17075=ADVANCED_FACE('',(#3959),#1592,.T.);
#17076=ADVANCED_FACE('',(#3960),#3277,.T.);
#17077=ADVANCED_FACE('',(#3961),#1593,.T.);
#17078=ADVANCED_FACE('',(#3962),#1594,.T.);
#17079=ADVANCED_FACE('',(#3963),#3278,.T.);
#17080=ADVANCED_FACE('',(#3964),#1595,.T.);
#17081=ADVANCED_FACE('',(#3965),#1596,.T.);
#17082=ADVANCED_FACE('',(#3966),#3279,.T.);
#17083=ADVANCED_FACE('',(#3967),#1597,.T.);
#17084=ADVANCED_FACE('',(#3968),#1598,.T.);
#17085=ADVANCED_FACE('',(#3969),#3280,.T.);
#17086=ADVANCED_FACE('',(#3970),#1599,.T.);
#17087=ADVANCED_FACE('',(#3971),#1600,.T.);
#17088=ADVANCED_FACE('',(#3972),#1601,.T.);
#17089=ADVANCED_FACE('',(#3973),#1602,.T.);
#17090=ADVANCED_FACE('',(#3974),#1603,.T.);
#17091=ADVANCED_FACE('',(#3975),#1604,.T.);
#17092=ADVANCED_FACE('',(#3976),#1605,.T.);
#17093=ADVANCED_FACE('',(#3977),#1606,.T.);
#17094=ADVANCED_FACE('',(#3978),#1607,.T.);
#17095=ADVANCED_FACE('',(#3979),#206,.T.);
#17096=ADVANCED_FACE('',(#3980),#1608,.T.);
#17097=ADVANCED_FACE('',(#3981),#1609,.T.);
#17098=ADVANCED_FACE('',(#3982),#1610,.T.);
#17099=ADVANCED_FACE('',(#3983),#1611,.T.);
#17100=ADVANCED_FACE('',(#3984),#3281,.T.);
#17101=ADVANCED_FACE('',(#3985),#1612,.T.);
#17102=ADVANCED_FACE('',(#3986),#1613,.T.);
#17103=ADVANCED_FACE('',(#3987),#3282,.T.);
#17104=ADVANCED_FACE('',(#3988),#1614,.T.);
#17105=ADVANCED_FACE('',(#3989),#1615,.T.);
#17106=ADVANCED_FACE('',(#3990),#1616,.T.);
#17107=ADVANCED_FACE('',(#3991),#207,.T.);
#17108=ADVANCED_FACE('',(#3992),#208,.T.);
#17109=ADVANCED_FACE('',(#3993),#209,.T.);
#17110=ADVANCED_FACE('',(#3994),#1617,.T.);
#17111=ADVANCED_FACE('',(#3995),#1618,.T.);
#17112=ADVANCED_FACE('',(#3996),#210,.T.);
#17113=ADVANCED_FACE('',(#3997),#3283,.T.);
#17114=ADVANCED_FACE('',(#3998),#3284,.T.);
#17115=ADVANCED_FACE('',(#3999),#1619,.T.);
#17116=ADVANCED_FACE('',(#4000),#1620,.T.);
#17117=ADVANCED_FACE('',(#4001),#1621,.T.);
#17118=ADVANCED_FACE('',(#4002),#1622,.T.);
#17119=ADVANCED_FACE('',(#4003),#3285,.T.);
#17120=ADVANCED_FACE('',(#4004),#3286,.T.);
#17121=ADVANCED_FACE('',(#4005),#1623,.T.);
#17122=ADVANCED_FACE('',(#4006),#1624,.T.);
#17123=ADVANCED_FACE('',(#4007),#1625,.T.);
#17124=ADVANCED_FACE('',(#4008),#1626,.T.);
#17125=ADVANCED_FACE('',(#4009),#3287,.T.);
#17126=ADVANCED_FACE('',(#4010),#3288,.T.);
#17127=ADVANCED_FACE('',(#4011),#1627,.T.);
#17128=ADVANCED_FACE('',(#4012),#1628,.T.);
#17129=ADVANCED_FACE('',(#4013),#1629,.T.);
#17130=ADVANCED_FACE('',(#4014),#1630,.T.);
#17131=ADVANCED_FACE('',(#4015),#3289,.T.);
#17132=ADVANCED_FACE('',(#4016),#3290,.T.);
#17133=ADVANCED_FACE('',(#4017),#1631,.T.);
#17134=ADVANCED_FACE('',(#4018),#1632,.T.);
#17135=ADVANCED_FACE('',(#4019),#1633,.T.);
#17136=ADVANCED_FACE('',(#4020),#1634,.T.);
#17137=ADVANCED_FACE('',(#4021),#3291,.T.);
#17138=ADVANCED_FACE('',(#4022),#3292,.T.);
#17139=ADVANCED_FACE('',(#4023),#1635,.T.);
#17140=ADVANCED_FACE('',(#4024),#1636,.T.);
#17141=ADVANCED_FACE('',(#4025),#1637,.T.);
#17142=ADVANCED_FACE('',(#4026),#1638,.T.);
#17143=ADVANCED_FACE('',(#4027),#3293,.T.);
#17144=ADVANCED_FACE('',(#4028),#3294,.T.);
#17145=ADVANCED_FACE('',(#4029),#1639,.T.);
#17146=ADVANCED_FACE('',(#4030),#1640,.T.);
#17147=ADVANCED_FACE('',(#4031),#1641,.T.);
#17148=ADVANCED_FACE('',(#4032),#1642,.T.);
#17149=ADVANCED_FACE('',(#4033),#3295,.T.);
#17150=ADVANCED_FACE('',(#4034),#3296,.T.);
#17151=ADVANCED_FACE('',(#4035),#1643,.T.);
#17152=ADVANCED_FACE('',(#4036),#1644,.T.);
#17153=ADVANCED_FACE('',(#4037),#1645,.T.);
#17154=ADVANCED_FACE('',(#4038),#1646,.T.);
#17155=ADVANCED_FACE('',(#4039),#3297,.T.);
#17156=ADVANCED_FACE('',(#4040),#3298,.T.);
#17157=ADVANCED_FACE('',(#4041),#1647,.T.);
#17158=ADVANCED_FACE('',(#4042),#1648,.T.);
#17159=ADVANCED_FACE('',(#4043),#1649,.T.);
#17160=ADVANCED_FACE('',(#4044),#335,.T.);
#17161=ADVANCED_FACE('',(#4045),#3299,.T.);
#17162=ADVANCED_FACE('',(#4046),#3300,.T.);
#17163=ADVANCED_FACE('',(#4047),#1650,.T.);
#17164=ADVANCED_FACE('',(#4048),#1651,.T.);
#17165=ADVANCED_FACE('',(#4049),#1652,.T.);
#17166=ADVANCED_FACE('',(#4050),#336,.T.);
#17167=ADVANCED_FACE('',(#4051),#3301,.T.);
#17168=ADVANCED_FACE('',(#4052),#3302,.T.);
#17169=ADVANCED_FACE('',(#4053),#1653,.T.);
#17170=ADVANCED_FACE('',(#4054),#1654,.T.);
#17171=ADVANCED_FACE('',(#4055),#1655,.T.);
#17172=ADVANCED_FACE('',(#4056),#1656,.T.);
#17173=ADVANCED_FACE('',(#4057),#3303,.T.);
#17174=ADVANCED_FACE('',(#4058),#3304,.T.);
#17175=ADVANCED_FACE('',(#4059),#1657,.T.);
#17176=ADVANCED_FACE('',(#4060),#1658,.T.);
#17177=ADVANCED_FACE('',(#4061),#1659,.T.);
#17178=ADVANCED_FACE('',(#4062),#1660,.T.);
#17179=ADVANCED_FACE('',(#4063),#3305,.T.);
#17180=ADVANCED_FACE('',(#4064),#3306,.T.);
#17181=ADVANCED_FACE('',(#4065),#1661,.T.);
#17182=ADVANCED_FACE('',(#4066),#1662,.T.);
#17183=ADVANCED_FACE('',(#4067),#1663,.T.);
#17184=ADVANCED_FACE('',(#4068),#1664,.T.);
#17185=ADVANCED_FACE('',(#4069),#3307,.T.);
#17186=ADVANCED_FACE('',(#4070),#3308,.T.);
#17187=ADVANCED_FACE('',(#4071),#1665,.T.);
#17188=ADVANCED_FACE('',(#4072),#1666,.T.);
#17189=ADVANCED_FACE('',(#4073),#1667,.T.);
#17190=ADVANCED_FACE('',(#4074),#1668,.T.);
#17191=ADVANCED_FACE('',(#4075),#1669,.T.);
#17192=ADVANCED_FACE('',(#4076),#1670,.T.);
#17193=ADVANCED_FACE('',(#4077),#1671,.T.);
#17194=ADVANCED_FACE('',(#4078),#1672,.T.);
#17195=ADVANCED_FACE('',(#4079),#1673,.T.);
#17196=ADVANCED_FACE('',(#4080),#1674,.T.);
#17197=ADVANCED_FACE('',(#4081),#1675,.T.);
#17198=ADVANCED_FACE('',(#4082),#1676,.T.);
#17199=ADVANCED_FACE('',(#4083),#1677,.T.);
#17200=ADVANCED_FACE('',(#4084),#211,.T.);
#17201=ADVANCED_FACE('',(#4085),#1678,.T.);
#17202=ADVANCED_FACE('',(#4086),#1679,.T.);
#17203=ADVANCED_FACE('',(#4087),#3309,.T.);
#17204=ADVANCED_FACE('',(#4088),#3310,.T.);
#17205=ADVANCED_FACE('',(#4089),#1680,.T.);
#17206=ADVANCED_FACE('',(#4090),#1681,.T.);
#17207=ADVANCED_FACE('',(#4091),#1682,.T.);
#17208=ADVANCED_FACE('',(#4092),#1683,.T.);
#17209=ADVANCED_FACE('',(#4093),#212,.T.);
#17210=ADVANCED_FACE('',(#4094),#213,.T.);
#17211=ADVANCED_FACE('',(#4095),#214,.T.);
#17212=ADVANCED_FACE('',(#4096),#1684,.T.);
#17213=ADVANCED_FACE('',(#4097),#215,.T.);
#17214=ADVANCED_FACE('',(#4098),#216,.T.);
#17215=ADVANCED_FACE('',(#4099),#217,.T.);
#17216=ADVANCED_FACE('',(#4100),#3311,.T.);
#17217=ADVANCED_FACE('',(#4101),#1685,.T.);
#17218=ADVANCED_FACE('',(#4102),#218,.T.);
#17219=ADVANCED_FACE('',(#4103),#1686,.T.);
#17220=ADVANCED_FACE('',(#4104),#219,.T.);
#17221=ADVANCED_FACE('',(#4105),#220,.T.);
#17222=ADVANCED_FACE('',(#4106),#1687,.T.);
#17223=ADVANCED_FACE('',(#4107),#221,.T.);
#17224=ADVANCED_FACE('',(#4108),#1688,.T.);
#17225=ADVANCED_FACE('',(#4109),#222,.T.);
#17226=ADVANCED_FACE('',(#4110),#1689,.T.);
#17227=ADVANCED_FACE('',(#4111),#3312,.T.);
#17228=ADVANCED_FACE('',(#4112),#1690,.T.);
#17229=ADVANCED_FACE('',(#4113),#223,.T.);
#17230=ADVANCED_FACE('',(#4114),#224,.T.);
#17231=ADVANCED_FACE('',(#4115),#225,.T.);
#17232=ADVANCED_FACE('',(#4116),#226,.T.);
#17233=ADVANCED_FACE('',(#4117),#1691,.T.);
#17234=ADVANCED_FACE('',(#4118),#3313,.T.);
#17235=ADVANCED_FACE('',(#4119),#1692,.T.);
#17236=ADVANCED_FACE('',(#4120),#227,.T.);
#17237=ADVANCED_FACE('',(#4121),#1693,.T.);
#17238=ADVANCED_FACE('',(#4122),#228,.T.);
#17239=ADVANCED_FACE('',(#4123),#1694,.T.);
#17240=ADVANCED_FACE('',(#4124),#229,.T.);
#17241=ADVANCED_FACE('',(#4125),#230,.T.);
#17242=ADVANCED_FACE('',(#4126),#1695,.T.);
#17243=ADVANCED_FACE('',(#4127),#231,.T.);
#17244=ADVANCED_FACE('',(#4128),#1696,.T.);
#17245=ADVANCED_FACE('',(#4129),#3314,.T.);
#17246=ADVANCED_FACE('',(#4130),#232,.T.);
#17247=ADVANCED_FACE('',(#4131),#233,.T.);
#17248=ADVANCED_FACE('',(#4132),#234,.T.);
#17249=ADVANCED_FACE('',(#4133),#1697,.T.);
#17250=ADVANCED_FACE('',(#4134),#1698,.T.);
#17251=ADVANCED_FACE('',(#4135),#1699,.T.);
#17252=ADVANCED_FACE('',(#4136),#1700,.T.);
#17253=ADVANCED_FACE('',(#4137),#1701,.T.);
#17254=ADVANCED_FACE('',(#4138),#1702,.F.);
#17255=ADVANCED_FACE('',(#4139),#1703,.T.);
#17256=ADVANCED_FACE('',(#4140,#3501),#16568,.F.);
#17257=ADVANCED_FACE('',(#4141),#3315,.T.);
#17258=ADVANCED_FACE('',(#4142),#16569,.T.);
#17259=ADVANCED_FACE('',(#4143,#3502),#16570,.T.);
#17260=ADVANCED_FACE('',(#4144),#3316,.F.);
#17261=ADVANCED_FACE('',(#4145,#3503),#3317,.F.);
#17262=ADVANCED_FACE('',(#4146),#3318,.F.);
#17263=ADVANCED_FACE('',(#4147),#3319,.F.);
#17264=ADVANCED_FACE('',(#4148),#3320,.T.);
#17265=ADVANCED_FACE('',(#4149),#3321,.T.);
#17266=ADVANCED_FACE('',(#4150),#3322,.T.);
#17267=ADVANCED_FACE('',(#4151),#3323,.T.);
#17268=ADVANCED_FACE('',(#4152),#3324,.T.);
#17269=ADVANCED_FACE('',(#4153,#3504),#16571,.T.);
#17270=ADVANCED_FACE('',(#4154),#235,.T.);
#17271=ADVANCED_FACE('',(#4155),#3325,.F.);
#17272=ADVANCED_FACE('',(#4156),#16572,.T.);
#17273=ADVANCED_FACE('',(#4157),#3326,.T.);
#17274=ADVANCED_FACE('',(#4158),#3327,.F.);
#17275=ADVANCED_FACE('',(#4159,#3505),#16573,.T.);
#17276=ADVANCED_FACE('',(#4160),#16574,.F.);
#17277=ADVANCED_FACE('',(#4161),#3328,.F.);
#17278=ADVANCED_FACE('',(#4162),#1704,.T.);
#17279=ADVANCED_FACE('',(#4163),#1705,.F.);
#17280=ADVANCED_FACE('',(#4164),#236,.T.);
#17281=ADVANCED_FACE('',(#4165),#1706,.T.);
#17282=ADVANCED_FACE('',(#4166),#237,.F.);
#17283=ADVANCED_FACE('',(#4167),#238,.T.);
#17284=ADVANCED_FACE('',(#4168),#239,.T.);
#17285=ADVANCED_FACE('',(#4169,#3506),#16575,.T.);
#17286=ADVANCED_FACE('',(#4170,#3507),#16576,.T.);
#17287=ADVANCED_FACE('',(#4171),#16577,.T.);
#17288=ADVANCED_FACE('',(#4172),#16578,.T.);
#17289=ADVANCED_FACE('',(#4173),#16579,.T.);
#17290=ADVANCED_FACE('',(#4174),#16580,.T.);
#17291=ADVANCED_FACE('',(#4175),#16581,.T.);
#17292=ADVANCED_FACE('',(#4176),#16582,.T.);
#17293=ADVANCED_FACE('',(#4177),#16583,.T.);
#17294=ADVANCED_FACE('',(#4178),#16584,.T.);
#17295=ADVANCED_FACE('',(#4179),#16585,.T.);
#17296=ADVANCED_FACE('',(#4180),#3329,.T.);
#17297=ADVANCED_FACE('',(#4181),#16586,.T.);
#17298=ADVANCED_FACE('',(#4182),#16587,.T.);
#17299=ADVANCED_FACE('',(#4183),#16588,.T.);
#17300=ADVANCED_FACE('',(#4184),#16589,.T.);
#17301=ADVANCED_FACE('',(#4185),#16590,.T.);
#17302=ADVANCED_FACE('',(#4186),#3330,.F.);
#17303=ADVANCED_FACE('',(#4187),#3331,.T.);
#17304=ADVANCED_FACE('',(#4188),#3332,.T.);
#17305=ADVANCED_FACE('',(#4189),#3333,.T.);
#17306=ADVANCED_FACE('',(#4190),#3334,.T.);
#17307=ADVANCED_FACE('',(#4191),#3335,.T.);
#17308=ADVANCED_FACE('',(#4192),#3336,.T.);
#17309=ADVANCED_FACE('',(#4193),#3337,.T.);
#17310=ADVANCED_FACE('',(#4194),#3338,.T.);
#17311=ADVANCED_FACE('',(#4195),#3339,.T.);
#17312=ADVANCED_FACE('',(#4196),#3340,.T.);
#17313=ADVANCED_FACE('',(#4197),#3341,.T.);
#17314=ADVANCED_FACE('',(#4198),#3342,.T.);
#17315=ADVANCED_FACE('',(#4199),#3343,.T.);
#17316=ADVANCED_FACE('',(#4200),#3344,.T.);
#17317=ADVANCED_FACE('',(#4201),#3345,.T.);
#17318=ADVANCED_FACE('',(#4202),#3346,.T.);
#17319=ADVANCED_FACE('',(#4203),#3347,.T.);
#17320=ADVANCED_FACE('',(#4204),#3348,.T.);
#17321=ADVANCED_FACE('',(#4205),#3349,.T.);
#17322=ADVANCED_FACE('',(#4206),#3350,.T.);
#17323=ADVANCED_FACE('',(#4207),#3351,.T.);
#17324=ADVANCED_FACE('',(#4208),#3352,.T.);
#17325=ADVANCED_FACE('',(#4209),#3353,.F.);
#17326=ADVANCED_FACE('',(#4210),#3354,.T.);
#17327=ADVANCED_FACE('',(#4211),#3355,.T.);
#17328=ADVANCED_FACE('',(#4212),#3356,.T.);
#17329=ADVANCED_FACE('',(#4213),#240,.T.);
#17330=ADVANCED_FACE('',(#4214),#241,.T.);
#17331=ADVANCED_FACE('',(#4215),#3357,.T.);
#17332=ADVANCED_FACE('',(#4216),#3358,.T.);
#17333=ADVANCED_FACE('',(#4217),#242,.T.);
#17334=ADVANCED_FACE('',(#4218),#243,.T.);
#17335=ADVANCED_FACE('',(#4219),#3359,.T.);
#17336=ADVANCED_FACE('',(#4220),#244,.T.);
#17337=ADVANCED_FACE('',(#4221),#245,.T.);
#17338=ADVANCED_FACE('',(#4222),#3360,.F.);
#17339=ADVANCED_FACE('',(#4223),#246,.T.);
#17340=ADVANCED_FACE('',(#4224),#247,.T.);
#17341=ADVANCED_FACE('',(#4225),#3361,.T.);
#17342=ADVANCED_FACE('',(#4226),#16591,.F.);
#17343=ADVANCED_FACE('',(#4227),#16592,.F.);
#17344=ADVANCED_FACE('',(#4228),#16593,.F.);
#17345=ADVANCED_FACE('',(#4229),#16594,.F.);
#17346=ADVANCED_FACE('',(#4230),#16595,.F.);
#17347=ADVANCED_FACE('',(#4231),#16596,.F.);
#17348=ADVANCED_FACE('',(#4232),#16597,.F.);
#17349=ADVANCED_FACE('',(#4233),#16598,.F.);
#17350=ADVANCED_FACE('',(#4234),#16599,.F.);
#17351=ADVANCED_FACE('',(#4235),#16600,.F.);
#17352=ADVANCED_FACE('',(#4236),#16601,.F.);
#17353=ADVANCED_FACE('',(#4237),#16602,.F.);
#17354=ADVANCED_FACE('',(#4238),#16603,.F.);
#17355=ADVANCED_FACE('',(#4239),#16604,.F.);
#17356=ADVANCED_FACE('',(#4240,#3508),#16605,.T.);
#17357=ADVANCED_FACE('',(#4241,#3509),#16606,.T.);
#17358=ADVANCED_FACE('',(#4242),#3362,.F.);
#17359=ADVANCED_FACE('',(#4243),#3363,.T.);
#17360=ADVANCED_FACE('',(#4244),#3364,.T.);
#17361=ADVANCED_FACE('',(#4245),#3365,.T.);
#17362=ADVANCED_FACE('',(#4246),#3366,.T.);
#17363=ADVANCED_FACE('',(#4247),#3367,.T.);
#17364=ADVANCED_FACE('',(#4248),#3368,.T.);
#17365=ADVANCED_FACE('',(#4249),#3369,.T.);
#17366=ADVANCED_FACE('',(#4250),#3370,.T.);
#17367=ADVANCED_FACE('',(#4251),#3371,.T.);
#17368=ADVANCED_FACE('',(#4252),#3372,.T.);
#17369=ADVANCED_FACE('',(#4253),#3373,.T.);
#17370=ADVANCED_FACE('',(#4254),#3374,.T.);
#17371=ADVANCED_FACE('',(#4255),#3375,.T.);
#17372=ADVANCED_FACE('',(#4256),#3376,.T.);
#17373=ADVANCED_FACE('',(#4257),#3377,.T.);
#17374=ADVANCED_FACE('',(#4258),#3378,.T.);
#17375=ADVANCED_FACE('',(#4259),#3379,.T.);
#17376=ADVANCED_FACE('',(#4260),#3380,.T.);
#17377=ADVANCED_FACE('',(#4261),#3381,.T.);
#17378=ADVANCED_FACE('',(#4262),#3382,.T.);
#17379=ADVANCED_FACE('',(#4263),#3383,.T.);
#17380=ADVANCED_FACE('',(#4264),#3384,.T.);
#17381=ADVANCED_FACE('',(#4265),#149,.T.);
#17382=ADVANCED_FACE('',(#4266),#150,.T.);
#17383=ADVANCED_FACE('',(#4267),#3385,.T.);
#17384=ADVANCED_FACE('',(#4268),#3386,.T.);
#17385=ADVANCED_FACE('',(#4269),#3387,.T.);
#17386=ADVANCED_FACE('',(#4270),#3388,.F.);
#17387=ADVANCED_FACE('',(#4271),#3389,.T.);
#17388=ADVANCED_FACE('',(#4272),#3390,.T.);
#17389=ADVANCED_FACE('',(#4273),#3391,.F.);
#17390=ADVANCED_FACE('',(#4274),#248,.T.);
#17391=ADVANCED_FACE('',(#4275),#249,.T.);
#17392=ADVANCED_FACE('',(#4276),#250,.T.);
#17393=ADVANCED_FACE('',(#4277),#251,.T.);
#17394=ADVANCED_FACE('',(#4278),#3392,.T.);
#17395=ADVANCED_FACE('',(#4279),#252,.T.);
#17396=ADVANCED_FACE('',(#4280),#253,.T.);
#17397=ADVANCED_FACE('',(#4281),#3393,.T.);
#17398=ADVANCED_FACE('',(#4282),#254,.T.);
#17399=ADVANCED_FACE('',(#4283),#255,.T.);
#17400=ADVANCED_FACE('',(#4284),#3394,.F.);
#17401=ADVANCED_FACE('',(#4285),#256,.T.);
#17402=ADVANCED_FACE('',(#4286),#257,.T.);
#17403=ADVANCED_FACE('',(#4287),#3395,.T.);
#17404=ADVANCED_FACE('',(#4288),#16607,.T.);
#17405=ADVANCED_FACE('',(#4289),#3396,.T.);
#17406=ADVANCED_FACE('',(#4290),#16608,.T.);
#17407=ADVANCED_FACE('',(#4291),#3397,.T.);
#17408=ADVANCED_FACE('',(#4292),#16609,.T.);
#17409=ADVANCED_FACE('',(#4293,#3510),#16610,.F.);
#17410=ADVANCED_FACE('',(#4294),#16611,.T.);
#17411=ADVANCED_FACE('',(#4295,#3511),#16612,.F.);
#17412=ADVANCED_FACE('',(#4296),#3398,.T.);
#17413=ADVANCED_FACE('',(#4297,#3512),#16613,.F.);
#17414=ADVANCED_FACE('',(#4298),#3399,.F.);
#17415=ADVANCED_FACE('',(#4299),#258,.T.);
#17416=ADVANCED_FACE('',(#4300),#259,.T.);
#17417=ADVANCED_FACE('',(#4301),#151,.T.);
#17418=ADVANCED_FACE('',(#4302,#3513),#16614,.F.);
#17419=ADVANCED_FACE('',(#4303),#3400,.T.);
#17420=ADVANCED_FACE('',(#4304),#16615,.F.);
#17421=ADVANCED_FACE('',(#4305),#3401,.T.);
#17422=ADVANCED_FACE('',(#4306),#141,.T.);
#17423=ADVANCED_FACE('',(#4307),#16616,.F.);
#17424=ADVANCED_FACE('',(#4308),#16617,.F.);
#17425=ADVANCED_FACE('',(#4309),#16618,.F.);
#17426=ADVANCED_FACE('',(#4310),#16619,.F.);
#17427=ADVANCED_FACE('',(#4311),#16620,.F.);
#17428=ADVANCED_FACE('',(#4312),#16621,.F.);
#17429=ADVANCED_FACE('',(#4313),#16622,.F.);
#17430=ADVANCED_FACE('',(#4314),#16623,.F.);
#17431=ADVANCED_FACE('',(#4315),#16624,.F.);
#17432=ADVANCED_FACE('',(#4316),#16625,.F.);
#17433=ADVANCED_FACE('',(#4317),#16626,.F.);
#17434=ADVANCED_FACE('',(#4318),#16627,.F.);
#17435=ADVANCED_FACE('',(#4319),#16628,.F.);
#17436=ADVANCED_FACE('',(#4320),#16629,.F.);
#17437=ADVANCED_FACE('',(#4321),#16630,.F.);
#17438=ADVANCED_FACE('',(#4322),#16631,.F.);
#17439=ADVANCED_FACE('',(#4323),#16632,.F.);
#17440=ADVANCED_FACE('',(#4324),#16633,.F.);
#17441=ADVANCED_FACE('',(#4325),#16634,.F.);
#17442=ADVANCED_FACE('',(#4326),#16635,.F.);
#17443=ADVANCED_FACE('',(#4327),#16636,.T.);
#17444=ADVANCED_FACE('',(#4328),#260,.F.);
#17445=ADVANCED_FACE('',(#4329),#3402,.T.);
#17446=ADVANCED_FACE('',(#4330),#3403,.T.);
#17447=ADVANCED_FACE('',(#4331,#3514,#3515,#3516,#3517),#16637,.T.);
#17448=ADVANCED_FACE('',(#4332,#3518,#3519,#3520,#3521),#16638,.F.);
#17449=ADVANCED_FACE('',(#4333),#3404,.F.);
#17450=ADVANCED_FACE('',(#4334),#3405,.F.);
#17451=ADVANCED_FACE('',(#4335),#3406,.F.);
#17452=ADVANCED_FACE('',(#4336),#3407,.F.);
#17453=ADVANCED_FACE('',(#4337),#261,.T.);
#17454=ADVANCED_FACE('',(#4338),#262,.T.);
#17455=ADVANCED_FACE('',(#4339),#263,.T.);
#17456=ADVANCED_FACE('',(#4340),#264,.T.);
#17457=ADVANCED_FACE('',(#4341),#265,.T.);
#17458=ADVANCED_FACE('',(#4342),#266,.T.);
#17459=ADVANCED_FACE('',(#4343),#267,.T.);
#17460=ADVANCED_FACE('',(#4344),#268,.T.);
#17461=ADVANCED_FACE('',(#4345),#269,.T.);
#17462=ADVANCED_FACE('',(#4346),#270,.T.);
#17463=ADVANCED_FACE('',(#4347),#271,.T.);
#17464=ADVANCED_FACE('',(#4348),#272,.T.);
#17465=ADVANCED_FACE('',(#4349),#3408,.F.);
#17466=ADVANCED_FACE('',(#4350),#16639,.F.);
#17467=ADVANCED_FACE('',(#4351),#16640,.F.);
#17468=ADVANCED_FACE('',(#4352),#3409,.T.);
#17469=ADVANCED_FACE('',(#4353),#16641,.F.);
#17470=ADVANCED_FACE('',(#4354),#16642,.F.);
#17471=ADVANCED_FACE('',(#4355),#3410,.F.);
#17472=ADVANCED_FACE('',(#4356),#3411,.T.);
#17473=ADVANCED_FACE('',(#4357,#3522),#16643,.F.);
#17474=ADVANCED_FACE('',(#4358,#3523),#16644,.T.);
#17475=ADVANCED_FACE('',(#4359),#3412,.F.);
#17476=ADVANCED_FACE('',(#4360),#3413,.T.);
#17477=ADVANCED_FACE('',(#4361),#152,.T.);
#17478=ADVANCED_FACE('',(#4362),#153,.T.);
#17479=ADVANCED_FACE('',(#4363),#3414,.T.);
#17480=ADVANCED_FACE('',(#4364),#273,.T.);
#17481=ADVANCED_FACE('',(#4365),#3415,.T.);
#17482=ADVANCED_FACE('',(#4366),#3416,.T.);
#17483=ADVANCED_FACE('',(#4367),#3417,.T.);
#17484=ADVANCED_FACE('',(#4368),#154,.T.);
#17485=ADVANCED_FACE('',(#4369),#274,.T.);
#17486=ADVANCED_FACE('',(#4370),#275,.T.);
#17487=ADVANCED_FACE('',(#4371),#155,.T.);
#17488=ADVANCED_FACE('',(#4372),#276,.T.);
#17489=ADVANCED_FACE('',(#4373),#277,.T.);
#17490=ADVANCED_FACE('',(#4374),#3418,.T.);
#17491=ADVANCED_FACE('',(#4375),#3419,.T.);
#17492=ADVANCED_FACE('',(#4376),#3420,.T.);
#17493=ADVANCED_FACE('',(#4377),#278,.T.);
#17494=ADVANCED_FACE('',(#4378),#156,.T.);
#17495=ADVANCED_FACE('',(#4379),#157,.T.);
#17496=ADVANCED_FACE('',(#4380),#279,.T.);
#17497=ADVANCED_FACE('',(#4381),#280,.T.);
#17498=ADVANCED_FACE('',(#4382),#3421,.T.);
#17499=ADVANCED_FACE('',(#4383),#3422,.T.);
#17500=ADVANCED_FACE('',(#4384),#3423,.T.);
#17501=ADVANCED_FACE('',(#4385),#158,.T.);
#17502=ADVANCED_FACE('',(#4386),#159,.T.);
#17503=ADVANCED_FACE('',(#4387),#3424,.T.);
#17504=ADVANCED_FACE('',(#4388),#281,.T.);
#17505=ADVANCED_FACE('',(#4389),#282,.T.);
#17506=ADVANCED_FACE('',(#4390),#1707,.T.);
#17507=ADVANCED_FACE('',(#4391),#1708,.T.);
#17508=ADVANCED_FACE('',(#4392),#1709,.T.);
#17509=ADVANCED_FACE('',(#4393),#1710,.T.);
#17510=ADVANCED_FACE('',(#4394),#1711,.T.);
#17511=ADVANCED_FACE('',(#4395),#3425,.F.);
#17512=ADVANCED_FACE('',(#4396),#3426,.F.);
#17513=ADVANCED_FACE('',(#4397),#3427,.F.);
#17514=ADVANCED_FACE('',(#4398),#3428,.F.);
#17515=ADVANCED_FACE('',(#4399,#3524,#3525,#3526,#3527,#3528),#16645,.F.);
#17516=ADVANCED_FACE('',(#4400),#3429,.F.);
#17517=ADVANCED_FACE('',(#4401),#3430,.F.);
#17518=ADVANCED_FACE('',(#4402,#3529,#3530,#3531,#3532,#3533),#3431,.T.);
#17519=ADVANCED_FACE('',(#4403),#3432,.T.);
#17520=ADVANCED_FACE('',(#4404),#16646,.T.);
#17521=ADVANCED_FACE('',(#4405),#3433,.T.);
#17522=ADVANCED_FACE('',(#4406),#16647,.F.);
#17523=ADVANCED_FACE('',(#4407),#3434,.T.);
#17524=ADVANCED_FACE('',(#4408,#3534,#3535,#3536),#16648,.T.);
#17525=ADVANCED_FACE('',(#4409,#3537),#16649,.F.);
#17526=ADVANCED_FACE('',(#4410),#3435,.F.);
#17527=ADVANCED_FACE('',(#4411),#3436,.F.);
#17528=ADVANCED_FACE('',(#4412,#3538),#16650,.F.);
#17529=ADVANCED_FACE('',(#4413,#3539),#16651,.F.);
#17530=ADVANCED_FACE('',(#4414),#3437,.F.);
#17531=ADVANCED_FACE('',(#4415),#16652,.F.);
#17532=ADVANCED_FACE('',(#4416),#16653,.F.);
#17533=ADVANCED_FACE('',(#4417),#337,.T.);
#17534=ADVANCED_FACE('',(#4418),#338,.T.);
#17535=ADVANCED_FACE('',(#4419),#339,.T.);
#17536=ADVANCED_FACE('',(#4420),#340,.T.);
#17537=ADVANCED_FACE('',(#4421),#341,.T.);
#17538=ADVANCED_FACE('',(#4422),#16654,.T.);
#17539=ADVANCED_FACE('',(#4423),#160,.F.);
#17540=ADVANCED_FACE('',(#4424),#161,.F.);
#17541=ADVANCED_FACE('',(#4425),#162,.F.);
#17542=ADVANCED_FACE('',(#4426),#163,.F.);
#17543=ADVANCED_FACE('',(#4427),#164,.F.);
#17544=ADVANCED_FACE('',(#4428),#3438,.F.);
#17545=ADVANCED_FACE('',(#4429),#3439,.F.);
#17546=ADVANCED_FACE('',(#4430),#3440,.F.);
#17547=ADVANCED_FACE('',(#4431,#3540,#3541,#3542),#16655,.T.);
#17548=ADVANCED_FACE('',(#4432),#3441,.F.);
#17549=ADVANCED_FACE('',(#4433),#16656,.F.);
#17550=ADVANCED_FACE('',(#4434),#16657,.F.);
#17551=ADVANCED_FACE('',(#4435),#1712,.F.);
#17552=ADVANCED_FACE('',(#4436),#1713,.F.);
#17553=ADVANCED_FACE('',(#4437),#1714,.F.);
#17554=ADVANCED_FACE('',(#4438),#1715,.F.);
#17555=ADVANCED_FACE('',(#4439),#1716,.F.);
#17556=ADVANCED_FACE('',(#4440),#1717,.F.);
#17557=ADVANCED_FACE('',(#4441),#1718,.T.);
#17558=ADVANCED_FACE('',(#4442),#283,.F.);
#17559=ADVANCED_FACE('',(#4443),#1719,.T.);
#17560=ADVANCED_FACE('',(#4444),#284,.F.);
#17561=ADVANCED_FACE('',(#4445),#342,.T.);
#17562=ADVANCED_FACE('',(#4446),#285,.F.);
#17563=ADVANCED_FACE('',(#4447),#286,.F.);
#17564=ADVANCED_FACE('',(#4448),#1720,.T.);
#17565=ADVANCED_FACE('',(#4449),#287,.T.);
#17566=ADVANCED_FACE('',(#4450),#288,.T.);
#17567=ADVANCED_FACE('',(#4451),#3442,.F.);
#17568=ADVANCED_FACE('',(#4452),#289,.T.);
#17569=ADVANCED_FACE('',(#4453),#290,.F.);
#17570=ADVANCED_FACE('',(#4454),#3443,.T.);
#17571=ADVANCED_FACE('',(#4455),#291,.F.);
#17572=ADVANCED_FACE('',(#4456),#292,.F.);
#17573=ADVANCED_FACE('',(#4457),#293,.F.);
#17574=ADVANCED_FACE('',(#4458),#294,.F.);
#17575=ADVANCED_FACE('',(#4459),#295,.F.);
#17576=ADVANCED_FACE('',(#4460),#296,.F.);
#17577=ADVANCED_FACE('',(#4461),#3444,.T.);
#17578=ADVANCED_FACE('',(#4462),#3445,.F.);
#17579=ADVANCED_FACE('',(#4463),#297,.T.);
#17580=ADVANCED_FACE('',(#4464),#298,.T.);
#17581=ADVANCED_FACE('',(#4465),#299,.T.);
#17582=ADVANCED_FACE('',(#4466),#1721,.T.);
#17583=ADVANCED_FACE('',(#4467),#300,.T.);
#17584=ADVANCED_FACE('',(#4468),#3446,.T.);
#17585=ADVANCED_FACE('',(#4469),#301,.F.);
#17586=ADVANCED_FACE('',(#4470),#3447,.T.);
#17587=ADVANCED_FACE('',(#4471),#3448,.T.);
#17588=ADVANCED_FACE('',(#4472),#3449,.T.);
#17589=ADVANCED_FACE('',(#4473),#1722,.T.);
#17590=ADVANCED_FACE('',(#4474),#302,.T.);
#17591=ADVANCED_FACE('',(#4475),#303,.T.);
#17592=ADVANCED_FACE('',(#4476),#165,.T.);
#17593=ADVANCED_FACE('',(#4477),#3450,.F.);
#17594=ADVANCED_FACE('',(#4478),#304,.F.);
#17595=ADVANCED_FACE('',(#4479),#3451,.T.);
#17596=ADVANCED_FACE('',(#4480),#3452,.T.);
#17597=ADVANCED_FACE('',(#4481),#305,.F.);
#17598=ADVANCED_FACE('',(#4482),#1723,.T.);
#17599=ADVANCED_FACE('',(#4483),#306,.T.);
#17600=ADVANCED_FACE('',(#4484),#307,.T.);
#17601=ADVANCED_FACE('',(#4485),#3453,.F.);
#17602=ADVANCED_FACE('',(#4486),#3454,.T.);
#17603=ADVANCED_FACE('',(#4487),#3455,.T.);
#17604=ADVANCED_FACE('',(#4488),#3456,.T.);
#17605=ADVANCED_FACE('',(#4489),#1724,.T.);
#17606=ADVANCED_FACE('',(#4490),#166,.T.);
#17607=ADVANCED_FACE('',(#4491),#3457,.T.);
#17608=ADVANCED_FACE('',(#4492),#308,.F.);
#17609=ADVANCED_FACE('',(#4493),#309,.T.);
#17610=ADVANCED_FACE('',(#4494),#1725,.T.);
#17611=ADVANCED_FACE('',(#4495),#3458,.T.);
#17612=ADVANCED_FACE('',(#4496),#1726,.T.);
#17613=ADVANCED_FACE('',(#4497),#310,.T.);
#17614=ADVANCED_FACE('',(#4498),#311,.T.);
#17615=ADVANCED_FACE('',(#4499),#3459,.T.);
#17616=ADVANCED_FACE('',(#4500),#1727,.T.);
#17617=ADVANCED_FACE('',(#4501),#312,.T.);
#17618=ADVANCED_FACE('',(#4502),#1728,.T.);
#17619=ADVANCED_FACE('',(#4503),#3460,.T.);
#17620=ADVANCED_FACE('',(#4504),#3461,.T.);
#17621=ADVANCED_FACE('',(#4505),#313,.T.);
#17622=ADVANCED_FACE('',(#4506),#314,.T.);
#17623=ADVANCED_FACE('',(#4507),#315,.T.);
#17624=ADVANCED_FACE('',(#4508),#316,.T.);
#17625=ADVANCED_FACE('',(#4509),#317,.T.);
#17626=ADVANCED_FACE('',(#4510),#167,.F.);
#17627=ADVANCED_FACE('',(#4511),#318,.T.);
#17628=ADVANCED_FACE('',(#4512),#168,.T.);
#17629=ADVANCED_FACE('',(#4513),#169,.T.);
#17630=ADVANCED_FACE('',(#4514),#3462,.T.);
#17631=ADVANCED_FACE('',(#4515),#319,.F.);
#17632=ADVANCED_FACE('',(#4516),#3463,.T.);
#17633=ADVANCED_FACE('',(#4517),#1729,.T.);
#17634=ADVANCED_FACE('',(#4518),#320,.T.);
#17635=ADVANCED_FACE('',(#4519),#1730,.T.);
#17636=ADVANCED_FACE('',(#4520),#1731,.T.);
#17637=ADVANCED_FACE('',(#4521),#1732,.T.);
#17638=ADVANCED_FACE('',(#4522),#1733,.T.);
#17639=ADVANCED_FACE('',(#4523),#1734,.T.);
#17640=ADVANCED_FACE('',(#4524),#321,.F.);
#17641=ADVANCED_FACE('',(#4525),#1735,.F.);
#17642=ADVANCED_FACE('',(#4526),#1736,.F.);
#17643=ADVANCED_FACE('',(#4527),#3464,.F.);
#17644=ADVANCED_FACE('',(#4528),#3465,.F.);
#17645=ADVANCED_FACE('',(#4529),#1737,.F.);
#17646=ADVANCED_FACE('',(#4530),#1738,.F.);
#17647=ADVANCED_FACE('',(#4531),#3466,.T.);
#17648=ADVANCED_FACE('',(#4532),#3467,.T.);
#17649=ADVANCED_FACE('',(#4533),#1739,.F.);
#17650=ADVANCED_FACE('',(#4534),#1740,.F.);
#17651=ADVANCED_FACE('',(#4535),#3468,.F.);
#17652=ADVANCED_FACE('',(#4536),#3469,.F.);
#17653=ADVANCED_FACE('',(#4537),#3470,.F.);
#17654=ADVANCED_FACE('',(#4538),#1741,.F.);
#17655=ADVANCED_FACE('',(#4539),#1742,.F.);
#17656=ADVANCED_FACE('',(#4540),#3471,.T.);
#17657=ADVANCED_FACE('',(#4541),#3472,.F.);
#17658=ADVANCED_FACE('',(#4542),#3473,.F.);
#17659=ADVANCED_FACE('',(#4543),#3474,.F.);
#17660=ADVANCED_FACE('',(#4544),#3475,.F.);
#17661=ADVANCED_FACE('',(#4545),#322,.T.);
#17662=ADVANCED_FACE('',(#4546),#170,.T.);
#17663=ADVANCED_FACE('',(#4547),#16658,.F.);
#17664=ADVANCED_FACE('',(#4548),#3476,.T.);
#17665=ADVANCED_FACE('',(#4549,#3543),#16659,.F.);
#17666=CLOSED_SHELL('',(#16660,#16661,#16662,#16663,#16664,#16665,#16666,
#16667,#16668,#16669,#16670,#16671,#16672,#16673,#16674,#16675,#16676,#16677,
#16678,#16679,#16680,#16681,#16682,#16683,#16684,#16685,#16686,#16687,#16688,
#16689,#16690,#16691,#16692,#16693,#16694,#16695,#16696,#16697,#16698,#16699,
#16700,#16701,#16702,#16703,#16704,#16705,#16706,#16707,#16708,#16709,#16710,
#16711,#16712,#16713,#16714,#16715,#16716,#16717,#16718,#16719,#16720,#16721,
#16722,#16723,#16724,#16725,#16726,#16727,#16728,#16729,#16730,#16731,#16732,
#16733,#16734,#16735,#16736,#16737,#16738,#16739,#16740,#16741,#16742,#16743,
#16744,#16745,#16746,#16747,#16748,#16749,#16750,#16751,#16752,#16753,#16754,
#16755,#16756,#16757,#16758,#16759,#16760,#16761,#16762,#16763,#16764,#16765,
#16766,#16767,#16768,#16769,#16770,#16771,#16772,#16773,#16774,#16775,#16776,
#16777,#16778,#16779,#16780,#16781,#16782,#16783,#16784,#16785,#16786,#16787,
#16788,#16789,#16790,#16791,#16792,#16793,#16794,#16795,#16796,#16797,#16798,
#16799,#16800,#16801,#16802,#16803,#16804,#16805,#16806,#16807,#16808,#16809,
#16810,#16811,#16812,#16813,#16814,#16815,#16816,#16817,#16818,#16819,#16820,
#16821,#16822,#16823,#16824,#16825,#16826,#16827,#16828,#16829,#16830,#16831,
#16832,#16833,#16834,#16835,#16836,#16837,#16838,#16839,#16840,#16841,#16842,
#16843,#16844,#16845,#16846));
#17667=CLOSED_SHELL('',(#16847,#16848,#16849,#16850,#16851,#16852,#16853,
#16854,#16855,#16856,#16857,#16858,#16859,#16860,#16861,#16862,#16863,#16864,
#16865,#16866,#16867,#16868,#16869,#16870,#16871,#16872,#16873,#16874,#16875,
#16876,#16877,#16878,#16879,#16880,#16881,#16882,#16883,#16884,#16885,#16886,
#16887,#16888,#16889,#16890,#16891,#16892,#16893,#16894,#16895));
#17668=CLOSED_SHELL('',(#16896));
#17669=CLOSED_SHELL('',(#16897,#16898,#16899,#16900,#16901,#16902,#16903,
#16904,#16905,#16906,#16907,#16908,#16909,#16910,#16911,#16912,#16913,#16914,
#16915,#16916,#16917,#16918,#16919,#16920,#16921,#16922,#16923,#16924,#16925,
#16926,#16927,#16928,#16929,#16930,#16931,#16932,#16933,#16934,#16935,#16936,
#16937,#16938,#16939,#16940,#16941,#16942,#16943,#16944,#16945,#16946,#16947,
#16948,#16949,#16950,#16951,#16952,#16953,#16954,#16955,#16956,#16957,#16958,
#16959,#16960,#16961,#16962,#16963,#16964,#16965,#16966,#16967,#16968,#16969,
#16970,#16971,#16972,#16973,#16974,#16975,#16976,#16977,#16978,#16979,#16980,
#16981,#16982,#16983,#16984,#16985,#16986,#16987,#16988,#16989,#16990,#16991,
#16992,#16993,#16994,#16995,#16996,#16997,#16998,#16999,#17000,#17001,#17002,
#17003,#17004,#17005,#17006,#17007,#17008,#17009,#17010,#17011,#17012,#17013,
#17014,#17015,#17016,#17017,#17018,#17019,#17020,#17021,#17022,#17023,#17024,
#17025,#17026,#17027,#17028,#17029,#17030,#17031,#17032,#17033,#17034,#17035,
#17036,#17037,#17038,#17039,#17040,#17041,#17042,#17043,#17044,#17045,#17046,
#17047,#17048,#17049,#17050,#17051,#17052,#17053,#17054,#17055,#17056,#17057,
#17058,#17059,#17060,#17061,#17062,#17063,#17064,#17065,#17066,#17067,#17068,
#17069,#17070,#17071,#17072,#17073,#17074,#17075,#17076,#17077,#17078,#17079,
#17080,#17081,#17082,#17083,#17084,#17085,#17086,#17087,#17088,#17089,#17090,
#17091,#17092,#17093,#17094,#17095,#17096,#17097,#17098,#17099,#17100,#17101,
#17102,#17103,#17104,#17105,#17106,#17107,#17108,#17109,#17110,#17111,#17112,
#17113,#17114,#17115,#17116,#17117,#17118,#17119,#17120,#17121,#17122,#17123,
#17124,#17125,#17126,#17127,#17128,#17129,#17130,#17131,#17132,#17133,#17134,
#17135,#17136,#17137,#17138,#17139,#17140,#17141,#17142,#17143,#17144,#17145,
#17146,#17147,#17148,#17149,#17150,#17151,#17152,#17153,#17154,#17155,#17156,
#17157,#17158,#17159,#17160,#17161,#17162,#17163,#17164,#17165,#17166,#17167,
#17168,#17169,#17170,#17171,#17172,#17173,#17174,#17175,#17176,#17177,#17178,
#17179,#17180,#17181,#17182,#17183,#17184,#17185,#17186,#17187,#17188,#17189,
#17190,#17191,#17192,#17193,#17194,#17195,#17196,#17197,#17198,#17199,#17200,
#17201,#17202,#17203,#17204,#17205,#17206,#17207,#17208,#17209,#17210,#17211,
#17212,#17213,#17214,#17215,#17216,#17217,#17218,#17219,#17220,#17221,#17222,
#17223,#17224,#17225,#17226,#17227,#17228,#17229,#17230,#17231,#17232,#17233,
#17234,#17235,#17236,#17237,#17238,#17239,#17240,#17241,#17242,#17243,#17244,
#17245,#17246,#17247,#17248,#17249,#17250,#17251,#17252));
#17670=CLOSED_SHELL('',(#17253,#17254,#17255,#17256,#17257,#17258,#17259,
#17260,#17261,#17262,#17263,#17264,#17265,#17266,#17267,#17268,#17269,#17270,
#17271,#17272,#17273,#17274,#17275,#17276,#17277,#17278,#17279,#17280,#17281,
#17282,#17283,#17284));
#17671=CLOSED_SHELL('',(#17285,#17286,#17287,#17288,#17289,#17290,#17291,
#17292,#17293,#17294,#17295,#17296,#17297,#17298,#17299,#17300,#17301,#17302,
#17303,#17304,#17305,#17306,#17307,#17308,#17309,#17310,#17311,#17312,#17313,
#17314,#17315,#17316,#17317,#17318,#17319,#17320,#17321,#17322,#17323,#17324,
#17325,#17326,#17327,#17328,#17329,#17330,#17331,#17332,#17333,#17334,#17335,
#17336,#17337,#17338,#17339,#17340));
#17672=CLOSED_SHELL('',(#17341,#17342,#17343,#17344,#17345,#17346,#17347,
#17348,#17349,#17350,#17351,#17352,#17353,#17354,#17355,#17356,#17357,#17358,
#17359,#17360,#17361,#17362,#17363,#17364,#17365,#17366,#17367,#17368,#17369,
#17370,#17371,#17372,#17373,#17374,#17375,#17376,#17377,#17378,#17379,#17380,
#17381,#17382,#17383,#17384,#17385,#17386,#17387,#17388,#17389,#17390,#17391,
#17392,#17393,#17394,#17395,#17396,#17397,#17398,#17399,#17400,#17401,#17402));
#17673=CLOSED_SHELL('',(#17403,#17404,#17405,#17406,#17407,#17408,#17409,
#17410));
#17674=CLOSED_SHELL('',(#17411,#17412,#17413,#17414,#17415,#17416));
#17675=CLOSED_SHELL('',(#17417,#17418,#17419,#17420,#17421,#17422,#17423,
#17424,#17425,#17426,#17427,#17428,#17429,#17430,#17431,#17432,#17433,#17434,
#17435,#17436,#17437,#17438,#17439,#17440,#17441,#17442,#17443,#17444));
#17676=CLOSED_SHELL('',(#17445,#17446,#17447,#17448,#17449,#17450,#17451,
#17452,#17453,#17454,#17455,#17456,#17457,#17458,#17459,#17460,#17461,#17462,
#17463,#17464));
#17677=CLOSED_SHELL('',(#17465,#17466,#17467,#17468,#17469,#17470,#17471,
#17472,#17473,#17474,#17475,#17476,#17477,#17478,#17479,#17480,#17481,#17482,
#17483,#17484,#17485,#17486,#17487,#17488,#17489,#17490,#17491,#17492,#17493,
#17494,#17495,#17496,#17497,#17498,#17499,#17500,#17501,#17502,#17503,#17504,
#17505));
#17678=CLOSED_SHELL('',(#17506,#17507,#17508,#17509,#17510,#17511,#17512,
#17513,#17514,#17515,#17516,#17517,#17518,#17519,#17520,#17521,#17522,#17523,
#17524,#17525,#17526,#17527,#17528,#17529,#17530,#17531,#17532,#17533,#17534,
#17535,#17536,#17537,#17538,#17539,#17540,#17541,#17542,#17543,#17544,#17545,
#17546,#17547,#17548,#17549,#17550,#17551,#17552,#17553,#17554,#17555,#17556,
#17557,#17558,#17559,#17560,#17561,#17562,#17563,#17564,#17565,#17566,#17567,
#17568,#17569,#17570,#17571,#17572,#17573,#17574,#17575,#17576,#17577,#17578,
#17579,#17580,#17581,#17582,#17583,#17584,#17585,#17586,#17587,#17588,#17589,
#17590,#17591,#17592,#17593,#17594,#17595,#17596,#17597,#17598,#17599,#17600,
#17601,#17602,#17603,#17604,#17605,#17606,#17607,#17608,#17609,#17610,#17611,
#17612,#17613,#17614,#17615,#17616,#17617,#17618,#17619,#17620,#17621,#17622,
#17623,#17624,#17625,#17626,#17627,#17628,#17629,#17630,#17631,#17632,#17633,
#17634,#17635,#17636,#17637,#17638,#17639,#17640,#17641,#17642,#17643,#17644,
#17645,#17646,#17647,#17648,#17649,#17650,#17651,#17652,#17653,#17654,#17655,
#17656,#17657,#17658,#17659,#17660,#17661));
#17679=CLOSED_SHELL('',(#17662,#17663,#17664,#17665));
#17680=DERIVED_UNIT_ELEMENT(#17708,1.);
#17681=DERIVED_UNIT_ELEMENT(#54581,-3.);
#17682=DERIVED_UNIT_ELEMENT(#17708,1.);
#17683=DERIVED_UNIT_ELEMENT(#54581,-3.);
#17684=DERIVED_UNIT_ELEMENT(#17708,1.);
#17685=DERIVED_UNIT_ELEMENT(#54581,-3.);
#17686=DERIVED_UNIT_ELEMENT(#17708,1.);
#17687=DERIVED_UNIT_ELEMENT(#54581,-3.);
#17688=DERIVED_UNIT_ELEMENT(#17708,1.);
#17689=DERIVED_UNIT_ELEMENT(#54581,-3.);
#17690=DERIVED_UNIT_ELEMENT(#17708,1.);
#17691=DERIVED_UNIT_ELEMENT(#54581,-3.);
#17692=DERIVED_UNIT_ELEMENT(#17708,1.);
#17693=DERIVED_UNIT_ELEMENT(#54581,-3.);
#17694=DERIVED_UNIT_ELEMENT(#17708,1.);
#17695=DERIVED_UNIT_ELEMENT(#54581,-3.);
#17696=DERIVED_UNIT_ELEMENT(#17708,1.);
#17697=DERIVED_UNIT_ELEMENT(#54581,-3.);
#17698=DERIVED_UNIT_ELEMENT(#17708,1.);
#17699=DERIVED_UNIT_ELEMENT(#54581,-3.);
#17700=DERIVED_UNIT_ELEMENT(#17708,1.);
#17701=DERIVED_UNIT_ELEMENT(#54581,-3.);
#17702=DERIVED_UNIT_ELEMENT(#17708,1.);
#17703=DERIVED_UNIT_ELEMENT(#54581,-3.);
#17704=DERIVED_UNIT_ELEMENT(#17708,1.);
#17705=DERIVED_UNIT_ELEMENT(#54581,-3.);
#17706=DERIVED_UNIT_ELEMENT(#17708,1.);
#17707=DERIVED_UNIT_ELEMENT(#54581,-3.);
#17708=(
MASS_UNIT()
NAMED_UNIT(*)
SI_UNIT(.KILO.,.GRAM.)
);
#17709=DERIVED_UNIT((#17680,#17681));
#17710=DERIVED_UNIT((#17682,#17683));
#17711=DERIVED_UNIT((#17684,#17685));
#17712=DERIVED_UNIT((#17686,#17687));
#17713=DERIVED_UNIT((#17688,#17689));
#17714=DERIVED_UNIT((#17690,#17691));
#17715=DERIVED_UNIT((#17692,#17693));
#17716=DERIVED_UNIT((#17694,#17695));
#17717=DERIVED_UNIT((#17696,#17697));
#17718=DERIVED_UNIT((#17698,#17699));
#17719=DERIVED_UNIT((#17700,#17701));
#17720=DERIVED_UNIT((#17702,#17703));
#17721=DERIVED_UNIT((#17704,#17705));
#17722=DERIVED_UNIT((#17706,#17707));
#17723=MEASURE_REPRESENTATION_ITEM('density measure',
POSITIVE_RATIO_MEASURE(7850.),#17709);
#17724=MEASURE_REPRESENTATION_ITEM('density measure',
POSITIVE_RATIO_MEASURE(7850.),#17710);
#17725=MEASURE_REPRESENTATION_ITEM('density measure',
POSITIVE_RATIO_MEASURE(7850.),#17711);
#17726=MEASURE_REPRESENTATION_ITEM('density measure',
POSITIVE_RATIO_MEASURE(7850.),#17712);
#17727=MEASURE_REPRESENTATION_ITEM('density measure',
POSITIVE_RATIO_MEASURE(7850.),#17713);
#17728=MEASURE_REPRESENTATION_ITEM('density measure',
POSITIVE_RATIO_MEASURE(7850.),#17714);
#17729=MEASURE_REPRESENTATION_ITEM('density measure',
POSITIVE_RATIO_MEASURE(7850.),#17715);
#17730=MEASURE_REPRESENTATION_ITEM('density measure',
POSITIVE_RATIO_MEASURE(7850.),#17716);
#17731=MEASURE_REPRESENTATION_ITEM('density measure',
POSITIVE_RATIO_MEASURE(7850.),#17717);
#17732=MEASURE_REPRESENTATION_ITEM('density measure',
POSITIVE_RATIO_MEASURE(7850.),#17718);
#17733=MEASURE_REPRESENTATION_ITEM('density measure',
POSITIVE_RATIO_MEASURE(7850.),#17719);
#17734=MEASURE_REPRESENTATION_ITEM('density measure',
POSITIVE_RATIO_MEASURE(7850.),#17720);
#17735=MEASURE_REPRESENTATION_ITEM('density measure',
POSITIVE_RATIO_MEASURE(7850.),#17721);
#17736=MEASURE_REPRESENTATION_ITEM('density measure',
POSITIVE_RATIO_MEASURE(7850.),#17722);
#17737=PROPERTY_DEFINITION_REPRESENTATION(#17807,#17765);
#17738=PROPERTY_DEFINITION_REPRESENTATION(#17808,#17766);
#17739=PROPERTY_DEFINITION_REPRESENTATION(#17809,#17767);
#17740=PROPERTY_DEFINITION_REPRESENTATION(#17810,#17768);
#17741=PROPERTY_DEFINITION_REPRESENTATION(#17811,#17769);
#17742=PROPERTY_DEFINITION_REPRESENTATION(#17812,#17770);
#17743=PROPERTY_DEFINITION_REPRESENTATION(#17813,#17771);
#17744=PROPERTY_DEFINITION_REPRESENTATION(#17814,#17772);
#17745=PROPERTY_DEFINITION_REPRESENTATION(#17815,#17773);
#17746=PROPERTY_DEFINITION_REPRESENTATION(#17816,#17774);
#17747=PROPERTY_DEFINITION_REPRESENTATION(#17817,#17775);
#17748=PROPERTY_DEFINITION_REPRESENTATION(#17818,#17776);
#17749=PROPERTY_DEFINITION_REPRESENTATION(#17819,#17777);
#17750=PROPERTY_DEFINITION_REPRESENTATION(#17820,#17778);
#17751=PROPERTY_DEFINITION_REPRESENTATION(#17821,#17779);
#17752=PROPERTY_DEFINITION_REPRESENTATION(#17822,#17780);
#17753=PROPERTY_DEFINITION_REPRESENTATION(#17823,#17781);
#17754=PROPERTY_DEFINITION_REPRESENTATION(#17824,#17782);
#17755=PROPERTY_DEFINITION_REPRESENTATION(#17825,#17783);
#17756=PROPERTY_DEFINITION_REPRESENTATION(#17826,#17784);
#17757=PROPERTY_DEFINITION_REPRESENTATION(#17827,#17785);
#17758=PROPERTY_DEFINITION_REPRESENTATION(#17828,#17786);
#17759=PROPERTY_DEFINITION_REPRESENTATION(#17829,#17787);
#17760=PROPERTY_DEFINITION_REPRESENTATION(#17830,#17788);
#17761=PROPERTY_DEFINITION_REPRESENTATION(#17831,#17789);
#17762=PROPERTY_DEFINITION_REPRESENTATION(#17832,#17790);
#17763=PROPERTY_DEFINITION_REPRESENTATION(#17833,#17791);
#17764=PROPERTY_DEFINITION_REPRESENTATION(#17834,#17792);
#17765=REPRESENTATION('material name',(#17793),#54566);
#17766=REPRESENTATION('density',(#17723),#54566);
#17767=REPRESENTATION('material name',(#17794),#54567);
#17768=REPRESENTATION('density',(#17724),#54567);
#17769=REPRESENTATION('material name',(#17795),#54568);
#17770=REPRESENTATION('density',(#17725),#54568);
#17771=REPRESENTATION('material name',(#17796),#54569);
#17772=REPRESENTATION('density',(#17726),#54569);
#17773=REPRESENTATION('material name',(#17797),#54570);
#17774=REPRESENTATION('density',(#17727),#54570);
#17775=REPRESENTATION('material name',(#17798),#54571);
#17776=REPRESENTATION('density',(#17728),#54571);
#17777=REPRESENTATION('material name',(#17799),#54572);
#17778=REPRESENTATION('density',(#17729),#54572);
#17779=REPRESENTATION('material name',(#17800),#54573);
#17780=REPRESENTATION('density',(#17730),#54573);
#17781=REPRESENTATION('material name',(#17801),#54574);
#17782=REPRESENTATION('density',(#17731),#54574);
#17783=REPRESENTATION('material name',(#17802),#54575);
#17784=REPRESENTATION('density',(#17732),#54575);
#17785=REPRESENTATION('material name',(#17803),#54576);
#17786=REPRESENTATION('density',(#17733),#54576);
#17787=REPRESENTATION('material name',(#17804),#54577);
#17788=REPRESENTATION('density',(#17734),#54577);
#17789=REPRESENTATION('material name',(#17805),#54578);
#17790=REPRESENTATION('density',(#17735),#54578);
#17791=REPRESENTATION('material name',(#17806),#54579);
#17792=REPRESENTATION('density',(#17736),#54579);
#17793=DESCRIPTIVE_REPRESENTATION_ITEM('Steel','Steel');
#17794=DESCRIPTIVE_REPRESENTATION_ITEM('Steel','Steel');
#17795=DESCRIPTIVE_REPRESENTATION_ITEM('Steel','Steel');
#17796=DESCRIPTIVE_REPRESENTATION_ITEM('Steel','Steel');
#17797=DESCRIPTIVE_REPRESENTATION_ITEM('Steel','Steel');
#17798=DESCRIPTIVE_REPRESENTATION_ITEM('Steel','Steel');
#17799=DESCRIPTIVE_REPRESENTATION_ITEM('Steel','Steel');
#17800=DESCRIPTIVE_REPRESENTATION_ITEM('Steel','Steel');
#17801=DESCRIPTIVE_REPRESENTATION_ITEM('Steel','Steel');
#17802=DESCRIPTIVE_REPRESENTATION_ITEM('Steel','Steel');
#17803=DESCRIPTIVE_REPRESENTATION_ITEM('Steel','Steel');
#17804=DESCRIPTIVE_REPRESENTATION_ITEM('Steel','Steel');
#17805=DESCRIPTIVE_REPRESENTATION_ITEM('Steel','Steel');
#17806=DESCRIPTIVE_REPRESENTATION_ITEM('Steel','Steel');
#17807=PROPERTY_DEFINITION('material property','material name',#54646);
#17808=PROPERTY_DEFINITION('material property','density of part',#54646);
#17809=PROPERTY_DEFINITION('material property','material name',#54647);
#17810=PROPERTY_DEFINITION('material property','density of part',#54647);
#17811=PROPERTY_DEFINITION('material property','material name',#54648);
#17812=PROPERTY_DEFINITION('material property','density of part',#54648);
#17813=PROPERTY_DEFINITION('material property','material name',#54649);
#17814=PROPERTY_DEFINITION('material property','density of part',#54649);
#17815=PROPERTY_DEFINITION('material property','material name',#54650);
#17816=PROPERTY_DEFINITION('material property','density of part',#54650);
#17817=PROPERTY_DEFINITION('material property','material name',#54651);
#17818=PROPERTY_DEFINITION('material property','density of part',#54651);
#17819=PROPERTY_DEFINITION('material property','material name',#54652);
#17820=PROPERTY_DEFINITION('material property','density of part',#54652);
#17821=PROPERTY_DEFINITION('material property','material name',#54653);
#17822=PROPERTY_DEFINITION('material property','density of part',#54653);
#17823=PROPERTY_DEFINITION('material property','material name',#54654);
#17824=PROPERTY_DEFINITION('material property','density of part',#54654);
#17825=PROPERTY_DEFINITION('material property','material name',#54655);
#17826=PROPERTY_DEFINITION('material property','density of part',#54655);
#17827=PROPERTY_DEFINITION('material property','material name',#54656);
#17828=PROPERTY_DEFINITION('material property','density of part',#54656);
#17829=PROPERTY_DEFINITION('material property','material name',#54657);
#17830=PROPERTY_DEFINITION('material property','density of part',#54657);
#17831=PROPERTY_DEFINITION('material property','material name',#54658);
#17832=PROPERTY_DEFINITION('material property','density of part',#54658);
#17833=PROPERTY_DEFINITION('material property','material name',#54659);
#17834=PROPERTY_DEFINITION('material property','density of part',#54659);
#17835=AXIS2_PLACEMENT_3D('',#23726,#19601,#19602);
#17836=AXIS2_PLACEMENT_3D('',#23727,#19603,#19604);
#17837=AXIS2_PLACEMENT_3D('',#23728,#19605,#19606);
#17838=AXIS2_PLACEMENT_3D('',#23731,#19607,#19608);
#17839=AXIS2_PLACEMENT_3D('',#23733,#19609,#19610);
#17840=AXIS2_PLACEMENT_3D('',#23735,#19611,#19612);
#17841=AXIS2_PLACEMENT_3D('',#23737,#19613,#19614);
#17842=AXIS2_PLACEMENT_3D('',#23739,#19615,#19616);
#17843=AXIS2_PLACEMENT_3D('',#23741,#19617,#19618);
#17844=AXIS2_PLACEMENT_3D('',#23743,#19619,#19620);
#17845=AXIS2_PLACEMENT_3D('',#23745,#19621,#19622);
#17846=AXIS2_PLACEMENT_3D('',#23747,#19623,#19624);
#17847=AXIS2_PLACEMENT_3D('',#23749,#19625,#19626);
#17848=AXIS2_PLACEMENT_3D('',#23751,#19627,#19628);
#17849=AXIS2_PLACEMENT_3D('',#23753,#19629,#19630);
#17850=AXIS2_PLACEMENT_3D('',#23755,#19631,#19632);
#17851=AXIS2_PLACEMENT_3D('',#23757,#19633,#19634);
#17852=AXIS2_PLACEMENT_3D('',#23759,#19635,#19636);
#17853=AXIS2_PLACEMENT_3D('',#23761,#19637,#19638);
#17854=AXIS2_PLACEMENT_3D('',#23763,#19639,#19640);
#17855=AXIS2_PLACEMENT_3D('',#23765,#19641,#19642);
#17856=AXIS2_PLACEMENT_3D('',#23767,#19643,#19644);
#17857=AXIS2_PLACEMENT_3D('',#23769,#19645,#19646);
#17858=AXIS2_PLACEMENT_3D('',#23771,#19647,#19648);
#17859=AXIS2_PLACEMENT_3D('',#23773,#19649,#19650);
#17860=AXIS2_PLACEMENT_3D('',#23775,#19651,#19652);
#17861=AXIS2_PLACEMENT_3D('',#23777,#19653,#19654);
#17862=AXIS2_PLACEMENT_3D('',#23779,#19655,#19656);
#17863=AXIS2_PLACEMENT_3D('',#23781,#19657,#19658);
#17864=AXIS2_PLACEMENT_3D('',#23783,#19659,#19660);
#17865=AXIS2_PLACEMENT_3D('',#23785,#19661,#19662);
#17866=AXIS2_PLACEMENT_3D('',#23787,#19663,#19664);
#17867=AXIS2_PLACEMENT_3D('',#23789,#19665,#19666);
#17868=AXIS2_PLACEMENT_3D('',#23791,#19667,#19668);
#17869=AXIS2_PLACEMENT_3D('',#23793,#19669,#19670);
#17870=AXIS2_PLACEMENT_3D('',#23795,#19671,#19672);
#17871=AXIS2_PLACEMENT_3D('',#23797,#19673,#19674);
#17872=AXIS2_PLACEMENT_3D('',#23799,#19675,#19676);
#17873=AXIS2_PLACEMENT_3D('',#23801,#19677,#19678);
#17874=AXIS2_PLACEMENT_3D('',#23803,#19679,#19680);
#17875=AXIS2_PLACEMENT_3D('',#23805,#19681,#19682);
#17876=AXIS2_PLACEMENT_3D('',#23807,#19683,#19684);
#17877=AXIS2_PLACEMENT_3D('',#23809,#19685,#19686);
#17878=AXIS2_PLACEMENT_3D('',#23811,#19687,#19688);
#17879=AXIS2_PLACEMENT_3D('',#23813,#19689,#19690);
#17880=AXIS2_PLACEMENT_3D('',#23815,#19691,#19692);
#17881=AXIS2_PLACEMENT_3D('',#23817,#19693,#19694);
#17882=AXIS2_PLACEMENT_3D('',#23819,#19695,#19696);
#17883=AXIS2_PLACEMENT_3D('',#23821,#19697,#19698);
#17884=AXIS2_PLACEMENT_3D('',#23823,#19699,#19700);
#17885=AXIS2_PLACEMENT_3D('',#23825,#19701,#19702);
#17886=AXIS2_PLACEMENT_3D('',#23827,#19703,#19704);
#17887=AXIS2_PLACEMENT_3D('',#23829,#19705,#19706);
#17888=AXIS2_PLACEMENT_3D('',#23831,#19707,#19708);
#17889=AXIS2_PLACEMENT_3D('',#23833,#19709,#19710);
#17890=AXIS2_PLACEMENT_3D('',#23835,#19711,#19712);
#17891=AXIS2_PLACEMENT_3D('',#23837,#19713,#19714);
#17892=AXIS2_PLACEMENT_3D('',#23839,#19715,#19716);
#17893=AXIS2_PLACEMENT_3D('',#23841,#19717,#19718);
#17894=AXIS2_PLACEMENT_3D('',#23843,#19719,#19720);
#17895=AXIS2_PLACEMENT_3D('',#23845,#19721,#19722);
#17896=AXIS2_PLACEMENT_3D('',#23847,#19723,#19724);
#17897=AXIS2_PLACEMENT_3D('',#23849,#19725,#19726);
#17898=AXIS2_PLACEMENT_3D('',#23851,#19727,#19728);
#17899=AXIS2_PLACEMENT_3D('',#23853,#19729,#19730);
#17900=AXIS2_PLACEMENT_3D('',#23855,#19731,#19732);
#17901=AXIS2_PLACEMENT_3D('',#23857,#19733,#19734);
#17902=AXIS2_PLACEMENT_3D('',#23859,#19735,#19736);
#17903=AXIS2_PLACEMENT_3D('',#23861,#19737,#19738);
#17904=AXIS2_PLACEMENT_3D('',#23863,#19739,#19740);
#17905=AXIS2_PLACEMENT_3D('',#23865,#19741,#19742);
#17906=AXIS2_PLACEMENT_3D('',#23867,#19743,#19744);
#17907=AXIS2_PLACEMENT_3D('',#23869,#19745,#19746);
#17908=AXIS2_PLACEMENT_3D('',#23871,#19747,#19748);
#17909=AXIS2_PLACEMENT_3D('',#23873,#19749,#19750);
#17910=AXIS2_PLACEMENT_3D('',#23875,#19751,#19752);
#17911=AXIS2_PLACEMENT_3D('',#23877,#19753,#19754);
#17912=AXIS2_PLACEMENT_3D('',#23879,#19755,#19756);
#17913=AXIS2_PLACEMENT_3D('',#23881,#19757,#19758);
#17914=AXIS2_PLACEMENT_3D('',#23883,#19759,#19760);
#17915=AXIS2_PLACEMENT_3D('',#23885,#19761,#19762);
#17916=AXIS2_PLACEMENT_3D('',#23887,#19763,#19764);
#17917=AXIS2_PLACEMENT_3D('',#23889,#19765,#19766);
#17918=AXIS2_PLACEMENT_3D('',#23891,#19767,#19768);
#17919=AXIS2_PLACEMENT_3D('',#23893,#19769,#19770);
#17920=AXIS2_PLACEMENT_3D('',#23895,#19771,#19772);
#17921=AXIS2_PLACEMENT_3D('',#23897,#19773,#19774);
#17922=AXIS2_PLACEMENT_3D('',#23899,#19775,#19776);
#17923=AXIS2_PLACEMENT_3D('',#23901,#19777,#19778);
#17924=AXIS2_PLACEMENT_3D('',#23903,#19779,#19780);
#17925=AXIS2_PLACEMENT_3D('',#23905,#19781,#19782);
#17926=AXIS2_PLACEMENT_3D('',#23907,#19783,#19784);
#17927=AXIS2_PLACEMENT_3D('',#23909,#19785,#19786);
#17928=AXIS2_PLACEMENT_3D('',#23911,#19787,#19788);
#17929=AXIS2_PLACEMENT_3D('',#23913,#19789,#19790);
#17930=AXIS2_PLACEMENT_3D('',#23915,#19791,#19792);
#17931=AXIS2_PLACEMENT_3D('',#23917,#19793,#19794);
#17932=AXIS2_PLACEMENT_3D('',#23919,#19795,#19796);
#17933=AXIS2_PLACEMENT_3D('',#23921,#19797,#19798);
#17934=AXIS2_PLACEMENT_3D('',#23923,#19799,#19800);
#17935=AXIS2_PLACEMENT_3D('',#23925,#19801,#19802);
#17936=AXIS2_PLACEMENT_3D('',#23927,#19803,#19804);
#17937=AXIS2_PLACEMENT_3D('',#23929,#19805,#19806);
#17938=AXIS2_PLACEMENT_3D('',#23931,#19807,#19808);
#17939=AXIS2_PLACEMENT_3D('',#23933,#19809,#19810);
#17940=AXIS2_PLACEMENT_3D('',#23935,#19811,#19812);
#17941=AXIS2_PLACEMENT_3D('',#23937,#19813,#19814);
#17942=AXIS2_PLACEMENT_3D('',#23939,#19815,#19816);
#17943=AXIS2_PLACEMENT_3D('',#23941,#19817,#19818);
#17944=AXIS2_PLACEMENT_3D('',#23943,#19819,#19820);
#17945=AXIS2_PLACEMENT_3D('',#23945,#19821,#19822);
#17946=AXIS2_PLACEMENT_3D('',#23947,#19823,#19824);
#17947=AXIS2_PLACEMENT_3D('',#23949,#19825,#19826);
#17948=AXIS2_PLACEMENT_3D('',#23951,#19827,#19828);
#17949=AXIS2_PLACEMENT_3D('',#23953,#19829,#19830);
#17950=AXIS2_PLACEMENT_3D('',#23955,#19831,#19832);
#17951=AXIS2_PLACEMENT_3D('',#23957,#19833,#19834);
#17952=AXIS2_PLACEMENT_3D('',#23959,#19835,#19836);
#17953=AXIS2_PLACEMENT_3D('',#23961,#19837,#19838);
#17954=AXIS2_PLACEMENT_3D('',#23963,#19839,#19840);
#17955=AXIS2_PLACEMENT_3D('',#23965,#19841,#19842);
#17956=AXIS2_PLACEMENT_3D('',#23967,#19843,#19844);
#17957=AXIS2_PLACEMENT_3D('',#23969,#19845,#19846);
#17958=AXIS2_PLACEMENT_3D('',#23971,#19847,#19848);
#17959=AXIS2_PLACEMENT_3D('',#23973,#19849,#19850);
#17960=AXIS2_PLACEMENT_3D('',#23975,#19851,#19852);
#17961=AXIS2_PLACEMENT_3D('',#23977,#19853,#19854);
#17962=AXIS2_PLACEMENT_3D('',#23979,#19855,#19856);
#17963=AXIS2_PLACEMENT_3D('',#23981,#19857,#19858);
#17964=AXIS2_PLACEMENT_3D('',#23983,#19859,#19860);
#17965=AXIS2_PLACEMENT_3D('',#23985,#19861,#19862);
#17966=AXIS2_PLACEMENT_3D('',#23987,#19863,#19864);
#17967=AXIS2_PLACEMENT_3D('',#23989,#19865,#19866);
#17968=AXIS2_PLACEMENT_3D('',#23991,#19867,#19868);
#17969=AXIS2_PLACEMENT_3D('',#23993,#19869,#19870);
#17970=AXIS2_PLACEMENT_3D('',#23995,#19871,#19872);
#17971=AXIS2_PLACEMENT_3D('',#23997,#19873,#19874);
#17972=AXIS2_PLACEMENT_3D('',#23999,#19875,#19876);
#17973=AXIS2_PLACEMENT_3D('',#24001,#19877,#19878);
#17974=AXIS2_PLACEMENT_3D('',#24003,#19879,#19880);
#17975=AXIS2_PLACEMENT_3D('',#24005,#19881,#19882);
#17976=AXIS2_PLACEMENT_3D('',#24007,#19883,#19884);
#17977=AXIS2_PLACEMENT_3D('',#24009,#19885,#19886);
#17978=AXIS2_PLACEMENT_3D('',#24011,#19887,#19888);
#17979=AXIS2_PLACEMENT_3D('',#24013,#19889,#19890);
#17980=AXIS2_PLACEMENT_3D('',#24015,#19891,#19892);
#17981=AXIS2_PLACEMENT_3D('',#24017,#19893,#19894);
#17982=AXIS2_PLACEMENT_3D('',#24019,#19895,#19896);
#17983=AXIS2_PLACEMENT_3D('',#24021,#19897,#19898);
#17984=AXIS2_PLACEMENT_3D('',#24023,#19899,#19900);
#17985=AXIS2_PLACEMENT_3D('',#24025,#19901,#19902);
#17986=AXIS2_PLACEMENT_3D('',#24027,#19903,#19904);
#17987=AXIS2_PLACEMENT_3D('',#24029,#19905,#19906);
#17988=AXIS2_PLACEMENT_3D('',#24031,#19907,#19908);
#17989=AXIS2_PLACEMENT_3D('',#24033,#19909,#19910);
#17990=AXIS2_PLACEMENT_3D('',#24035,#19911,#19912);
#17991=AXIS2_PLACEMENT_3D('',#24037,#19913,#19914);
#17992=AXIS2_PLACEMENT_3D('',#24039,#19915,#19916);
#17993=AXIS2_PLACEMENT_3D('',#24041,#19917,#19918);
#17994=AXIS2_PLACEMENT_3D('',#24043,#19919,#19920);
#17995=AXIS2_PLACEMENT_3D('',#24045,#19921,#19922);
#17996=AXIS2_PLACEMENT_3D('',#24047,#19923,#19924);
#17997=AXIS2_PLACEMENT_3D('',#24049,#19925,#19926);
#17998=AXIS2_PLACEMENT_3D('',#24051,#19927,#19928);
#17999=AXIS2_PLACEMENT_3D('',#24053,#19929,#19930);
#18000=AXIS2_PLACEMENT_3D('',#24055,#19931,#19932);
#18001=AXIS2_PLACEMENT_3D('',#24057,#19933,#19934);
#18002=AXIS2_PLACEMENT_3D('',#24059,#19935,#19936);
#18003=AXIS2_PLACEMENT_3D('',#24061,#19937,#19938);
#18004=AXIS2_PLACEMENT_3D('',#24063,#19939,#19940);
#18005=AXIS2_PLACEMENT_3D('',#24065,#19941,#19942);
#18006=AXIS2_PLACEMENT_3D('',#24067,#19943,#19944);
#18007=AXIS2_PLACEMENT_3D('',#24069,#19945,#19946);
#18008=AXIS2_PLACEMENT_3D('',#24071,#19947,#19948);
#18009=AXIS2_PLACEMENT_3D('',#24073,#19949,#19950);
#18010=AXIS2_PLACEMENT_3D('',#24075,#19951,#19952);
#18011=AXIS2_PLACEMENT_3D('',#24077,#19953,#19954);
#18012=AXIS2_PLACEMENT_3D('',#24079,#19955,#19956);
#18013=AXIS2_PLACEMENT_3D('',#24081,#19957,#19958);
#18014=AXIS2_PLACEMENT_3D('',#24083,#19959,#19960);
#18015=AXIS2_PLACEMENT_3D('',#24085,#19961,#19962);
#18016=AXIS2_PLACEMENT_3D('',#24087,#19963,#19964);
#18017=AXIS2_PLACEMENT_3D('',#24089,#19965,#19966);
#18018=AXIS2_PLACEMENT_3D('',#24091,#19967,#19968);
#18019=AXIS2_PLACEMENT_3D('',#24093,#19969,#19970);
#18020=AXIS2_PLACEMENT_3D('',#24095,#19971,#19972);
#18021=AXIS2_PLACEMENT_3D('',#24096,#19973,#19974);
#18022=AXIS2_PLACEMENT_3D('',#24098,#19975,#19976);
#18023=AXIS2_PLACEMENT_3D('',#24099,#19977,#19978);
#18024=AXIS2_PLACEMENT_3D('',#24104,#19981,#19982);
#18025=AXIS2_PLACEMENT_3D('',#24105,#19983,#19984);
#18026=AXIS2_PLACEMENT_3D('',#24109,#19986,#19987);
#18027=AXIS2_PLACEMENT_3D('',#24111,#19989,#19990);
#18028=AXIS2_PLACEMENT_3D('',#24116,#19993,#19994);
#18029=AXIS2_PLACEMENT_3D('',#24117,#19995,#19996);
#18030=AXIS2_PLACEMENT_3D('',#24122,#19999,#20000);
#18031=AXIS2_PLACEMENT_3D('',#24123,#20001,#20002);
#18032=AXIS2_PLACEMENT_3D('',#24128,#20005,#20006);
#18033=AXIS2_PLACEMENT_3D('',#24129,#20007,#20008);
#18034=AXIS2_PLACEMENT_3D('',#24133,#20010,#20011);
#18035=AXIS2_PLACEMENT_3D('',#24135,#20013,#20014);
#18036=AXIS2_PLACEMENT_3D('',#24139,#20016,#20017);
#18037=AXIS2_PLACEMENT_3D('',#24141,#20019,#20020);
#18038=AXIS2_PLACEMENT_3D('',#24146,#20023,#20024);
#18039=AXIS2_PLACEMENT_3D('',#24147,#20025,#20026);
#18040=AXIS2_PLACEMENT_3D('',#24151,#20028,#20029);
#18041=AXIS2_PLACEMENT_3D('',#24153,#20031,#20032);
#18042=AXIS2_PLACEMENT_3D('',#24158,#20035,#20036);
#18043=AXIS2_PLACEMENT_3D('',#24159,#20037,#20038);
#18044=AXIS2_PLACEMENT_3D('',#24164,#20041,#20042);
#18045=AXIS2_PLACEMENT_3D('',#24165,#20043,#20044);
#18046=AXIS2_PLACEMENT_3D('',#24170,#20047,#20048);
#18047=AXIS2_PLACEMENT_3D('',#24171,#20049,#20050);
#18048=AXIS2_PLACEMENT_3D('',#24176,#20053,#20054);
#18049=AXIS2_PLACEMENT_3D('',#24177,#20055,#20056);
#18050=AXIS2_PLACEMENT_3D('',#24181,#20058,#20059);
#18051=AXIS2_PLACEMENT_3D('',#24183,#20061,#20062);
#18052=AXIS2_PLACEMENT_3D('',#24188,#20065,#20066);
#18053=AXIS2_PLACEMENT_3D('',#24189,#20067,#20068);
#18054=AXIS2_PLACEMENT_3D('',#24194,#20071,#20072);
#18055=AXIS2_PLACEMENT_3D('',#24195,#20073,#20074);
#18056=AXIS2_PLACEMENT_3D('',#24200,#20077,#20078);
#18057=AXIS2_PLACEMENT_3D('',#24201,#20079,#20080);
#18058=AXIS2_PLACEMENT_3D('',#24205,#20082,#20083);
#18059=AXIS2_PLACEMENT_3D('',#24207,#20085,#20086);
#18060=AXIS2_PLACEMENT_3D('',#24211,#20088,#20089);
#18061=AXIS2_PLACEMENT_3D('',#24213,#20091,#20092);
#18062=AXIS2_PLACEMENT_3D('',#24218,#20095,#20096);
#18063=AXIS2_PLACEMENT_3D('',#24219,#20097,#20098);
#18064=AXIS2_PLACEMENT_3D('',#24223,#20100,#20101);
#18065=AXIS2_PLACEMENT_3D('',#24225,#20103,#20104);
#18066=AXIS2_PLACEMENT_3D('',#24230,#20107,#20108);
#18067=AXIS2_PLACEMENT_3D('',#24231,#20109,#20110);
#18068=AXIS2_PLACEMENT_3D('',#24236,#20113,#20114);
#18069=AXIS2_PLACEMENT_3D('',#24237,#20115,#20116);
#18070=AXIS2_PLACEMENT_3D('',#24242,#20119,#20120);
#18071=AXIS2_PLACEMENT_3D('',#24243,#20121,#20122);
#18072=AXIS2_PLACEMENT_3D('',#24247,#20124,#20125);
#18073=AXIS2_PLACEMENT_3D('',#24249,#20127,#20128);
#18074=AXIS2_PLACEMENT_3D('',#24254,#20131,#20132);
#18075=AXIS2_PLACEMENT_3D('',#24255,#20133,#20134);
#18076=AXIS2_PLACEMENT_3D('',#24260,#20137,#20138);
#18077=AXIS2_PLACEMENT_3D('',#24261,#20139,#20140);
#18078=AXIS2_PLACEMENT_3D('',#24266,#20143,#20144);
#18079=AXIS2_PLACEMENT_3D('',#24267,#20145,#20146);
#18080=AXIS2_PLACEMENT_3D('',#24271,#20148,#20149);
#18081=AXIS2_PLACEMENT_3D('',#24273,#20151,#20152);
#18082=AXIS2_PLACEMENT_3D('',#24278,#20155,#20156);
#18083=AXIS2_PLACEMENT_3D('',#24279,#20157,#20158);
#18084=AXIS2_PLACEMENT_3D('',#24284,#20161,#20162);
#18085=AXIS2_PLACEMENT_3D('',#24285,#20163,#20164);
#18086=AXIS2_PLACEMENT_3D('',#24289,#20166,#20167);
#18087=AXIS2_PLACEMENT_3D('',#24291,#20169,#20170);
#18088=AXIS2_PLACEMENT_3D('',#24296,#20173,#20174);
#18089=AXIS2_PLACEMENT_3D('',#24297,#20175,#20176);
#18090=AXIS2_PLACEMENT_3D('',#24302,#20179,#20180);
#18091=AXIS2_PLACEMENT_3D('',#24303,#20181,#20182);
#18092=AXIS2_PLACEMENT_3D('',#24308,#20185,#20186);
#18093=AXIS2_PLACEMENT_3D('',#24309,#20187,#20188);
#18094=AXIS2_PLACEMENT_3D('',#24313,#20190,#20191);
#18095=AXIS2_PLACEMENT_3D('',#24315,#20193,#20194);
#18096=AXIS2_PLACEMENT_3D('',#24320,#20197,#20198);
#18097=AXIS2_PLACEMENT_3D('',#24321,#20199,#20200);
#18098=AXIS2_PLACEMENT_3D('',#24326,#20203,#20204);
#18099=AXIS2_PLACEMENT_3D('',#24327,#20205,#20206);
#18100=AXIS2_PLACEMENT_3D('',#24332,#20209,#20210);
#18101=AXIS2_PLACEMENT_3D('',#24333,#20211,#20212);
#18102=AXIS2_PLACEMENT_3D('',#24337,#20214,#20215);
#18103=AXIS2_PLACEMENT_3D('',#24339,#20217,#20218);
#18104=AXIS2_PLACEMENT_3D('',#24344,#20221,#20222);
#18105=AXIS2_PLACEMENT_3D('',#24345,#20223,#20224);
#18106=AXIS2_PLACEMENT_3D('',#24350,#20227,#20228);
#18107=AXIS2_PLACEMENT_3D('',#24351,#20229,#20230);
#18108=AXIS2_PLACEMENT_3D('',#24355,#20232,#20233);
#18109=AXIS2_PLACEMENT_3D('',#24357,#20235,#20236);
#18110=AXIS2_PLACEMENT_3D('',#24362,#20239,#20240);
#18111=AXIS2_PLACEMENT_3D('',#24363,#20241,#20242);
#18112=AXIS2_PLACEMENT_3D('',#24368,#20245,#20246);
#18113=AXIS2_PLACEMENT_3D('',#24369,#20247,#20248);
#18114=AXIS2_PLACEMENT_3D('',#24371,#20249,#20250);
#18115=AXIS2_PLACEMENT_3D('',#24373,#20251,#20252);
#18116=AXIS2_PLACEMENT_3D('',#24375,#20253,#20254);
#18117=AXIS2_PLACEMENT_3D('',#24376,#20255,#20256);
#18118=AXIS2_PLACEMENT_3D('',#24378,#20257,#20258);
#18119=AXIS2_PLACEMENT_3D('',#24380,#20259,#20260);
#18120=AXIS2_PLACEMENT_3D('',#24381,#20261,#20262);
#18121=AXIS2_PLACEMENT_3D('',#24383,#20263,#20264);
#18122=AXIS2_PLACEMENT_3D('',#24385,#20265,#20266);
#18123=AXIS2_PLACEMENT_3D('',#24386,#20267,#20268);
#18124=AXIS2_PLACEMENT_3D('',#24388,#20269,#20270);
#18125=AXIS2_PLACEMENT_3D('',#24390,#20271,#20272);
#18126=AXIS2_PLACEMENT_3D('',#24391,#20273,#20274);
#18127=AXIS2_PLACEMENT_3D('',#24393,#20275,#20276);
#18128=AXIS2_PLACEMENT_3D('',#24395,#20277,#20278);
#18129=AXIS2_PLACEMENT_3D('',#24396,#20279,#20280);
#18130=AXIS2_PLACEMENT_3D('',#24398,#20281,#20282);
#18131=AXIS2_PLACEMENT_3D('',#24400,#20283,#20284);
#18132=AXIS2_PLACEMENT_3D('',#24401,#20285,#20286);
#18133=AXIS2_PLACEMENT_3D('',#24403,#20287,#20288);
#18134=AXIS2_PLACEMENT_3D('',#24405,#20289,#20290);
#18135=AXIS2_PLACEMENT_3D('',#24406,#20291,#20292);
#18136=AXIS2_PLACEMENT_3D('',#24408,#20293,#20294);
#18137=AXIS2_PLACEMENT_3D('',#24410,#20295,#20296);
#18138=AXIS2_PLACEMENT_3D('',#24411,#20297,#20298);
#18139=AXIS2_PLACEMENT_3D('',#24413,#20299,#20300);
#18140=AXIS2_PLACEMENT_3D('',#24415,#20301,#20302);
#18141=AXIS2_PLACEMENT_3D('',#24416,#20303,#20304);
#18142=AXIS2_PLACEMENT_3D('',#24418,#20305,#20306);
#18143=AXIS2_PLACEMENT_3D('',#24420,#20307,#20308);
#18144=AXIS2_PLACEMENT_3D('',#24421,#20309,#20310);
#18145=AXIS2_PLACEMENT_3D('',#24423,#20311,#20312);
#18146=AXIS2_PLACEMENT_3D('',#24425,#20313,#20314);
#18147=AXIS2_PLACEMENT_3D('',#24427,#20315,#20316);
#18148=AXIS2_PLACEMENT_3D('',#24429,#20317,#20318);
#18149=AXIS2_PLACEMENT_3D('',#24431,#20319,#20320);
#18150=AXIS2_PLACEMENT_3D('',#24433,#20321,#20322);
#18151=AXIS2_PLACEMENT_3D('',#24434,#20323,#20324);
#18152=AXIS2_PLACEMENT_3D('',#24436,#20325,#20326);
#18153=AXIS2_PLACEMENT_3D('',#24438,#20327,#20328);
#18154=AXIS2_PLACEMENT_3D('',#24439,#20329,#20330);
#18155=AXIS2_PLACEMENT_3D('',#24441,#20331,#20332);
#18156=AXIS2_PLACEMENT_3D('',#24443,#20333,#20334);
#18157=AXIS2_PLACEMENT_3D('',#24444,#20335,#20336);
#18158=AXIS2_PLACEMENT_3D('',#24446,#20337,#20338);
#18159=AXIS2_PLACEMENT_3D('',#24448,#20339,#20340);
#18160=AXIS2_PLACEMENT_3D('',#24449,#20341,#20342);
#18161=AXIS2_PLACEMENT_3D('',#24451,#20343,#20344);
#18162=AXIS2_PLACEMENT_3D('',#24453,#20345,#20346);
#18163=AXIS2_PLACEMENT_3D('',#24454,#20347,#20348);
#18164=AXIS2_PLACEMENT_3D('',#24456,#20349,#20350);
#18165=AXIS2_PLACEMENT_3D('',#24458,#20351,#20352);
#18166=AXIS2_PLACEMENT_3D('',#24459,#20353,#20354);
#18167=AXIS2_PLACEMENT_3D('',#24461,#20355,#20356);
#18168=AXIS2_PLACEMENT_3D('',#24463,#20357,#20358);
#18169=AXIS2_PLACEMENT_3D('',#24464,#20359,#20360);
#18170=AXIS2_PLACEMENT_3D('',#24466,#20361,#20362);
#18171=AXIS2_PLACEMENT_3D('',#24468,#20363,#20364);
#18172=AXIS2_PLACEMENT_3D('',#24469,#20365,#20366);
#18173=AXIS2_PLACEMENT_3D('',#24471,#20367,#20368);
#18174=AXIS2_PLACEMENT_3D('',#24473,#20369,#20370);
#18175=AXIS2_PLACEMENT_3D('',#24474,#20371,#20372);
#18176=AXIS2_PLACEMENT_3D('',#24476,#20373,#20374);
#18177=AXIS2_PLACEMENT_3D('',#24478,#20375,#20376);
#18178=AXIS2_PLACEMENT_3D('',#24479,#20377,#20378);
#18179=AXIS2_PLACEMENT_3D('',#24481,#20379,#20380);
#18180=AXIS2_PLACEMENT_3D('',#24483,#20381,#20382);
#18181=AXIS2_PLACEMENT_3D('',#24484,#20383,#20384);
#18182=AXIS2_PLACEMENT_3D('',#24486,#20385,#20386);
#18183=AXIS2_PLACEMENT_3D('',#24488,#20387,#20388);
#18184=AXIS2_PLACEMENT_3D('',#24489,#20389,#20390);
#18185=AXIS2_PLACEMENT_3D('',#24491,#20391,#20392);
#18186=AXIS2_PLACEMENT_3D('',#24493,#20393,#20394);
#18187=AXIS2_PLACEMENT_3D('',#24494,#20395,#20396);
#18188=AXIS2_PLACEMENT_3D('',#24496,#20397,#20398);
#18189=AXIS2_PLACEMENT_3D('',#24498,#20399,#20400);
#18190=AXIS2_PLACEMENT_3D('',#24499,#20401,#20402);
#18191=AXIS2_PLACEMENT_3D('',#24501,#20403,#20404);
#18192=AXIS2_PLACEMENT_3D('',#24503,#20405,#20406);
#18193=AXIS2_PLACEMENT_3D('',#24504,#20407,#20408);
#18194=AXIS2_PLACEMENT_3D('',#24506,#20409,#20410);
#18195=AXIS2_PLACEMENT_3D('',#24508,#20411,#20412);
#18196=AXIS2_PLACEMENT_3D('',#24509,#20413,#20414);
#18197=AXIS2_PLACEMENT_3D('',#24511,#20415,#20416);
#18198=AXIS2_PLACEMENT_3D('',#24513,#20417,#20418);
#18199=AXIS2_PLACEMENT_3D('',#24514,#20419,#20420);
#18200=AXIS2_PLACEMENT_3D('',#24516,#20421,#20422);
#18201=AXIS2_PLACEMENT_3D('',#24518,#20423,#20424);
#18202=AXIS2_PLACEMENT_3D('',#24519,#20425,#20426);
#18203=AXIS2_PLACEMENT_3D('',#24521,#20427,#20428);
#18204=AXIS2_PLACEMENT_3D('',#24523,#20429,#20430);
#18205=AXIS2_PLACEMENT_3D('',#24524,#20431,#20432);
#18206=AXIS2_PLACEMENT_3D('',#24526,#20433,#20434);
#18207=AXIS2_PLACEMENT_3D('',#24528,#20435,#20436);
#18208=AXIS2_PLACEMENT_3D('',#24529,#20437,#20438);
#18209=AXIS2_PLACEMENT_3D('',#24531,#20439,#20440);
#18210=AXIS2_PLACEMENT_3D('',#24533,#20441,#20442);
#18211=AXIS2_PLACEMENT_3D('',#24534,#20443,#20444);
#18212=AXIS2_PLACEMENT_3D('',#24536,#20445,#20446);
#18213=AXIS2_PLACEMENT_3D('',#24538,#20447,#20448);
#18214=AXIS2_PLACEMENT_3D('',#24539,#20449,#20450);
#18215=AXIS2_PLACEMENT_3D('',#24541,#20451,#20452);
#18216=AXIS2_PLACEMENT_3D('',#24543,#20453,#20454);
#18217=AXIS2_PLACEMENT_3D('',#24544,#20455,#20456);
#18218=AXIS2_PLACEMENT_3D('',#24546,#20457,#20458);
#18219=AXIS2_PLACEMENT_3D('',#24548,#20459,#20460);
#18220=AXIS2_PLACEMENT_3D('',#24549,#20461,#20462);
#18221=AXIS2_PLACEMENT_3D('',#24551,#20463,#20464);
#18222=AXIS2_PLACEMENT_3D('',#24553,#20465,#20466);
#18223=AXIS2_PLACEMENT_3D('',#24554,#20467,#20468);
#18224=AXIS2_PLACEMENT_3D('',#24556,#20469,#20470);
#18225=AXIS2_PLACEMENT_3D('',#24558,#20471,#20472);
#18226=AXIS2_PLACEMENT_3D('',#24559,#20473,#20474);
#18227=AXIS2_PLACEMENT_3D('',#24561,#20475,#20476);
#18228=AXIS2_PLACEMENT_3D('',#24563,#20477,#20478);
#18229=AXIS2_PLACEMENT_3D('',#24564,#20479,#20480);
#18230=AXIS2_PLACEMENT_3D('',#24566,#20481,#20482);
#18231=AXIS2_PLACEMENT_3D('',#24568,#20483,#20484);
#18232=AXIS2_PLACEMENT_3D('',#24569,#20485,#20486);
#18233=AXIS2_PLACEMENT_3D('',#24571,#20487,#20488);
#18234=AXIS2_PLACEMENT_3D('',#24573,#20489,#20490);
#18235=AXIS2_PLACEMENT_3D('',#24574,#20491,#20492);
#18236=AXIS2_PLACEMENT_3D('',#24576,#20493,#20494);
#18237=AXIS2_PLACEMENT_3D('',#24578,#20495,#20496);
#18238=AXIS2_PLACEMENT_3D('',#24579,#20497,#20498);
#18239=AXIS2_PLACEMENT_3D('',#24581,#20499,#20500);
#18240=AXIS2_PLACEMENT_3D('',#24583,#20501,#20502);
#18241=AXIS2_PLACEMENT_3D('',#24584,#20503,#20504);
#18242=AXIS2_PLACEMENT_3D('',#24586,#20505,#20506);
#18243=AXIS2_PLACEMENT_3D('',#24588,#20507,#20508);
#18244=AXIS2_PLACEMENT_3D('',#24589,#20509,#20510);
#18245=AXIS2_PLACEMENT_3D('',#24591,#20511,#20512);
#18246=AXIS2_PLACEMENT_3D('',#24593,#20513,#20514);
#18247=AXIS2_PLACEMENT_3D('',#24594,#20515,#20516);
#18248=AXIS2_PLACEMENT_3D('',#24596,#20517,#20518);
#18249=AXIS2_PLACEMENT_3D('',#24598,#20519,#20520);
#18250=AXIS2_PLACEMENT_3D('',#24599,#20521,#20522);
#18251=AXIS2_PLACEMENT_3D('',#24601,#20523,#20524);
#18252=AXIS2_PLACEMENT_3D('',#24602,#20525,#20526);
#18253=AXIS2_PLACEMENT_3D('',#24604,#20527,#20528);
#18254=AXIS2_PLACEMENT_3D('',#24605,#20529,#20530);
#18255=AXIS2_PLACEMENT_3D('',#24608,#20533,#20534);
#18256=AXIS2_PLACEMENT_3D('',#24610,#20536,#20537);
#18257=AXIS2_PLACEMENT_3D('',#24612,#20539,#20540);
#18258=AXIS2_PLACEMENT_3D('',#24613,#20541,#20542);
#18259=AXIS2_PLACEMENT_3D('',#24615,#20544,#20545);
#18260=AXIS2_PLACEMENT_3D('',#24617,#20547,#20548);
#18261=AXIS2_PLACEMENT_3D('',#24618,#20549,#20550);
#18262=AXIS2_PLACEMENT_3D('',#24620,#20552,#20553);
#18263=AXIS2_PLACEMENT_3D('',#24622,#20555,#20556);
#18264=AXIS2_PLACEMENT_3D('',#24623,#20557,#20558);
#18265=AXIS2_PLACEMENT_3D('',#24625,#20560,#20561);
#18266=AXIS2_PLACEMENT_3D('',#24627,#20563,#20564);
#18267=AXIS2_PLACEMENT_3D('',#24628,#20565,#20566);
#18268=AXIS2_PLACEMENT_3D('',#24630,#20568,#20569);
#18269=AXIS2_PLACEMENT_3D('',#24632,#20571,#20572);
#18270=AXIS2_PLACEMENT_3D('',#24633,#20573,#20574);
#18271=AXIS2_PLACEMENT_3D('',#24635,#20576,#20577);
#18272=AXIS2_PLACEMENT_3D('',#24637,#20579,#20580);
#18273=AXIS2_PLACEMENT_3D('',#24638,#20581,#20582);
#18274=AXIS2_PLACEMENT_3D('',#24640,#20584,#20585);
#18275=AXIS2_PLACEMENT_3D('',#24642,#20587,#20588);
#18276=AXIS2_PLACEMENT_3D('',#24643,#20589,#20590);
#18277=AXIS2_PLACEMENT_3D('',#24645,#20592,#20593);
#18278=AXIS2_PLACEMENT_3D('',#24647,#20595,#20596);
#18279=AXIS2_PLACEMENT_3D('',#24648,#20597,#20598);
#18280=AXIS2_PLACEMENT_3D('',#24650,#20600,#20601);
#18281=AXIS2_PLACEMENT_3D('',#24652,#20603,#20604);
#18282=AXIS2_PLACEMENT_3D('',#24653,#20605,#20606);
#18283=AXIS2_PLACEMENT_3D('',#24655,#20608,#20609);
#18284=AXIS2_PLACEMENT_3D('',#24657,#20611,#20612);
#18285=AXIS2_PLACEMENT_3D('',#24658,#20613,#20614);
#18286=AXIS2_PLACEMENT_3D('',#24660,#20616,#20617);
#18287=AXIS2_PLACEMENT_3D('',#24662,#20619,#20620);
#18288=AXIS2_PLACEMENT_3D('',#24663,#20621,#20622);
#18289=AXIS2_PLACEMENT_3D('',#24665,#20624,#20625);
#18290=AXIS2_PLACEMENT_3D('',#24667,#20627,#20628);
#18291=AXIS2_PLACEMENT_3D('',#24668,#20629,#20630);
#18292=AXIS2_PLACEMENT_3D('',#24670,#20632,#20633);
#18293=AXIS2_PLACEMENT_3D('',#24672,#20635,#20636);
#18294=AXIS2_PLACEMENT_3D('',#24673,#20637,#20638);
#18295=AXIS2_PLACEMENT_3D('',#24675,#20640,#20641);
#18296=AXIS2_PLACEMENT_3D('',#24677,#20643,#20644);
#18297=AXIS2_PLACEMENT_3D('',#24678,#20645,#20646);
#18298=AXIS2_PLACEMENT_3D('',#24680,#20648,#20649);
#18299=AXIS2_PLACEMENT_3D('',#24682,#20651,#20652);
#18300=AXIS2_PLACEMENT_3D('',#24683,#20653,#20654);
#18301=AXIS2_PLACEMENT_3D('',#24685,#20656,#20657);
#18302=AXIS2_PLACEMENT_3D('',#24687,#20659,#20660);
#18303=AXIS2_PLACEMENT_3D('',#24688,#20661,#20662);
#18304=AXIS2_PLACEMENT_3D('',#24690,#20664,#20665);
#18305=AXIS2_PLACEMENT_3D('',#24692,#20667,#20668);
#18306=AXIS2_PLACEMENT_3D('',#24693,#20669,#20670);
#18307=AXIS2_PLACEMENT_3D('',#24695,#20672,#20673);
#18308=AXIS2_PLACEMENT_3D('',#24697,#20675,#20676);
#18309=AXIS2_PLACEMENT_3D('',#24698,#20677,#20678);
#18310=AXIS2_PLACEMENT_3D('',#24700,#20680,#20681);
#18311=AXIS2_PLACEMENT_3D('',#24702,#20683,#20684);
#18312=AXIS2_PLACEMENT_3D('',#24703,#20685,#20686);
#18313=AXIS2_PLACEMENT_3D('',#24705,#20688,#20689);
#18314=AXIS2_PLACEMENT_3D('',#24707,#20691,#20692);
#18315=AXIS2_PLACEMENT_3D('',#24708,#20693,#20694);
#18316=AXIS2_PLACEMENT_3D('',#24710,#20696,#20697);
#18317=AXIS2_PLACEMENT_3D('',#24712,#20699,#20700);
#18318=AXIS2_PLACEMENT_3D('',#24713,#20701,#20702);
#18319=AXIS2_PLACEMENT_3D('',#24715,#20704,#20705);
#18320=AXIS2_PLACEMENT_3D('',#24717,#20707,#20708);
#18321=AXIS2_PLACEMENT_3D('',#24718,#20709,#20710);
#18322=AXIS2_PLACEMENT_3D('',#24720,#20712,#20713);
#18323=AXIS2_PLACEMENT_3D('',#24722,#20715,#20716);
#18324=AXIS2_PLACEMENT_3D('',#24723,#20717,#20718);
#18325=AXIS2_PLACEMENT_3D('',#24725,#20720,#20721);
#18326=AXIS2_PLACEMENT_3D('',#24727,#20723,#20724);
#18327=AXIS2_PLACEMENT_3D('',#24728,#20725,#20726);
#18328=AXIS2_PLACEMENT_3D('',#24730,#20728,#20729);
#18329=AXIS2_PLACEMENT_3D('',#24732,#20731,#20732);
#18330=AXIS2_PLACEMENT_3D('',#24733,#20733,#20734);
#18331=AXIS2_PLACEMENT_3D('',#24735,#20736,#20737);
#18332=AXIS2_PLACEMENT_3D('',#24737,#20739,#20740);
#18333=AXIS2_PLACEMENT_3D('',#24738,#20741,#20742);
#18334=AXIS2_PLACEMENT_3D('',#24740,#20744,#20745);
#18335=AXIS2_PLACEMENT_3D('',#24742,#20747,#20748);
#18336=AXIS2_PLACEMENT_3D('',#24743,#20749,#20750);
#18337=AXIS2_PLACEMENT_3D('',#24745,#20752,#20753);
#18338=AXIS2_PLACEMENT_3D('',#24747,#20755,#20756);
#18339=AXIS2_PLACEMENT_3D('',#24748,#20757,#20758);
#18340=AXIS2_PLACEMENT_3D('',#24750,#20760,#20761);
#18341=AXIS2_PLACEMENT_3D('',#24752,#20763,#20764);
#18342=AXIS2_PLACEMENT_3D('',#24753,#20765,#20766);
#18343=AXIS2_PLACEMENT_3D('',#24755,#20768,#20769);
#18344=AXIS2_PLACEMENT_3D('',#24757,#20771,#20772);
#18345=AXIS2_PLACEMENT_3D('',#24758,#20773,#20774);
#18346=AXIS2_PLACEMENT_3D('',#24760,#20776,#20777);
#18347=AXIS2_PLACEMENT_3D('',#24762,#20779,#20780);
#18348=AXIS2_PLACEMENT_3D('',#24763,#20781,#20782);
#18349=AXIS2_PLACEMENT_3D('',#24765,#20784,#20785);
#18350=AXIS2_PLACEMENT_3D('',#24767,#20787,#20788);
#18351=AXIS2_PLACEMENT_3D('',#24768,#20789,#20790);
#18352=AXIS2_PLACEMENT_3D('',#24770,#20792,#20793);
#18353=AXIS2_PLACEMENT_3D('',#24772,#20795,#20796);
#18354=AXIS2_PLACEMENT_3D('',#24773,#20797,#20798);
#18355=AXIS2_PLACEMENT_3D('',#24775,#20800,#20801);
#18356=AXIS2_PLACEMENT_3D('',#24777,#20803,#20804);
#18357=AXIS2_PLACEMENT_3D('',#24778,#20805,#20806);
#18358=AXIS2_PLACEMENT_3D('',#24780,#20808,#20809);
#18359=AXIS2_PLACEMENT_3D('',#24782,#20811,#20812);
#18360=AXIS2_PLACEMENT_3D('',#24783,#20813,#20814);
#18361=AXIS2_PLACEMENT_3D('',#24785,#20816,#20817);
#18362=AXIS2_PLACEMENT_3D('',#24787,#20819,#20820);
#18363=AXIS2_PLACEMENT_3D('',#24788,#20821,#20822);
#18364=AXIS2_PLACEMENT_3D('',#24790,#20824,#20825);
#18365=AXIS2_PLACEMENT_3D('',#24792,#20827,#20828);
#18366=AXIS2_PLACEMENT_3D('',#24793,#20829,#20830);
#18367=AXIS2_PLACEMENT_3D('',#24795,#20832,#20833);
#18368=AXIS2_PLACEMENT_3D('',#24797,#20835,#20836);
#18369=AXIS2_PLACEMENT_3D('',#24798,#20837,#20838);
#18370=AXIS2_PLACEMENT_3D('',#24800,#20840,#20841);
#18371=AXIS2_PLACEMENT_3D('',#24802,#20843,#20844);
#18372=AXIS2_PLACEMENT_3D('',#24803,#20845,#20846);
#18373=AXIS2_PLACEMENT_3D('',#24805,#20848,#20849);
#18374=AXIS2_PLACEMENT_3D('',#24807,#20851,#20852);
#18375=AXIS2_PLACEMENT_3D('',#24808,#20853,#20854);
#18376=AXIS2_PLACEMENT_3D('',#24810,#20856,#20857);
#18377=AXIS2_PLACEMENT_3D('',#24812,#20859,#20860);
#18378=AXIS2_PLACEMENT_3D('',#24813,#20861,#20862);
#18379=AXIS2_PLACEMENT_3D('',#24815,#20864,#20865);
#18380=AXIS2_PLACEMENT_3D('',#24817,#20867,#20868);
#18381=AXIS2_PLACEMENT_3D('',#24818,#20869,#20870);
#18382=AXIS2_PLACEMENT_3D('',#24820,#20872,#20873);
#18383=AXIS2_PLACEMENT_3D('',#24822,#20875,#20876);
#18384=AXIS2_PLACEMENT_3D('',#24823,#20877,#20878);
#18385=AXIS2_PLACEMENT_3D('',#24825,#20880,#20881);
#18386=AXIS2_PLACEMENT_3D('',#24827,#20883,#20884);
#18387=AXIS2_PLACEMENT_3D('',#24828,#20885,#20886);
#18388=AXIS2_PLACEMENT_3D('',#24830,#20888,#20889);
#18389=AXIS2_PLACEMENT_3D('',#24832,#20891,#20892);
#18390=AXIS2_PLACEMENT_3D('',#24833,#20893,#20894);
#18391=AXIS2_PLACEMENT_3D('',#24835,#20896,#20897);
#18392=AXIS2_PLACEMENT_3D('',#24837,#20899,#20900);
#18393=AXIS2_PLACEMENT_3D('',#24838,#20901,#20902);
#18394=AXIS2_PLACEMENT_3D('',#24840,#20904,#20905);
#18395=AXIS2_PLACEMENT_3D('',#25296,#20906,#20907);
#18396=AXIS2_PLACEMENT_3D('',#25299,#20908,#20909);
#18397=AXIS2_PLACEMENT_3D('',#25300,#20910,#20911);
#18398=AXIS2_PLACEMENT_3D('',#25304,#20913,#20914);
#18399=AXIS2_PLACEMENT_3D('',#25305,#20915,#20916);
#18400=AXIS2_PLACEMENT_3D('',#25306,#20917,#20918);
#18401=AXIS2_PLACEMENT_3D('',#25308,#20919,#20920);
#18402=AXIS2_PLACEMENT_3D('',#25312,#20922,#20923);
#18403=AXIS2_PLACEMENT_3D('',#25313,#20924,#20925);
#18404=AXIS2_PLACEMENT_3D('',#25314,#20926,#20927);
#18405=AXIS2_PLACEMENT_3D('',#25317,#20928,#20929);
#18406=AXIS2_PLACEMENT_3D('',#25318,#20930,#20931);
#18407=AXIS2_PLACEMENT_3D('',#25322,#20933,#20934);
#18408=AXIS2_PLACEMENT_3D('',#25323,#20935,#20936);
#18409=AXIS2_PLACEMENT_3D('',#25324,#20937,#20938);
#18410=AXIS2_PLACEMENT_3D('',#25326,#20939,#20940);
#18411=AXIS2_PLACEMENT_3D('',#25330,#20942,#20943);
#18412=AXIS2_PLACEMENT_3D('',#25331,#20944,#20945);
#18413=AXIS2_PLACEMENT_3D('',#25332,#20946,#20947);
#18414=AXIS2_PLACEMENT_3D('',#25334,#20948,#20949);
#18415=AXIS2_PLACEMENT_3D('',#25336,#20950,#20951);
#18416=AXIS2_PLACEMENT_3D('',#25337,#20952,#20953);
#18417=AXIS2_PLACEMENT_3D('',#25339,#20954,#20955);
#18418=AXIS2_PLACEMENT_3D('',#25340,#20956,#20957);
#18419=AXIS2_PLACEMENT_3D('',#25343,#20958,#20959);
#18420=AXIS2_PLACEMENT_3D('',#25344,#20960,#20961);
#18421=AXIS2_PLACEMENT_3D('',#25347,#20963,#20964);
#18422=AXIS2_PLACEMENT_3D('',#25348,#20965,#20966);
#18423=AXIS2_PLACEMENT_3D('',#25351,#20967,#20968);
#18424=AXIS2_PLACEMENT_3D('',#25352,#20969,#20970);
#18425=AXIS2_PLACEMENT_3D('',#25355,#20972,#20973);
#18426=AXIS2_PLACEMENT_3D('',#25356,#20974,#20975);
#18427=AXIS2_PLACEMENT_3D('',#25358,#20976,#20977);
#18428=AXIS2_PLACEMENT_3D('',#25362,#20979,#20980);
#18429=AXIS2_PLACEMENT_3D('',#25363,#20981,#20982);
#18430=AXIS2_PLACEMENT_3D('',#25364,#20983,#20984);
#18431=AXIS2_PLACEMENT_3D('',#25366,#20985,#20986);
#18432=AXIS2_PLACEMENT_3D('',#25370,#20988,#20989);
#18433=AXIS2_PLACEMENT_3D('',#25371,#20990,#20991);
#18434=AXIS2_PLACEMENT_3D('',#25372,#20992,#20993);
#18435=AXIS2_PLACEMENT_3D('',#25375,#20994,#20995);
#18436=AXIS2_PLACEMENT_3D('',#25376,#20996,#20997);
#18437=AXIS2_PLACEMENT_3D('',#25379,#20999,#21000);
#18438=AXIS2_PLACEMENT_3D('',#25380,#21001,#21002);
#18439=AXIS2_PLACEMENT_3D('',#25383,#21003,#21004);
#18440=AXIS2_PLACEMENT_3D('',#25384,#21005,#21006);
#18441=AXIS2_PLACEMENT_3D('',#25387,#21008,#21009);
#18442=AXIS2_PLACEMENT_3D('',#25388,#21010,#21011);
#18443=AXIS2_PLACEMENT_3D('',#25390,#21012,#21013);
#18444=AXIS2_PLACEMENT_3D('',#25394,#21015,#21016);
#18445=AXIS2_PLACEMENT_3D('',#25395,#21017,#21018);
#18446=AXIS2_PLACEMENT_3D('',#25396,#21019,#21020);
#18447=AXIS2_PLACEMENT_3D('',#25399,#21021,#21022);
#18448=AXIS2_PLACEMENT_3D('',#25400,#21023,#21024);
#18449=AXIS2_PLACEMENT_3D('',#25403,#21026,#21027);
#18450=AXIS2_PLACEMENT_3D('',#25404,#21028,#21029);
#18451=AXIS2_PLACEMENT_3D('',#25406,#21030,#21031);
#18452=AXIS2_PLACEMENT_3D('',#25410,#21033,#21034);
#18453=AXIS2_PLACEMENT_3D('',#25411,#21035,#21036);
#18454=AXIS2_PLACEMENT_3D('',#25412,#21037,#21038);
#18455=AXIS2_PLACEMENT_3D('',#25415,#21039,#21040);
#18456=AXIS2_PLACEMENT_3D('',#25416,#21041,#21042);
#18457=AXIS2_PLACEMENT_3D('',#25419,#21044,#21045);
#18458=AXIS2_PLACEMENT_3D('',#25420,#21046,#21047);
#18459=AXIS2_PLACEMENT_3D('',#25422,#21048,#21049);
#18460=AXIS2_PLACEMENT_3D('',#25426,#21051,#21052);
#18461=AXIS2_PLACEMENT_3D('',#25427,#21053,#21054);
#18462=AXIS2_PLACEMENT_3D('',#25428,#21055,#21056);
#18463=AXIS2_PLACEMENT_3D('',#25431,#21057,#21058);
#18464=AXIS2_PLACEMENT_3D('',#25432,#21059,#21060);
#18465=AXIS2_PLACEMENT_3D('',#25435,#21062,#21063);
#18466=AXIS2_PLACEMENT_3D('',#25436,#21064,#21065);
#18467=AXIS2_PLACEMENT_3D('',#25438,#21066,#21067);
#18468=AXIS2_PLACEMENT_3D('',#25442,#21069,#21070);
#18469=AXIS2_PLACEMENT_3D('',#25443,#21071,#21072);
#18470=AXIS2_PLACEMENT_3D('',#25544,#21073,#21074);
#18471=AXIS2_PLACEMENT_3D('',#25555,#21075,#21076);
#18472=AXIS2_PLACEMENT_3D('',#25556,#21077,#21078);
#18473=AXIS2_PLACEMENT_3D('',#25558,#21079,#21080);
#18474=AXIS2_PLACEMENT_3D('',#25559,#21081,#21082);
#18475=AXIS2_PLACEMENT_3D('',#25688,#21083,#21084);
#18476=AXIS2_PLACEMENT_3D('',#25715,#21085,#21086);
#18477=AXIS2_PLACEMENT_3D('',#25729,#21087,#21088);
#18478=AXIS2_PLACEMENT_3D('',#25743,#21089,#21090);
#18479=AXIS2_PLACEMENT_3D('',#25744,#21091,#21092);
#18480=AXIS2_PLACEMENT_3D('',#25745,#21093,#21094);
#18481=AXIS2_PLACEMENT_3D('',#25746,#21095,#21096);
#18482=AXIS2_PLACEMENT_3D('',#25747,#21097,#21098);
#18483=AXIS2_PLACEMENT_3D('',#25748,#21099,#21100);
#18484=AXIS2_PLACEMENT_3D('',#25749,#21101,#21102);
#18485=AXIS2_PLACEMENT_3D('',#25750,#21103,#21104);
#18486=AXIS2_PLACEMENT_3D('',#25751,#21105,#21106);
#18487=AXIS2_PLACEMENT_3D('',#25752,#21107,#21108);
#18488=AXIS2_PLACEMENT_3D('',#25753,#21109,#21110);
#18489=AXIS2_PLACEMENT_3D('',#25754,#21111,#21112);
#18490=AXIS2_PLACEMENT_3D('',#25755,#21113,#21114);
#18491=AXIS2_PLACEMENT_3D('',#25756,#21115,#21116);
#18492=AXIS2_PLACEMENT_3D('',#25757,#21117,#21118);
#18493=AXIS2_PLACEMENT_3D('',#25758,#21119,#21120);
#18494=AXIS2_PLACEMENT_3D('',#25759,#21121,#21122);
#18495=AXIS2_PLACEMENT_3D('',#25760,#21123,#21124);
#18496=AXIS2_PLACEMENT_3D('',#25761,#21125,#21126);
#18497=AXIS2_PLACEMENT_3D('',#25762,#21127,#21128);
#18498=AXIS2_PLACEMENT_3D('',#25763,#21129,#21130);
#18499=AXIS2_PLACEMENT_3D('',#25764,#21131,#21132);
#18500=AXIS2_PLACEMENT_3D('',#25765,#21133,#21134);
#18501=AXIS2_PLACEMENT_3D('',#25766,#21135,#21136);
#18502=AXIS2_PLACEMENT_3D('',#25767,#21137,#21138);
#18503=AXIS2_PLACEMENT_3D('',#25768,#21139,#21140);
#18504=AXIS2_PLACEMENT_3D('',#25769,#21141,#21142);
#18505=AXIS2_PLACEMENT_3D('',#25770,#21143,#21144);
#18506=AXIS2_PLACEMENT_3D('',#25771,#21145,#21146);
#18507=AXIS2_PLACEMENT_3D('',#25772,#21147,#21148);
#18508=AXIS2_PLACEMENT_3D('',#25773,#21149,#21150);
#18509=AXIS2_PLACEMENT_3D('',#25774,#21151,#21152);
#18510=AXIS2_PLACEMENT_3D('',#25775,#21153,#21154);
#18511=AXIS2_PLACEMENT_3D('',#25776,#21155,#21156);
#18512=AXIS2_PLACEMENT_3D('',#25777,#21157,#21158);
#18513=AXIS2_PLACEMENT_3D('',#25778,#21159,#21160);
#18514=AXIS2_PLACEMENT_3D('',#25779,#21161,#21162);
#18515=AXIS2_PLACEMENT_3D('',#25780,#21163,#21164);
#18516=AXIS2_PLACEMENT_3D('',#25781,#21165,#21166);
#18517=AXIS2_PLACEMENT_3D('',#25839,#21167,#21168);
#18518=AXIS2_PLACEMENT_3D('',#25840,#21169,#21170);
#18519=AXIS2_PLACEMENT_3D('',#25843,#21171,#21172);
#18520=AXIS2_PLACEMENT_3D('',#25844,#21173,#21174);
#18521=AXIS2_PLACEMENT_3D('',#26092,#21175,#21176);
#18522=AXIS2_PLACEMENT_3D('',#27005,#21177,#21178);
#18523=AXIS2_PLACEMENT_3D('',#29780,#21194,#21195);
#18524=AXIS2_PLACEMENT_3D('',#29789,#21196,#21197);
#18525=AXIS2_PLACEMENT_3D('',#30303,#21198,#21199);
#18526=AXIS2_PLACEMENT_3D('',#31538,#21215,#21216);
#18527=AXIS2_PLACEMENT_3D('',#31908,#21217,#21218);
#18528=AXIS2_PLACEMENT_3D('',#31912,#21220,#21221);
#18529=AXIS2_PLACEMENT_3D('',#32079,#21223,#21224);
#18530=AXIS2_PLACEMENT_3D('',#35112,#21255,#21256);
#18531=AXIS2_PLACEMENT_3D('',#35124,#21257,#21258);
#18532=AXIS2_PLACEMENT_3D('',#35132,#21259,#21260);
#18533=AXIS2_PLACEMENT_3D('',#35144,#21262,#21263);
#18534=AXIS2_PLACEMENT_3D('',#35159,#21265,#21266);
#18535=AXIS2_PLACEMENT_3D('',#35164,#21267,#21268);
#18536=AXIS2_PLACEMENT_3D('',#35195,#21270,#21271);
#18537=AXIS2_PLACEMENT_3D('',#35203,#21272,#21273);
#18538=AXIS2_PLACEMENT_3D('',#35215,#21275,#21276);
#18539=AXIS2_PLACEMENT_3D('',#35386,#21277,#21278);
#18540=AXIS2_PLACEMENT_3D('',#35434,#21279,#21280);
#18541=AXIS2_PLACEMENT_3D('',#35461,#21281,#21282);
#18542=AXIS2_PLACEMENT_3D('',#35611,#21283,#21284);
#18543=AXIS2_PLACEMENT_3D('',#35704,#21285,#21286);
#18544=AXIS2_PLACEMENT_3D('',#35751,#21287,#21288);
#18545=AXIS2_PLACEMENT_3D('',#35821,#21289,#21290);
#18546=AXIS2_PLACEMENT_3D('',#35891,#21291,#21292);
#18547=AXIS2_PLACEMENT_3D('',#35913,#21293,#21294);
#18548=AXIS2_PLACEMENT_3D('',#35923,#21295,#21296);
#18549=AXIS2_PLACEMENT_3D('',#35978,#21299,#21300);
#18550=AXIS2_PLACEMENT_3D('',#36162,#21302,#21303);
#18551=AXIS2_PLACEMENT_3D('',#36346,#21305,#21306);
#18552=AXIS2_PLACEMENT_3D('',#36395,#21307,#21308);
#18553=AXIS2_PLACEMENT_3D('',#36405,#21309,#21310);
#18554=AXIS2_PLACEMENT_3D('',#36437,#21311,#21312);
#18555=AXIS2_PLACEMENT_3D('',#36467,#21313,#21314);
#18556=AXIS2_PLACEMENT_3D('',#36470,#21315,#21316);
#18557=AXIS2_PLACEMENT_3D('',#36485,#21317,#21318);
#18558=AXIS2_PLACEMENT_3D('',#36495,#21319,#21320);
#18559=AXIS2_PLACEMENT_3D('',#36566,#21321,#21322);
#18560=AXIS2_PLACEMENT_3D('',#36567,#21323,#21324);
#18561=AXIS2_PLACEMENT_3D('',#36568,#21325,#21326);
#18562=AXIS2_PLACEMENT_3D('',#36576,#21327,#21328);
#18563=AXIS2_PLACEMENT_3D('',#36577,#21329,#21330);
#18564=AXIS2_PLACEMENT_3D('',#36633,#21331,#21332);
#18565=AXIS2_PLACEMENT_3D('',#36641,#21333,#21334);
#18566=AXIS2_PLACEMENT_3D('',#36649,#21335,#21336);
#18567=AXIS2_PLACEMENT_3D('',#36678,#21337,#21338);
#18568=AXIS2_PLACEMENT_3D('',#36700,#21339,#21340);
#18569=AXIS2_PLACEMENT_3D('',#36701,#21341,#21342);
#18570=AXIS2_PLACEMENT_3D('',#36702,#21343,#21344);
#18571=AXIS2_PLACEMENT_3D('',#36703,#21345,#21346);
#18572=AXIS2_PLACEMENT_3D('',#36704,#21347,#21348);
#18573=AXIS2_PLACEMENT_3D('',#36705,#21349,#21350);
#18574=AXIS2_PLACEMENT_3D('',#36706,#21351,#21352);
#18575=AXIS2_PLACEMENT_3D('',#36793,#21353,#21354);
#18576=AXIS2_PLACEMENT_3D('',#36801,#21355,#21356);
#18577=AXIS2_PLACEMENT_3D('',#36842,#21357,#21358);
#18578=AXIS2_PLACEMENT_3D('',#36843,#21359,#21360);
#18579=AXIS2_PLACEMENT_3D('',#36844,#21361,#21362);
#18580=AXIS2_PLACEMENT_3D('',#36845,#21363,#21364);
#18581=AXIS2_PLACEMENT_3D('',#36846,#21365,#21366);
#18582=AXIS2_PLACEMENT_3D('',#36847,#21367,#21368);
#18583=AXIS2_PLACEMENT_3D('',#36848,#21369,#21370);
#18584=AXIS2_PLACEMENT_3D('',#36888,#21371,#21372);
#18585=AXIS2_PLACEMENT_3D('',#36889,#21373,#21374);
#18586=AXIS2_PLACEMENT_3D('',#36890,#21375,#21376);
#18587=AXIS2_PLACEMENT_3D('',#36912,#21377,#21378);
#18588=AXIS2_PLACEMENT_3D('',#36920,#21379,#21380);
#18589=AXIS2_PLACEMENT_3D('',#36921,#21381,#21382);
#18590=AXIS2_PLACEMENT_3D('',#36950,#21383,#21384);
#18591=AXIS2_PLACEMENT_3D('',#36951,#21385,#21386);
#18592=AXIS2_PLACEMENT_3D('',#36952,#21387,#21388);
#18593=AXIS2_PLACEMENT_3D('',#36981,#21389,#21390);
#18594=AXIS2_PLACEMENT_3D('',#36982,#21391,#21392);
#18595=AXIS2_PLACEMENT_3D('',#36983,#21393,#21394);
#18596=AXIS2_PLACEMENT_3D('',#36984,#21395,#21396);
#18597=AXIS2_PLACEMENT_3D('',#36985,#21397,#21398);
#18598=AXIS2_PLACEMENT_3D('',#36986,#21399,#21400);
#18599=AXIS2_PLACEMENT_3D('',#36987,#21401,#21402);
#18600=AXIS2_PLACEMENT_3D('',#37020,#21403,#21404);
#18601=AXIS2_PLACEMENT_3D('',#37021,#21405,#21406);
#18602=AXIS2_PLACEMENT_3D('',#37061,#21407,#21408);
#18603=AXIS2_PLACEMENT_3D('',#37062,#21409,#21410);
#18604=AXIS2_PLACEMENT_3D('',#37063,#21411,#21412);
#18605=AXIS2_PLACEMENT_3D('',#37064,#21413,#21414);
#18606=AXIS2_PLACEMENT_3D('',#37065,#21415,#21416);
#18607=AXIS2_PLACEMENT_3D('',#37066,#21417,#21418);
#18608=AXIS2_PLACEMENT_3D('',#37067,#21419,#21420);
#18609=AXIS2_PLACEMENT_3D('',#37068,#21421,#21422);
#18610=AXIS2_PLACEMENT_3D('',#37069,#21423,#21424);
#18611=AXIS2_PLACEMENT_3D('',#37070,#21425,#21426);
#18612=AXIS2_PLACEMENT_3D('',#37071,#21427,#21428);
#18613=AXIS2_PLACEMENT_3D('',#37108,#21429,#21430);
#18614=AXIS2_PLACEMENT_3D('',#37145,#21431,#21432);
#18615=AXIS2_PLACEMENT_3D('',#37146,#21433,#21434);
#18616=AXIS2_PLACEMENT_3D('',#37147,#21435,#21436);
#18617=AXIS2_PLACEMENT_3D('',#37311,#21437,#21438);
#18618=AXIS2_PLACEMENT_3D('',#37320,#21439,#21440);
#18619=AXIS2_PLACEMENT_3D('',#37334,#21441,#21442);
#18620=AXIS2_PLACEMENT_3D('',#37408,#21443,#21444);
#18621=AXIS2_PLACEMENT_3D('',#37497,#21445,#21446);
#18622=AXIS2_PLACEMENT_3D('',#37648,#21447,#21448);
#18623=AXIS2_PLACEMENT_3D('',#37844,#21449,#21450);
#18624=AXIS2_PLACEMENT_3D('',#37931,#21451,#21452);
#18625=AXIS2_PLACEMENT_3D('',#38086,#21453,#21454);
#18626=AXIS2_PLACEMENT_3D('',#38177,#21455,#21456);
#18627=AXIS2_PLACEMENT_3D('',#38333,#21457,#21458);
#18628=AXIS2_PLACEMENT_3D('',#38421,#21459,#21460);
#18629=AXIS2_PLACEMENT_3D('',#38507,#21461,#21462);
#18630=AXIS2_PLACEMENT_3D('',#38595,#21463,#21464);
#18631=AXIS2_PLACEMENT_3D('',#38682,#21465,#21466);
#18632=AXIS2_PLACEMENT_3D('',#38775,#21467,#21468);
#18633=AXIS2_PLACEMENT_3D('',#38892,#21469,#21470);
#18634=AXIS2_PLACEMENT_3D('',#38989,#21471,#21472);
#18635=AXIS2_PLACEMENT_3D('',#39075,#21473,#21474);
#18636=AXIS2_PLACEMENT_3D('',#39162,#21475,#21476);
#18637=AXIS2_PLACEMENT_3D('',#39171,#21477,#21478);
#18638=AXIS2_PLACEMENT_3D('',#39172,#21479,#21480);
#18639=AXIS2_PLACEMENT_3D('',#39246,#21481,#21482);
#18640=AXIS2_PLACEMENT_3D('',#39333,#21483,#21484);
#18641=AXIS2_PLACEMENT_3D('',#39482,#21485,#21486);
#18642=AXIS2_PLACEMENT_3D('',#39663,#21487,#21488);
#18643=AXIS2_PLACEMENT_3D('',#39748,#21489,#21490);
#18644=AXIS2_PLACEMENT_3D('',#39899,#21491,#21492);
#18645=AXIS2_PLACEMENT_3D('',#39986,#21493,#21494);
#18646=AXIS2_PLACEMENT_3D('',#40137,#21495,#21496);
#18647=AXIS2_PLACEMENT_3D('',#40253,#21497,#21498);
#18648=AXIS2_PLACEMENT_3D('',#40365,#21499,#21500);
#18649=AXIS2_PLACEMENT_3D('',#40448,#21501,#21502);
#18650=AXIS2_PLACEMENT_3D('',#40531,#21503,#21504);
#18651=AXIS2_PLACEMENT_3D('',#40618,#21505,#21506);
#18652=AXIS2_PLACEMENT_3D('',#40728,#21507,#21508);
#18653=AXIS2_PLACEMENT_3D('',#40824,#21509,#21510);
#18654=AXIS2_PLACEMENT_3D('',#40907,#21511,#21512);
#18655=AXIS2_PLACEMENT_3D('',#40989,#21513,#21514);
#18656=AXIS2_PLACEMENT_3D('',#40990,#21515,#21516);
#18657=AXIS2_PLACEMENT_3D('',#41035,#21517,#21518);
#18658=AXIS2_PLACEMENT_3D('',#41107,#21519,#21520);
#18659=AXIS2_PLACEMENT_3D('',#41124,#21521,#21522);
#18660=AXIS2_PLACEMENT_3D('',#41169,#21523,#21524);
#18661=AXIS2_PLACEMENT_3D('',#41244,#21525,#21526);
#18662=AXIS2_PLACEMENT_3D('',#41317,#21527,#21528);
#18663=AXIS2_PLACEMENT_3D('',#41392,#21529,#21530);
#18664=AXIS2_PLACEMENT_3D('',#41465,#21531,#21532);
#18665=AXIS2_PLACEMENT_3D('',#41540,#21533,#21534);
#18666=AXIS2_PLACEMENT_3D('',#41613,#21535,#21536);
#18667=AXIS2_PLACEMENT_3D('',#41687,#21537,#21538);
#18668=AXIS2_PLACEMENT_3D('',#41762,#21539,#21540);
#18669=AXIS2_PLACEMENT_3D('',#41838,#21541,#21542);
#18670=AXIS2_PLACEMENT_3D('',#41915,#21543,#21544);
#18671=AXIS2_PLACEMENT_3D('',#42001,#21545,#21546);
#18672=AXIS2_PLACEMENT_3D('',#42079,#21547,#21548);
#18673=AXIS2_PLACEMENT_3D('',#42154,#21549,#21550);
#18674=AXIS2_PLACEMENT_3D('',#42227,#21551,#21552);
#18675=AXIS2_PLACEMENT_3D('',#42301,#21553,#21554);
#18676=AXIS2_PLACEMENT_3D('',#42375,#21555,#21556);
#18677=AXIS2_PLACEMENT_3D('',#42449,#21557,#21558);
#18678=AXIS2_PLACEMENT_3D('',#42523,#21559,#21560);
#18679=AXIS2_PLACEMENT_3D('',#42597,#21561,#21562);
#18680=AXIS2_PLACEMENT_3D('',#42671,#21563,#21564);
#18681=AXIS2_PLACEMENT_3D('',#42745,#21565,#21566);
#18682=AXIS2_PLACEMENT_3D('',#42816,#21567,#21568);
#18683=AXIS2_PLACEMENT_3D('',#42892,#21569,#21570);
#18684=AXIS2_PLACEMENT_3D('',#43204,#21571,#21572);
#18685=AXIS2_PLACEMENT_3D('',#43350,#21573,#21574);
#18686=AXIS2_PLACEMENT_3D('',#43419,#21575,#21576);
#18687=AXIS2_PLACEMENT_3D('',#43512,#21577,#21578);
#18688=AXIS2_PLACEMENT_3D('',#43520,#21579,#21580);
#18689=AXIS2_PLACEMENT_3D('',#43545,#21581,#21582);
#18690=AXIS2_PLACEMENT_3D('',#43605,#21583,#21584);
#18691=AXIS2_PLACEMENT_3D('',#43622,#21585,#21586);
#18692=AXIS2_PLACEMENT_3D('',#43638,#21587,#21588);
#18693=AXIS2_PLACEMENT_3D('',#43771,#21589,#21590);
#18694=AXIS2_PLACEMENT_3D('',#43787,#21591,#21592);
#18695=AXIS2_PLACEMENT_3D('',#43920,#21593,#21594);
#18696=AXIS2_PLACEMENT_3D('',#43935,#21595,#21596);
#18697=AXIS2_PLACEMENT_3D('',#44068,#21597,#21598);
#18698=AXIS2_PLACEMENT_3D('',#44083,#21599,#21600);
#18699=AXIS2_PLACEMENT_3D('',#44216,#21601,#21602);
#18700=AXIS2_PLACEMENT_3D('',#44232,#21603,#21604);
#18701=AXIS2_PLACEMENT_3D('',#44366,#21605,#21606);
#18702=AXIS2_PLACEMENT_3D('',#44382,#21607,#21608);
#18703=AXIS2_PLACEMENT_3D('',#44520,#21609,#21610);
#18704=AXIS2_PLACEMENT_3D('',#44536,#21611,#21612);
#18705=AXIS2_PLACEMENT_3D('',#44687,#21613,#21614);
#18706=AXIS2_PLACEMENT_3D('',#44703,#21615,#21616);
#18707=AXIS2_PLACEMENT_3D('',#44849,#21617,#21618);
#18708=AXIS2_PLACEMENT_3D('',#44865,#21619,#21620);
#18709=AXIS2_PLACEMENT_3D('',#45010,#21621,#21622);
#18710=AXIS2_PLACEMENT_3D('',#45026,#21623,#21624);
#18711=AXIS2_PLACEMENT_3D('',#45158,#21625,#21626);
#18712=AXIS2_PLACEMENT_3D('',#45174,#21627,#21628);
#18713=AXIS2_PLACEMENT_3D('',#45301,#21629,#21630);
#18714=AXIS2_PLACEMENT_3D('',#45317,#21631,#21632);
#18715=AXIS2_PLACEMENT_3D('',#45455,#21633,#21634);
#18716=AXIS2_PLACEMENT_3D('',#45470,#21635,#21636);
#18717=AXIS2_PLACEMENT_3D('',#45882,#21637,#21638);
#18718=AXIS2_PLACEMENT_3D('',#45948,#21639,#21640);
#18719=AXIS2_PLACEMENT_3D('',#45962,#21641,#21642);
#18720=AXIS2_PLACEMENT_3D('',#46088,#21643,#21644);
#18721=AXIS2_PLACEMENT_3D('',#46093,#21645,#21646);
#18722=AXIS2_PLACEMENT_3D('',#46116,#21647,#21648);
#18723=AXIS2_PLACEMENT_3D('',#46139,#21649,#21650);
#18724=AXIS2_PLACEMENT_3D('',#46154,#21651,#21652);
#18725=AXIS2_PLACEMENT_3D('',#46165,#21653,#21654);
#18726=AXIS2_PLACEMENT_3D('',#46173,#21655,#21656);
#18727=AXIS2_PLACEMENT_3D('',#46215,#21657,#21658);
#18728=AXIS2_PLACEMENT_3D('',#46251,#21659,#21660);
#18729=AXIS2_PLACEMENT_3D('',#46262,#21661,#21662);
#18730=AXIS2_PLACEMENT_3D('',#46292,#21663,#21664);
#18731=AXIS2_PLACEMENT_3D('',#46372,#21665,#21666);
#18732=AXIS2_PLACEMENT_3D('',#46456,#21667,#21668);
#18733=AXIS2_PLACEMENT_3D('',#46499,#21669,#21670);
#18734=AXIS2_PLACEMENT_3D('',#46515,#21671,#21672);
#18735=AXIS2_PLACEMENT_3D('',#46532,#21673,#21674);
#18736=AXIS2_PLACEMENT_3D('',#46548,#21675,#21676);
#18737=AXIS2_PLACEMENT_3D('',#46598,#21677,#21678);
#18738=AXIS2_PLACEMENT_3D('',#46698,#21679,#21680);
#18739=AXIS2_PLACEMENT_3D('',#46767,#21681,#21682);
#18740=AXIS2_PLACEMENT_3D('',#46830,#21683,#21684);
#18741=AXIS2_PLACEMENT_3D('',#46838,#21685,#21686);
#18742=AXIS2_PLACEMENT_3D('',#46880,#21687,#21688);
#18743=AXIS2_PLACEMENT_3D('',#46913,#21689,#21690);
#18744=AXIS2_PLACEMENT_3D('',#46924,#21691,#21692);
#18745=AXIS2_PLACEMENT_3D('',#46932,#21693,#21694);
#18746=AXIS2_PLACEMENT_3D('',#46940,#21695,#21696);
#18747=AXIS2_PLACEMENT_3D('',#47199,#21697,#21698);
#18748=AXIS2_PLACEMENT_3D('',#47517,#21699,#21700);
#18749=AXIS2_PLACEMENT_3D('',#47623,#21701,#21702);
#18750=AXIS2_PLACEMENT_3D('',#47663,#21703,#21704);
#18751=AXIS2_PLACEMENT_3D('',#47665,#21705,#21706);
#18752=AXIS2_PLACEMENT_3D('',#47668,#21707,#21708);
#18753=AXIS2_PLACEMENT_3D('',#47670,#21709,#21710);
#18754=AXIS2_PLACEMENT_3D('',#47672,#21711,#21712);
#18755=AXIS2_PLACEMENT_3D('',#47674,#21713,#21714);
#18756=AXIS2_PLACEMENT_3D('',#47676,#21715,#21716);
#18757=AXIS2_PLACEMENT_3D('',#47678,#21717,#21718);
#18758=AXIS2_PLACEMENT_3D('',#47680,#21719,#21720);
#18759=AXIS2_PLACEMENT_3D('',#47681,#21721,#21722);
#18760=AXIS2_PLACEMENT_3D('',#47682,#21723,#21724);
#18761=AXIS2_PLACEMENT_3D('',#47684,#21725,#21726);
#18762=AXIS2_PLACEMENT_3D('',#47686,#21728,#21729);
#18763=AXIS2_PLACEMENT_3D('',#47688,#21730,#21731);
#18764=AXIS2_PLACEMENT_3D('',#47689,#21732,#21733);
#18765=AXIS2_PLACEMENT_3D('',#47692,#21734,#21735);
#18766=AXIS2_PLACEMENT_3D('',#47694,#21736,#21737);
#18767=AXIS2_PLACEMENT_3D('',#47696,#21738,#21739);
#18768=AXIS2_PLACEMENT_3D('',#47698,#21740,#21741);
#18769=AXIS2_PLACEMENT_3D('',#47700,#21742,#21743);
#18770=AXIS2_PLACEMENT_3D('',#47702,#21744,#21745);
#18771=AXIS2_PLACEMENT_3D('',#47704,#21746,#21747);
#18772=AXIS2_PLACEMENT_3D('',#47705,#21748,#21749);
#18773=AXIS2_PLACEMENT_3D('',#47707,#21750,#21751);
#18774=AXIS2_PLACEMENT_3D('',#47708,#21752,#21753);
#18775=AXIS2_PLACEMENT_3D('',#47711,#21756,#21757);
#18776=AXIS2_PLACEMENT_3D('',#47718,#21760,#21761);
#18777=AXIS2_PLACEMENT_3D('',#47721,#21764,#21765);
#18778=AXIS2_PLACEMENT_3D('',#47724,#21768,#21769);
#18779=AXIS2_PLACEMENT_3D('',#47725,#21770,#21771);
#18780=AXIS2_PLACEMENT_3D('',#47726,#21772,#21773);
#18781=AXIS2_PLACEMENT_3D('',#47727,#21774,#21775);
#18782=AXIS2_PLACEMENT_3D('',#47728,#21776,#21777);
#18783=AXIS2_PLACEMENT_3D('',#47732,#21779,#21780);
#18784=AXIS2_PLACEMENT_3D('',#47733,#21781,#21782);
#18785=AXIS2_PLACEMENT_3D('',#47734,#21783,#21784);
#18786=AXIS2_PLACEMENT_3D('',#47736,#21785,#21786);
#18787=AXIS2_PLACEMENT_3D('',#47738,#21787,#21788);
#18788=AXIS2_PLACEMENT_3D('',#47739,#21789,#21790);
#18789=AXIS2_PLACEMENT_3D('',#47740,#21791,#21792);
#18790=AXIS2_PLACEMENT_3D('',#47741,#21793,#21794);
#18791=AXIS2_PLACEMENT_3D('',#47743,#21795,#21796);
#18792=AXIS2_PLACEMENT_3D('',#47746,#21798,#21799);
#18793=AXIS2_PLACEMENT_3D('',#47747,#21800,#21801);
#18794=AXIS2_PLACEMENT_3D('',#47749,#21802,#21803);
#18795=AXIS2_PLACEMENT_3D('',#47750,#21804,#21805);
#18796=AXIS2_PLACEMENT_3D('',#47763,#21807,#21808);
#18797=AXIS2_PLACEMENT_3D('',#47766,#21809,#21810);
#18798=AXIS2_PLACEMENT_3D('',#47781,#21812,#21813);
#18799=AXIS2_PLACEMENT_3D('',#47782,#21814,#21815);
#18800=AXIS2_PLACEMENT_3D('',#47783,#21816,#21817);
#18801=AXIS2_PLACEMENT_3D('',#47868,#21818,#21819);
#18802=AXIS2_PLACEMENT_3D('',#47870,#21820,#21821);
#18803=AXIS2_PLACEMENT_3D('',#47871,#21822,#21823);
#18804=AXIS2_PLACEMENT_3D('',#47943,#21825,#21826);
#18805=AXIS2_PLACEMENT_3D('',#47944,#21827,#21828);
#18806=AXIS2_PLACEMENT_3D('',#47978,#21829,#21830);
#18807=AXIS2_PLACEMENT_3D('',#47979,#21831,#21832);
#18808=AXIS2_PLACEMENT_3D('',#47980,#21833,#21834);
#18809=AXIS2_PLACEMENT_3D('',#47981,#21835,#21836);
#18810=AXIS2_PLACEMENT_3D('',#47982,#21837,#21838);
#18811=AXIS2_PLACEMENT_3D('',#47983,#21839,#21840);
#18812=AXIS2_PLACEMENT_3D('',#47984,#21841,#21842);
#18813=AXIS2_PLACEMENT_3D('',#47985,#21843,#21844);
#18814=AXIS2_PLACEMENT_3D('',#48006,#21854,#21855);
#18815=AXIS2_PLACEMENT_3D('',#48008,#21856,#21857);
#18816=AXIS2_PLACEMENT_3D('',#48010,#21858,#21859);
#18817=AXIS2_PLACEMENT_3D('',#48021,#21865,#21866);
#18818=AXIS2_PLACEMENT_3D('',#48022,#21867,#21868);
#18819=AXIS2_PLACEMENT_3D('',#48053,#21883,#21884);
#18820=AXIS2_PLACEMENT_3D('',#48055,#21885,#21886);
#18821=AXIS2_PLACEMENT_3D('',#48056,#21887,#21888);
#18822=AXIS2_PLACEMENT_3D('',#48058,#21889,#21890);
#18823=AXIS2_PLACEMENT_3D('',#48059,#21891,#21892);
#18824=AXIS2_PLACEMENT_3D('',#48068,#21897,#21898);
#18825=AXIS2_PLACEMENT_3D('',#48074,#21902,#21903);
#18826=AXIS2_PLACEMENT_3D('',#48080,#21907,#21908);
#18827=AXIS2_PLACEMENT_3D('',#48086,#21912,#21913);
#18828=AXIS2_PLACEMENT_3D('',#48092,#21917,#21918);
#18829=AXIS2_PLACEMENT_3D('',#48098,#21922,#21923);
#18830=AXIS2_PLACEMENT_3D('',#48104,#21927,#21928);
#18831=AXIS2_PLACEMENT_3D('',#48110,#21932,#21933);
#18832=AXIS2_PLACEMENT_3D('',#48116,#21937,#21938);
#18833=AXIS2_PLACEMENT_3D('',#48121,#21940,#21941);
#18834=AXIS2_PLACEMENT_3D('',#48124,#21943,#21944);
#18835=AXIS2_PLACEMENT_3D('',#48125,#21945,#21946);
#18836=AXIS2_PLACEMENT_3D('',#48134,#21951,#21952);
#18837=AXIS2_PLACEMENT_3D('',#48140,#21956,#21957);
#18838=AXIS2_PLACEMENT_3D('',#48146,#21961,#21962);
#18839=AXIS2_PLACEMENT_3D('',#48152,#21966,#21967);
#18840=AXIS2_PLACEMENT_3D('',#48155,#21970,#21971);
#18841=AXIS2_PLACEMENT_3D('',#48158,#21972,#21973);
#18842=AXIS2_PLACEMENT_3D('',#48159,#21974,#21975);
#18843=AXIS2_PLACEMENT_3D('',#48162,#21977,#21978);
#18844=AXIS2_PLACEMENT_3D('',#48163,#21979,#21980);
#18845=AXIS2_PLACEMENT_3D('',#48164,#21981,#21982);
#18846=AXIS2_PLACEMENT_3D('',#48165,#21983,#21984);
#18847=AXIS2_PLACEMENT_3D('',#48166,#21985,#21986);
#18848=AXIS2_PLACEMENT_3D('',#48167,#21987,#21988);
#18849=AXIS2_PLACEMENT_3D('',#48168,#21989,#21990);
#18850=AXIS2_PLACEMENT_3D('',#48169,#21991,#21992);
#18851=AXIS2_PLACEMENT_3D('',#48170,#21993,#21994);
#18852=AXIS2_PLACEMENT_3D('',#48171,#21995,#21996);
#18853=AXIS2_PLACEMENT_3D('',#48172,#21997,#21998);
#18854=AXIS2_PLACEMENT_3D('',#48173,#21999,#22000);
#18855=AXIS2_PLACEMENT_3D('',#48174,#22001,#22002);
#18856=AXIS2_PLACEMENT_3D('',#48175,#22003,#22004);
#18857=AXIS2_PLACEMENT_3D('',#48176,#22005,#22006);
#18858=AXIS2_PLACEMENT_3D('',#48177,#22007,#22008);
#18859=AXIS2_PLACEMENT_3D('',#48178,#22009,#22010);
#18860=AXIS2_PLACEMENT_3D('',#48179,#22011,#22012);
#18861=AXIS2_PLACEMENT_3D('',#48180,#22013,#22014);
#18862=AXIS2_PLACEMENT_3D('',#48181,#22015,#22016);
#18863=AXIS2_PLACEMENT_3D('',#48182,#22017,#22018);
#18864=AXIS2_PLACEMENT_3D('',#48183,#22019,#22020);
#18865=AXIS2_PLACEMENT_3D('',#48184,#22021,#22022);
#18866=AXIS2_PLACEMENT_3D('',#48185,#22023,#22024);
#18867=AXIS2_PLACEMENT_3D('',#48186,#22025,#22026);
#18868=AXIS2_PLACEMENT_3D('',#48187,#22027,#22028);
#18869=AXIS2_PLACEMENT_3D('',#48188,#22029,#22030);
#18870=AXIS2_PLACEMENT_3D('',#48189,#22031,#22032);
#18871=AXIS2_PLACEMENT_3D('',#48190,#22033,#22034);
#18872=AXIS2_PLACEMENT_3D('',#48191,#22035,#22036);
#18873=AXIS2_PLACEMENT_3D('',#48192,#22037,#22038);
#18874=AXIS2_PLACEMENT_3D('',#48193,#22039,#22040);
#18875=AXIS2_PLACEMENT_3D('',#48194,#22041,#22042);
#18876=AXIS2_PLACEMENT_3D('',#48195,#22043,#22044);
#18877=AXIS2_PLACEMENT_3D('',#48196,#22045,#22046);
#18878=AXIS2_PLACEMENT_3D('',#48197,#22047,#22048);
#18879=AXIS2_PLACEMENT_3D('',#48198,#22049,#22050);
#18880=AXIS2_PLACEMENT_3D('',#48199,#22051,#22052);
#18881=AXIS2_PLACEMENT_3D('',#48200,#22053,#22054);
#18882=AXIS2_PLACEMENT_3D('',#48201,#22055,#22056);
#18883=AXIS2_PLACEMENT_3D('',#48202,#22057,#22058);
#18884=AXIS2_PLACEMENT_3D('',#48203,#22059,#22060);
#18885=AXIS2_PLACEMENT_3D('',#48204,#22061,#22062);
#18886=AXIS2_PLACEMENT_3D('',#48205,#22063,#22064);
#18887=AXIS2_PLACEMENT_3D('',#48206,#22065,#22066);
#18888=AXIS2_PLACEMENT_3D('',#48207,#22067,#22068);
#18889=AXIS2_PLACEMENT_3D('',#48208,#22069,#22070);
#18890=AXIS2_PLACEMENT_3D('',#48209,#22071,#22072);
#18891=AXIS2_PLACEMENT_3D('',#48210,#22073,#22074);
#18892=AXIS2_PLACEMENT_3D('',#48211,#22075,#22076);
#18893=AXIS2_PLACEMENT_3D('',#48212,#22077,#22078);
#18894=AXIS2_PLACEMENT_3D('',#48213,#22079,#22080);
#18895=AXIS2_PLACEMENT_3D('',#48214,#22081,#22082);
#18896=AXIS2_PLACEMENT_3D('',#48215,#22083,#22084);
#18897=AXIS2_PLACEMENT_3D('',#48216,#22085,#22086);
#18898=AXIS2_PLACEMENT_3D('',#48217,#22087,#22088);
#18899=AXIS2_PLACEMENT_3D('',#48218,#22089,#22090);
#18900=AXIS2_PLACEMENT_3D('',#48219,#22091,#22092);
#18901=AXIS2_PLACEMENT_3D('',#48220,#22093,#22094);
#18902=AXIS2_PLACEMENT_3D('',#48221,#22095,#22096);
#18903=AXIS2_PLACEMENT_3D('',#48222,#22097,#22098);
#18904=AXIS2_PLACEMENT_3D('',#48223,#22099,#22100);
#18905=AXIS2_PLACEMENT_3D('',#48224,#22101,#22102);
#18906=AXIS2_PLACEMENT_3D('',#48225,#22103,#22104);
#18907=AXIS2_PLACEMENT_3D('',#48226,#22105,#22106);
#18908=AXIS2_PLACEMENT_3D('',#48227,#22107,#22108);
#18909=AXIS2_PLACEMENT_3D('',#48228,#22109,#22110);
#18910=AXIS2_PLACEMENT_3D('',#48229,#22111,#22112);
#18911=AXIS2_PLACEMENT_3D('',#48230,#22113,#22114);
#18912=AXIS2_PLACEMENT_3D('',#48231,#22115,#22116);
#18913=AXIS2_PLACEMENT_3D('',#48232,#22117,#22118);
#18914=AXIS2_PLACEMENT_3D('',#48233,#22119,#22120);
#18915=AXIS2_PLACEMENT_3D('',#48234,#22121,#22122);
#18916=AXIS2_PLACEMENT_3D('',#48235,#22123,#22124);
#18917=AXIS2_PLACEMENT_3D('',#48236,#22125,#22126);
#18918=AXIS2_PLACEMENT_3D('',#48237,#22127,#22128);
#18919=AXIS2_PLACEMENT_3D('',#48238,#22129,#22130);
#18920=AXIS2_PLACEMENT_3D('',#48239,#22131,#22132);
#18921=AXIS2_PLACEMENT_3D('',#48240,#22133,#22134);
#18922=AXIS2_PLACEMENT_3D('',#48241,#22135,#22136);
#18923=AXIS2_PLACEMENT_3D('',#48242,#22137,#22138);
#18924=AXIS2_PLACEMENT_3D('',#48247,#22140,#22141);
#18925=AXIS2_PLACEMENT_3D('',#48250,#22143,#22144);
#18926=AXIS2_PLACEMENT_3D('',#48251,#22145,#22146);
#18927=AXIS2_PLACEMENT_3D('',#48260,#22151,#22152);
#18928=AXIS2_PLACEMENT_3D('',#48269,#22157,#22158);
#18929=AXIS2_PLACEMENT_3D('',#48275,#22162,#22163);
#18930=AXIS2_PLACEMENT_3D('',#48281,#22167,#22168);
#18931=AXIS2_PLACEMENT_3D('',#48287,#22172,#22173);
#18932=AXIS2_PLACEMENT_3D('',#48293,#22177,#22178);
#18933=AXIS2_PLACEMENT_3D('',#48299,#22182,#22183);
#18934=AXIS2_PLACEMENT_3D('',#48305,#22187,#22188);
#18935=AXIS2_PLACEMENT_3D('',#48311,#22192,#22193);
#18936=AXIS2_PLACEMENT_3D('',#48317,#22197,#22198);
#18937=AXIS2_PLACEMENT_3D('',#48323,#22202,#22203);
#18938=AXIS2_PLACEMENT_3D('',#48329,#22207,#22208);
#18939=AXIS2_PLACEMENT_3D('',#48335,#22212,#22213);
#18940=AXIS2_PLACEMENT_3D('',#48344,#22218,#22219);
#18941=AXIS2_PLACEMENT_3D('',#48353,#22223,#22224);
#18942=AXIS2_PLACEMENT_3D('',#48355,#22225,#22226);
#18943=AXIS2_PLACEMENT_3D('',#48357,#22227,#22228);
#18944=AXIS2_PLACEMENT_3D('',#48361,#22230,#22231);
#18945=AXIS2_PLACEMENT_3D('',#48382,#22242,#22243);
#18946=AXIS2_PLACEMENT_3D('',#48383,#22244,#22245);
#18947=AXIS2_PLACEMENT_3D('',#48392,#22249,#22250);
#18948=AXIS2_PLACEMENT_3D('',#48396,#22252,#22253);
#18949=AXIS2_PLACEMENT_3D('',#48398,#22254,#22255);
#18950=AXIS2_PLACEMENT_3D('',#48400,#22256,#22257);
#18951=AXIS2_PLACEMENT_3D('',#48421,#22268,#22269);
#18952=AXIS2_PLACEMENT_3D('',#48422,#22270,#22271);
#18953=AXIS2_PLACEMENT_3D('',#48425,#22272,#22273);
#18954=AXIS2_PLACEMENT_3D('',#48426,#22274,#22275);
#18955=AXIS2_PLACEMENT_3D('',#48429,#22277,#22278);
#18956=AXIS2_PLACEMENT_3D('',#48430,#22279,#22280);
#18957=AXIS2_PLACEMENT_3D('',#48431,#22281,#22282);
#18958=AXIS2_PLACEMENT_3D('',#48432,#22283,#22284);
#18959=AXIS2_PLACEMENT_3D('',#48433,#22285,#22286);
#18960=AXIS2_PLACEMENT_3D('',#48434,#22287,#22288);
#18961=AXIS2_PLACEMENT_3D('',#48435,#22289,#22290);
#18962=AXIS2_PLACEMENT_3D('',#48436,#22291,#22292);
#18963=AXIS2_PLACEMENT_3D('',#48437,#22293,#22294);
#18964=AXIS2_PLACEMENT_3D('',#48438,#22295,#22296);
#18965=AXIS2_PLACEMENT_3D('',#48439,#22297,#22298);
#18966=AXIS2_PLACEMENT_3D('',#48440,#22299,#22300);
#18967=AXIS2_PLACEMENT_3D('',#48441,#22301,#22302);
#18968=AXIS2_PLACEMENT_3D('',#48442,#22303,#22304);
#18969=AXIS2_PLACEMENT_3D('',#48443,#22305,#22306);
#18970=AXIS2_PLACEMENT_3D('',#48444,#22307,#22308);
#18971=AXIS2_PLACEMENT_3D('',#48445,#22309,#22310);
#18972=AXIS2_PLACEMENT_3D('',#48446,#22311,#22312);
#18973=AXIS2_PLACEMENT_3D('',#48447,#22313,#22314);
#18974=AXIS2_PLACEMENT_3D('',#48448,#22315,#22316);
#18975=AXIS2_PLACEMENT_3D('',#48449,#22317,#22318);
#18976=AXIS2_PLACEMENT_3D('',#48450,#22319,#22320);
#18977=AXIS2_PLACEMENT_3D('',#48451,#22321,#22322);
#18978=AXIS2_PLACEMENT_3D('',#48452,#22323,#22324);
#18979=AXIS2_PLACEMENT_3D('',#48453,#22325,#22326);
#18980=AXIS2_PLACEMENT_3D('',#48454,#22327,#22328);
#18981=AXIS2_PLACEMENT_3D('',#48455,#22329,#22330);
#18982=AXIS2_PLACEMENT_3D('',#48456,#22331,#22332);
#18983=AXIS2_PLACEMENT_3D('',#48457,#22333,#22334);
#18984=AXIS2_PLACEMENT_3D('',#48458,#22335,#22336);
#18985=AXIS2_PLACEMENT_3D('',#48459,#22337,#22338);
#18986=AXIS2_PLACEMENT_3D('',#48460,#22339,#22340);
#18987=AXIS2_PLACEMENT_3D('',#48461,#22341,#22342);
#18988=AXIS2_PLACEMENT_3D('',#48462,#22343,#22344);
#18989=AXIS2_PLACEMENT_3D('',#48463,#22345,#22346);
#18990=AXIS2_PLACEMENT_3D('',#48464,#22347,#22348);
#18991=AXIS2_PLACEMENT_3D('',#48465,#22349,#22350);
#18992=AXIS2_PLACEMENT_3D('',#48466,#22351,#22352);
#18993=AXIS2_PLACEMENT_3D('',#48467,#22353,#22354);
#18994=AXIS2_PLACEMENT_3D('',#48468,#22355,#22356);
#18995=AXIS2_PLACEMENT_3D('',#48469,#22357,#22358);
#18996=AXIS2_PLACEMENT_3D('',#48470,#22359,#22360);
#18997=AXIS2_PLACEMENT_3D('',#48471,#22361,#22362);
#18998=AXIS2_PLACEMENT_3D('',#48472,#22363,#22364);
#18999=AXIS2_PLACEMENT_3D('',#48473,#22365,#22366);
#19000=AXIS2_PLACEMENT_3D('',#48474,#22367,#22368);
#19001=AXIS2_PLACEMENT_3D('',#48475,#22369,#22370);
#19002=AXIS2_PLACEMENT_3D('',#48476,#22371,#22372);
#19003=AXIS2_PLACEMENT_3D('',#48477,#22373,#22374);
#19004=AXIS2_PLACEMENT_3D('',#48478,#22375,#22376);
#19005=AXIS2_PLACEMENT_3D('',#48479,#22377,#22378);
#19006=AXIS2_PLACEMENT_3D('',#48480,#22379,#22380);
#19007=AXIS2_PLACEMENT_3D('',#48481,#22381,#22382);
#19008=AXIS2_PLACEMENT_3D('',#48482,#22383,#22384);
#19009=AXIS2_PLACEMENT_3D('',#48483,#22385,#22386);
#19010=AXIS2_PLACEMENT_3D('',#48484,#22387,#22388);
#19011=AXIS2_PLACEMENT_3D('',#48485,#22389,#22390);
#19012=AXIS2_PLACEMENT_3D('',#48486,#22391,#22392);
#19013=AXIS2_PLACEMENT_3D('',#48487,#22393,#22394);
#19014=AXIS2_PLACEMENT_3D('',#48488,#22395,#22396);
#19015=AXIS2_PLACEMENT_3D('',#48489,#22397,#22398);
#19016=AXIS2_PLACEMENT_3D('',#48490,#22399,#22400);
#19017=AXIS2_PLACEMENT_3D('',#48491,#22401,#22402);
#19018=AXIS2_PLACEMENT_3D('',#48492,#22403,#22404);
#19019=AXIS2_PLACEMENT_3D('',#48493,#22405,#22406);
#19020=AXIS2_PLACEMENT_3D('',#48494,#22407,#22408);
#19021=AXIS2_PLACEMENT_3D('',#48495,#22409,#22410);
#19022=AXIS2_PLACEMENT_3D('',#48496,#22411,#22412);
#19023=AXIS2_PLACEMENT_3D('',#48497,#22413,#22414);
#19024=AXIS2_PLACEMENT_3D('',#48498,#22415,#22416);
#19025=AXIS2_PLACEMENT_3D('',#48499,#22417,#22418);
#19026=AXIS2_PLACEMENT_3D('',#48500,#22419,#22420);
#19027=AXIS2_PLACEMENT_3D('',#48501,#22421,#22422);
#19028=AXIS2_PLACEMENT_3D('',#48502,#22423,#22424);
#19029=AXIS2_PLACEMENT_3D('',#48503,#22425,#22426);
#19030=AXIS2_PLACEMENT_3D('',#48504,#22427,#22428);
#19031=AXIS2_PLACEMENT_3D('',#48505,#22429,#22430);
#19032=AXIS2_PLACEMENT_3D('',#48506,#22431,#22432);
#19033=AXIS2_PLACEMENT_3D('',#48507,#22433,#22434);
#19034=AXIS2_PLACEMENT_3D('',#48508,#22435,#22436);
#19035=AXIS2_PLACEMENT_3D('',#48509,#22437,#22438);
#19036=AXIS2_PLACEMENT_3D('',#48510,#22439,#22440);
#19037=AXIS2_PLACEMENT_3D('',#48511,#22441,#22442);
#19038=AXIS2_PLACEMENT_3D('',#48512,#22443,#22444);
#19039=AXIS2_PLACEMENT_3D('',#48513,#22445,#22446);
#19040=AXIS2_PLACEMENT_3D('',#48514,#22447,#22448);
#19041=AXIS2_PLACEMENT_3D('',#48515,#22449,#22450);
#19042=AXIS2_PLACEMENT_3D('',#48516,#22451,#22452);
#19043=AXIS2_PLACEMENT_3D('',#48517,#22453,#22454);
#19044=AXIS2_PLACEMENT_3D('',#48518,#22455,#22456);
#19045=AXIS2_PLACEMENT_3D('',#48519,#22457,#22458);
#19046=AXIS2_PLACEMENT_3D('',#48520,#22459,#22460);
#19047=AXIS2_PLACEMENT_3D('',#48521,#22461,#22462);
#19048=AXIS2_PLACEMENT_3D('',#48522,#22463,#22464);
#19049=AXIS2_PLACEMENT_3D('',#48523,#22465,#22466);
#19050=AXIS2_PLACEMENT_3D('',#48525,#22467,#22468);
#19051=AXIS2_PLACEMENT_3D('',#48528,#22470,#22471);
#19052=AXIS2_PLACEMENT_3D('',#48529,#22472,#22473);
#19053=AXIS2_PLACEMENT_3D('',#48530,#22474,#22475);
#19054=AXIS2_PLACEMENT_3D('',#48533,#22476,#22477);
#19055=AXIS2_PLACEMENT_3D('',#48537,#22479,#22480);
#19056=AXIS2_PLACEMENT_3D('',#48539,#22482,#22483);
#19057=AXIS2_PLACEMENT_3D('',#48545,#22487,#22488);
#19058=AXIS2_PLACEMENT_3D('',#48547,#22489,#22490);
#19059=AXIS2_PLACEMENT_3D('',#48550,#22492,#22493);
#19060=AXIS2_PLACEMENT_3D('',#48551,#22494,#22495);
#19061=AXIS2_PLACEMENT_3D('',#48554,#22498,#22499);
#19062=AXIS2_PLACEMENT_3D('',#48555,#22500,#22501);
#19063=AXIS2_PLACEMENT_3D('',#48556,#22502,#22503);
#19064=AXIS2_PLACEMENT_3D('',#48557,#22504,#22505);
#19065=AXIS2_PLACEMENT_3D('',#48559,#22506,#22507);
#19066=AXIS2_PLACEMENT_3D('',#48561,#22508,#22509);
#19067=AXIS2_PLACEMENT_3D('',#48562,#22510,#22511);
#19068=AXIS2_PLACEMENT_3D('',#48565,#22512,#22513);
#19069=AXIS2_PLACEMENT_3D('',#48566,#22514,#22515);
#19070=AXIS2_PLACEMENT_3D('',#48569,#22517,#22518);
#19071=AXIS2_PLACEMENT_3D('',#48570,#22519,#22520);
#19072=AXIS2_PLACEMENT_3D('',#48572,#22521,#22522);
#19073=AXIS2_PLACEMENT_3D('',#48574,#22523,#22524);
#19074=AXIS2_PLACEMENT_3D('',#48575,#22525,#22526);
#19075=AXIS2_PLACEMENT_3D('',#48577,#22528,#22529);
#19076=AXIS2_PLACEMENT_3D('',#48578,#22530,#22531);
#19077=AXIS2_PLACEMENT_3D('',#48579,#22532,#22533);
#19078=AXIS2_PLACEMENT_3D('',#48580,#22534,#22535);
#19079=AXIS2_PLACEMENT_3D('',#48581,#22536,#22537);
#19080=AXIS2_PLACEMENT_3D('',#48582,#22538,#22539);
#19081=AXIS2_PLACEMENT_3D('',#48585,#22540,#22541);
#19082=AXIS2_PLACEMENT_3D('',#48587,#22542,#22543);
#19083=AXIS2_PLACEMENT_3D('',#48589,#22544,#22545);
#19084=AXIS2_PLACEMENT_3D('',#48591,#22546,#22547);
#19085=AXIS2_PLACEMENT_3D('',#48593,#22548,#22549);
#19086=AXIS2_PLACEMENT_3D('',#48595,#22550,#22551);
#19087=AXIS2_PLACEMENT_3D('',#48597,#22552,#22553);
#19088=AXIS2_PLACEMENT_3D('',#48599,#22554,#22555);
#19089=AXIS2_PLACEMENT_3D('',#48601,#22556,#22557);
#19090=AXIS2_PLACEMENT_3D('',#48603,#22558,#22559);
#19091=AXIS2_PLACEMENT_3D('',#48605,#22560,#22561);
#19092=AXIS2_PLACEMENT_3D('',#48607,#22562,#22563);
#19093=AXIS2_PLACEMENT_3D('',#48609,#22564,#22565);
#19094=AXIS2_PLACEMENT_3D('',#48611,#22566,#22567);
#19095=AXIS2_PLACEMENT_3D('',#48612,#22568,#22569);
#19096=AXIS2_PLACEMENT_3D('',#48614,#22570,#22571);
#19097=AXIS2_PLACEMENT_3D('',#48616,#22572,#22573);
#19098=AXIS2_PLACEMENT_3D('',#48618,#22574,#22575);
#19099=AXIS2_PLACEMENT_3D('',#48620,#22576,#22577);
#19100=AXIS2_PLACEMENT_3D('',#48622,#22578,#22579);
#19101=AXIS2_PLACEMENT_3D('',#48624,#22580,#22581);
#19102=AXIS2_PLACEMENT_3D('',#48626,#22582,#22583);
#19103=AXIS2_PLACEMENT_3D('',#48628,#22584,#22585);
#19104=AXIS2_PLACEMENT_3D('',#48629,#22586,#22587);
#19105=AXIS2_PLACEMENT_3D('',#48630,#22588,#22589);
#19106=AXIS2_PLACEMENT_3D('',#48632,#22590,#22591);
#19107=AXIS2_PLACEMENT_3D('',#48634,#22592,#22593);
#19108=AXIS2_PLACEMENT_3D('',#48635,#22594,#22595);
#19109=AXIS2_PLACEMENT_3D('',#48637,#22597,#22598);
#19110=AXIS2_PLACEMENT_3D('',#48639,#22599,#22600);
#19111=AXIS2_PLACEMENT_3D('',#48640,#22601,#22602);
#19112=AXIS2_PLACEMENT_3D('',#48642,#22603,#22604);
#19113=AXIS2_PLACEMENT_3D('',#48645,#22606,#22607);
#19114=AXIS2_PLACEMENT_3D('',#48646,#22608,#22609);
#19115=AXIS2_PLACEMENT_3D('',#48648,#22611,#22612);
#19116=AXIS2_PLACEMENT_3D('',#48654,#22616,#22617);
#19117=AXIS2_PLACEMENT_3D('',#48658,#22620,#22621);
#19118=AXIS2_PLACEMENT_3D('',#48662,#22624,#22625);
#19119=AXIS2_PLACEMENT_3D('',#48666,#22628,#22629);
#19120=AXIS2_PLACEMENT_3D('',#48670,#22632,#22633);
#19121=AXIS2_PLACEMENT_3D('',#48674,#22636,#22637);
#19122=AXIS2_PLACEMENT_3D('',#48678,#22640,#22641);
#19123=AXIS2_PLACEMENT_3D('',#48682,#22644,#22645);
#19124=AXIS2_PLACEMENT_3D('',#48686,#22648,#22649);
#19125=AXIS2_PLACEMENT_3D('',#48690,#22652,#22653);
#19126=AXIS2_PLACEMENT_3D('',#48694,#22656,#22657);
#19127=AXIS2_PLACEMENT_3D('',#48698,#22660,#22661);
#19128=AXIS2_PLACEMENT_3D('',#48702,#22664,#22665);
#19129=AXIS2_PLACEMENT_3D('',#48706,#22668,#22669);
#19130=AXIS2_PLACEMENT_3D('',#48710,#22672,#22673);
#19131=AXIS2_PLACEMENT_3D('',#48714,#22676,#22677);
#19132=AXIS2_PLACEMENT_3D('',#48718,#22680,#22681);
#19133=AXIS2_PLACEMENT_3D('',#48722,#22684,#22685);
#19134=AXIS2_PLACEMENT_3D('',#48726,#22688,#22689);
#19135=AXIS2_PLACEMENT_3D('',#48728,#22691,#22692);
#19136=AXIS2_PLACEMENT_3D('',#48729,#22693,#22694);
#19137=AXIS2_PLACEMENT_3D('',#48730,#22695,#22696);
#19138=AXIS2_PLACEMENT_3D('',#48731,#22697,#22698);
#19139=AXIS2_PLACEMENT_3D('',#48732,#22699,#22700);
#19140=AXIS2_PLACEMENT_3D('',#48737,#22702,#22703);
#19141=AXIS2_PLACEMENT_3D('',#48740,#22705,#22706);
#19142=AXIS2_PLACEMENT_3D('',#48741,#22707,#22708);
#19143=AXIS2_PLACEMENT_3D('',#48742,#22709,#22710);
#19144=AXIS2_PLACEMENT_3D('',#48743,#22711,#22712);
#19145=AXIS2_PLACEMENT_3D('',#48744,#22713,#22714);
#19146=AXIS2_PLACEMENT_3D('',#48747,#22715,#22716);
#19147=AXIS2_PLACEMENT_3D('',#48748,#22717,#22718);
#19148=AXIS2_PLACEMENT_3D('',#48750,#22719,#22720);
#19149=AXIS2_PLACEMENT_3D('',#48752,#22721,#22722);
#19150=AXIS2_PLACEMENT_3D('',#48754,#22723,#22724);
#19151=AXIS2_PLACEMENT_3D('',#48756,#22725,#22726);
#19152=AXIS2_PLACEMENT_3D('',#48757,#22727,#22728);
#19153=AXIS2_PLACEMENT_3D('',#48760,#22729,#22730);
#19154=AXIS2_PLACEMENT_3D('',#48761,#22731,#22732);
#19155=AXIS2_PLACEMENT_3D('',#48763,#22733,#22734);
#19156=AXIS2_PLACEMENT_3D('',#48765,#22735,#22736);
#19157=AXIS2_PLACEMENT_3D('',#48767,#22737,#22738);
#19158=AXIS2_PLACEMENT_3D('',#48769,#22739,#22740);
#19159=AXIS2_PLACEMENT_3D('',#48770,#22741,#22742);
#19160=AXIS2_PLACEMENT_3D('',#48773,#22743,#22744);
#19161=AXIS2_PLACEMENT_3D('',#48774,#22745,#22746);
#19162=AXIS2_PLACEMENT_3D('',#48778,#22748,#22749);
#19163=AXIS2_PLACEMENT_3D('',#48779,#22750,#22751);
#19164=AXIS2_PLACEMENT_3D('',#48780,#22752,#22753);
#19165=AXIS2_PLACEMENT_3D('',#48783,#22754,#22755);
#19166=AXIS2_PLACEMENT_3D('',#48784,#22756,#22757);
#19167=AXIS2_PLACEMENT_3D('',#48788,#22759,#22760);
#19168=AXIS2_PLACEMENT_3D('',#48789,#22761,#22762);
#19169=AXIS2_PLACEMENT_3D('',#48790,#22763,#22764);
#19170=AXIS2_PLACEMENT_3D('',#48793,#22765,#22766);
#19171=AXIS2_PLACEMENT_3D('',#48794,#22767,#22768);
#19172=AXIS2_PLACEMENT_3D('',#48798,#22770,#22771);
#19173=AXIS2_PLACEMENT_3D('',#48799,#22772,#22773);
#19174=AXIS2_PLACEMENT_3D('',#48800,#22774,#22775);
#19175=AXIS2_PLACEMENT_3D('',#48803,#22776,#22777);
#19176=AXIS2_PLACEMENT_3D('',#48804,#22778,#22779);
#19177=AXIS2_PLACEMENT_3D('',#48808,#22781,#22782);
#19178=AXIS2_PLACEMENT_3D('',#48809,#22783,#22784);
#19179=AXIS2_PLACEMENT_3D('',#48810,#22785,#22786);
#19180=AXIS2_PLACEMENT_3D('',#48839,#22787,#22788);
#19181=AXIS2_PLACEMENT_3D('',#48840,#22789,#22790);
#19182=AXIS2_PLACEMENT_3D('',#48841,#22791,#22792);
#19183=AXIS2_PLACEMENT_3D('',#48842,#22793,#22794);
#19184=AXIS2_PLACEMENT_3D('',#48843,#22795,#22796);
#19185=AXIS2_PLACEMENT_3D('',#48844,#22797,#22798);
#19186=AXIS2_PLACEMENT_3D('',#48845,#22799,#22800);
#19187=AXIS2_PLACEMENT_3D('',#48846,#22801,#22802);
#19188=AXIS2_PLACEMENT_3D('',#48847,#22803,#22804);
#19189=AXIS2_PLACEMENT_3D('',#48848,#22805,#22806);
#19190=AXIS2_PLACEMENT_3D('',#48877,#22807,#22808);
#19191=AXIS2_PLACEMENT_3D('',#48878,#22809,#22810);
#19192=AXIS2_PLACEMENT_3D('',#48879,#22811,#22812);
#19193=AXIS2_PLACEMENT_3D('',#48880,#22813,#22814);
#19194=AXIS2_PLACEMENT_3D('',#48881,#22815,#22816);
#19195=AXIS2_PLACEMENT_3D('',#48882,#22817,#22818);
#19196=AXIS2_PLACEMENT_3D('',#48883,#22819,#22820);
#19197=AXIS2_PLACEMENT_3D('',#48884,#22821,#22822);
#19198=AXIS2_PLACEMENT_3D('',#48885,#22823,#22824);
#19199=AXIS2_PLACEMENT_3D('',#48886,#22825,#22826);
#19200=AXIS2_PLACEMENT_3D('',#48887,#22827,#22828);
#19201=AXIS2_PLACEMENT_3D('',#48892,#22830,#22831);
#19202=AXIS2_PLACEMENT_3D('',#48895,#22833,#22834);
#19203=AXIS2_PLACEMENT_3D('',#48896,#22835,#22836);
#19204=AXIS2_PLACEMENT_3D('',#48905,#22841,#22842);
#19205=AXIS2_PLACEMENT_3D('',#48914,#22847,#22848);
#19206=AXIS2_PLACEMENT_3D('',#48916,#22849,#22850);
#19207=AXIS2_PLACEMENT_3D('',#48919,#22852,#22853);
#19208=AXIS2_PLACEMENT_3D('',#48920,#22854,#22855);
#19209=AXIS2_PLACEMENT_3D('',#48926,#22859,#22860);
#19210=AXIS2_PLACEMENT_3D('',#48935,#22865,#22866);
#19211=AXIS2_PLACEMENT_3D('',#48940,#22868,#22869);
#19212=AXIS2_PLACEMENT_3D('',#48943,#22871,#22872);
#19213=AXIS2_PLACEMENT_3D('',#48944,#22873,#22874);
#19214=AXIS2_PLACEMENT_3D('',#48945,#22875,#22876);
#19215=AXIS2_PLACEMENT_3D('',#48946,#22877,#22878);
#19216=AXIS2_PLACEMENT_3D('',#48947,#22879,#22880);
#19217=AXIS2_PLACEMENT_3D('',#48966,#22881,#22882);
#19218=AXIS2_PLACEMENT_3D('',#48968,#22883,#22884);
#19219=AXIS2_PLACEMENT_3D('',#48970,#22885,#22886);
#19220=AXIS2_PLACEMENT_3D('',#48976,#22889,#22890);
#19221=AXIS2_PLACEMENT_3D('',#48981,#22893,#22894);
#19222=AXIS2_PLACEMENT_3D('',#48982,#22895,#22896);
#19223=AXIS2_PLACEMENT_3D('',#49005,#22899,#22900);
#19224=AXIS2_PLACEMENT_3D('',#49007,#22901,#22902);
#19225=AXIS2_PLACEMENT_3D('',#49009,#22903,#22904);
#19226=AXIS2_PLACEMENT_3D('',#49014,#22907,#22908);
#19227=AXIS2_PLACEMENT_3D('',#49016,#22909,#22910);
#19228=AXIS2_PLACEMENT_3D('',#49017,#22911,#22912);
#19229=AXIS2_PLACEMENT_3D('',#49020,#22913,#22914);
#19230=AXIS2_PLACEMENT_3D('',#49021,#22915,#22916);
#19231=AXIS2_PLACEMENT_3D('',#49025,#22918,#22919);
#19232=AXIS2_PLACEMENT_3D('',#49026,#22920,#22921);
#19233=AXIS2_PLACEMENT_3D('',#49027,#22922,#22923);
#19234=AXIS2_PLACEMENT_3D('',#49028,#22924,#22925);
#19235=AXIS2_PLACEMENT_3D('',#49029,#22926,#22927);
#19236=AXIS2_PLACEMENT_3D('',#49030,#22928,#22929);
#19237=AXIS2_PLACEMENT_3D('',#49038,#22930,#22931);
#19238=AXIS2_PLACEMENT_3D('',#49039,#22932,#22933);
#19239=AXIS2_PLACEMENT_3D('',#49040,#22934,#22935);
#19240=AXIS2_PLACEMENT_3D('',#49041,#22936,#22937);
#19241=AXIS2_PLACEMENT_3D('',#49042,#22938,#22939);
#19242=AXIS2_PLACEMENT_3D('',#49043,#22940,#22941);
#19243=AXIS2_PLACEMENT_3D('',#49044,#22942,#22943);
#19244=AXIS2_PLACEMENT_3D('',#49052,#22944,#22945);
#19245=AXIS2_PLACEMENT_3D('',#49053,#22946,#22947);
#19246=AXIS2_PLACEMENT_3D('',#49054,#22948,#22949);
#19247=AXIS2_PLACEMENT_3D('',#49055,#22950,#22951);
#19248=AXIS2_PLACEMENT_3D('',#49056,#22952,#22953);
#19249=AXIS2_PLACEMENT_3D('',#49057,#22954,#22955);
#19250=AXIS2_PLACEMENT_3D('',#49058,#22956,#22957);
#19251=AXIS2_PLACEMENT_3D('',#49059,#22958,#22959);
#19252=AXIS2_PLACEMENT_3D('',#49067,#22960,#22961);
#19253=AXIS2_PLACEMENT_3D('',#49068,#22962,#22963);
#19254=AXIS2_PLACEMENT_3D('',#49069,#22964,#22965);
#19255=AXIS2_PLACEMENT_3D('',#49070,#22966,#22967);
#19256=AXIS2_PLACEMENT_3D('',#49071,#22968,#22969);
#19257=AXIS2_PLACEMENT_3D('',#49072,#22970,#22971);
#19258=AXIS2_PLACEMENT_3D('',#49073,#22972,#22973);
#19259=AXIS2_PLACEMENT_3D('',#49081,#22974,#22975);
#19260=AXIS2_PLACEMENT_3D('',#49089,#22976,#22977);
#19261=AXIS2_PLACEMENT_3D('',#49090,#22978,#22979);
#19262=AXIS2_PLACEMENT_3D('',#49092,#22980,#22981);
#19263=AXIS2_PLACEMENT_3D('',#49093,#22982,#22983);
#19264=AXIS2_PLACEMENT_3D('',#49094,#22984,#22985);
#19265=AXIS2_PLACEMENT_3D('',#49095,#22986,#22987);
#19266=AXIS2_PLACEMENT_3D('',#49096,#22988,#22989);
#19267=AXIS2_PLACEMENT_3D('',#49097,#22990,#22991);
#19268=AXIS2_PLACEMENT_3D('',#49098,#22992,#22993);
#19269=AXIS2_PLACEMENT_3D('',#49099,#22994,#22995);
#19270=AXIS2_PLACEMENT_3D('',#49100,#22996,#22997);
#19271=AXIS2_PLACEMENT_3D('',#49102,#22998,#22999);
#19272=AXIS2_PLACEMENT_3D('',#49103,#23000,#23001);
#19273=AXIS2_PLACEMENT_3D('',#49104,#23002,#23003);
#19274=AXIS2_PLACEMENT_3D('',#49105,#23004,#23005);
#19275=AXIS2_PLACEMENT_3D('',#49106,#23006,#23007);
#19276=AXIS2_PLACEMENT_3D('',#49107,#23008,#23009);
#19277=AXIS2_PLACEMENT_3D('',#49108,#23010,#23011);
#19278=AXIS2_PLACEMENT_3D('',#49116,#23012,#23013);
#19279=AXIS2_PLACEMENT_3D('',#49117,#23014,#23015);
#19280=AXIS2_PLACEMENT_3D('',#49118,#23016,#23017);
#19281=AXIS2_PLACEMENT_3D('',#49119,#23018,#23019);
#19282=AXIS2_PLACEMENT_3D('',#49120,#23020,#23021);
#19283=AXIS2_PLACEMENT_3D('',#49121,#23022,#23023);
#19284=AXIS2_PLACEMENT_3D('',#49122,#23024,#23025);
#19285=AXIS2_PLACEMENT_3D('',#49123,#23026,#23027);
#19286=AXIS2_PLACEMENT_3D('',#49124,#23028,#23029);
#19287=AXIS2_PLACEMENT_3D('',#49125,#23030,#23031);
#19288=AXIS2_PLACEMENT_3D('',#49126,#23032,#23033);
#19289=AXIS2_PLACEMENT_3D('',#49127,#23034,#23035);
#19290=AXIS2_PLACEMENT_3D('',#49128,#23036,#23037);
#19291=AXIS2_PLACEMENT_3D('',#49129,#23038,#23039);
#19292=AXIS2_PLACEMENT_3D('',#49130,#23040,#23041);
#19293=AXIS2_PLACEMENT_3D('',#49131,#23042,#23043);
#19294=AXIS2_PLACEMENT_3D('',#49597,#23044,#23045);
#19295=AXIS2_PLACEMENT_3D('',#49607,#23047,#23048);
#19296=AXIS2_PLACEMENT_3D('',#49611,#23050,#23051);
#19297=AXIS2_PLACEMENT_3D('',#49612,#23052,#23053);
#19298=AXIS2_PLACEMENT_3D('',#49613,#23054,#23055);
#19299=AXIS2_PLACEMENT_3D('',#49615,#23056,#23057);
#19300=AXIS2_PLACEMENT_3D('',#49618,#23059,#23060);
#19301=AXIS2_PLACEMENT_3D('',#49619,#23061,#23062);
#19302=AXIS2_PLACEMENT_3D('',#49622,#23063,#23064);
#19303=AXIS2_PLACEMENT_3D('',#49626,#23066,#23067);
#19304=AXIS2_PLACEMENT_3D('',#49628,#23069,#23070);
#19305=AXIS2_PLACEMENT_3D('',#49633,#23072,#23073);
#19306=AXIS2_PLACEMENT_3D('',#49636,#23075,#23076);
#19307=AXIS2_PLACEMENT_3D('',#49637,#23077,#23078);
#19308=AXIS2_PLACEMENT_3D('',#49640,#23079,#23080);
#19309=AXIS2_PLACEMENT_3D('',#49642,#23081,#23082);
#19310=AXIS2_PLACEMENT_3D('',#49644,#23083,#23084);
#19311=AXIS2_PLACEMENT_3D('',#49646,#23085,#23086);
#19312=AXIS2_PLACEMENT_3D('',#49648,#23087,#23088);
#19313=AXIS2_PLACEMENT_3D('',#49650,#23089,#23090);
#19314=AXIS2_PLACEMENT_3D('',#49652,#23091,#23092);
#19315=AXIS2_PLACEMENT_3D('',#49654,#23093,#23094);
#19316=AXIS2_PLACEMENT_3D('',#49656,#23095,#23096);
#19317=AXIS2_PLACEMENT_3D('',#49657,#23097,#23098);
#19318=AXIS2_PLACEMENT_3D('',#49659,#23099,#23100);
#19319=AXIS2_PLACEMENT_3D('',#49661,#23101,#23102);
#19320=AXIS2_PLACEMENT_3D('',#49663,#23103,#23104);
#19321=AXIS2_PLACEMENT_3D('',#49665,#23105,#23106);
#19322=AXIS2_PLACEMENT_3D('',#49666,#23107,#23108);
#19323=AXIS2_PLACEMENT_3D('',#49677,#23110,#23111);
#19324=AXIS2_PLACEMENT_3D('',#49690,#23113,#23114);
#19325=AXIS2_PLACEMENT_3D('',#49693,#23115,#23116);
#19326=AXIS2_PLACEMENT_3D('',#49697,#23118,#23119);
#19327=AXIS2_PLACEMENT_3D('',#49699,#23121,#23122);
#19328=AXIS2_PLACEMENT_3D('',#49716,#23123,#23124);
#19329=AXIS2_PLACEMENT_3D('',#49718,#23125,#23126);
#19330=AXIS2_PLACEMENT_3D('',#49734,#23127,#23128);
#19331=AXIS2_PLACEMENT_3D('',#49738,#23130,#23131);
#19332=AXIS2_PLACEMENT_3D('',#49739,#23132,#23133);
#19333=AXIS2_PLACEMENT_3D('',#49740,#23134,#23135);
#19334=AXIS2_PLACEMENT_3D('',#49761,#23136,#23137);
#19335=AXIS2_PLACEMENT_3D('',#49766,#23139,#23140);
#19336=AXIS2_PLACEMENT_3D('',#49769,#23142,#23143);
#19337=AXIS2_PLACEMENT_3D('',#49770,#23144,#23145);
#19338=AXIS2_PLACEMENT_3D('',#49776,#23149,#23150);
#19339=AXIS2_PLACEMENT_3D('',#49781,#23152,#23153);
#19340=AXIS2_PLACEMENT_3D('',#49784,#23155,#23156);
#19341=AXIS2_PLACEMENT_3D('',#49785,#23157,#23158);
#19342=AXIS2_PLACEMENT_3D('',#49791,#23162,#23163);
#19343=AXIS2_PLACEMENT_3D('',#49792,#23164,#23165);
#19344=AXIS2_PLACEMENT_3D('',#49793,#23166,#23167);
#19345=AXIS2_PLACEMENT_3D('',#49794,#23168,#23169);
#19346=AXIS2_PLACEMENT_3D('',#49799,#23171,#23172);
#19347=AXIS2_PLACEMENT_3D('',#49805,#23175,#23176);
#19348=AXIS2_PLACEMENT_3D('',#49809,#23178,#23179);
#19349=AXIS2_PLACEMENT_3D('',#49813,#23181,#23182);
#19350=AXIS2_PLACEMENT_3D('',#49816,#23184,#23185);
#19351=AXIS2_PLACEMENT_3D('',#49818,#23186,#23187);
#19352=AXIS2_PLACEMENT_3D('',#49820,#23188,#23189);
#19353=AXIS2_PLACEMENT_3D('',#49821,#23190,#23191);
#19354=AXIS2_PLACEMENT_3D('',#49839,#23193,#23194);
#19355=AXIS2_PLACEMENT_3D('',#49843,#23196,#23197);
#19356=AXIS2_PLACEMENT_3D('',#49847,#23199,#23200);
#19357=AXIS2_PLACEMENT_3D('',#49878,#23202,#23203);
#19358=AXIS2_PLACEMENT_3D('',#49879,#23204,#23205);
#19359=AXIS2_PLACEMENT_3D('',#49880,#23206,#23207);
#19360=AXIS2_PLACEMENT_3D('',#49885,#23209,#23210);
#19361=AXIS2_PLACEMENT_3D('',#49888,#23212,#23213);
#19362=AXIS2_PLACEMENT_3D('',#49889,#23214,#23215);
#19363=AXIS2_PLACEMENT_3D('',#49890,#23216,#23217);
#19364=AXIS2_PLACEMENT_3D('',#49891,#23218,#23219);
#19365=AXIS2_PLACEMENT_3D('',#49892,#23220,#23221);
#19366=AXIS2_PLACEMENT_3D('',#49895,#23222,#23223);
#19367=AXIS2_PLACEMENT_3D('',#49897,#23224,#23225);
#19368=AXIS2_PLACEMENT_3D('',#49899,#23226,#23227);
#19369=AXIS2_PLACEMENT_3D('',#49901,#23228,#23229);
#19370=AXIS2_PLACEMENT_3D('',#49903,#23230,#23231);
#19371=AXIS2_PLACEMENT_3D('',#49905,#23232,#23233);
#19372=AXIS2_PLACEMENT_3D('',#49906,#23234,#23235);
#19373=AXIS2_PLACEMENT_3D('',#49908,#23236,#23237);
#19374=AXIS2_PLACEMENT_3D('',#49910,#23238,#23239);
#19375=AXIS2_PLACEMENT_3D('',#49912,#23240,#23241);
#19376=AXIS2_PLACEMENT_3D('',#49913,#23242,#23243);
#19377=AXIS2_PLACEMENT_3D('',#49914,#23244,#23245);
#19378=AXIS2_PLACEMENT_3D('',#49916,#23246,#23247);
#19379=AXIS2_PLACEMENT_3D('',#49918,#23248,#23249);
#19380=AXIS2_PLACEMENT_3D('',#49919,#23250,#23251);
#19381=AXIS2_PLACEMENT_3D('',#49922,#23252,#23253);
#19382=AXIS2_PLACEMENT_3D('',#49923,#23254,#23255);
#19383=AXIS2_PLACEMENT_3D('',#49927,#23257,#23258);
#19384=AXIS2_PLACEMENT_3D('',#49928,#23259,#23260);
#19385=AXIS2_PLACEMENT_3D('',#49929,#23261,#23262);
#19386=AXIS2_PLACEMENT_3D('',#49988,#23268,#23269);
#19387=AXIS2_PLACEMENT_3D('',#49989,#23270,#23271);
#19388=AXIS2_PLACEMENT_3D('',#50038,#23275,#23276);
#19389=AXIS2_PLACEMENT_3D('',#51349,#23281,#23282);
#19390=AXIS2_PLACEMENT_3D('',#51351,#23283,#23284);
#19391=AXIS2_PLACEMENT_3D('',#51352,#23285,#23286);
#19392=AXIS2_PLACEMENT_3D('',#51357,#23287,#23288);
#19393=AXIS2_PLACEMENT_3D('',#51362,#23289,#23290);
#19394=AXIS2_PLACEMENT_3D('',#51367,#23291,#23292);
#19395=AXIS2_PLACEMENT_3D('',#51372,#23293,#23294);
#19396=AXIS2_PLACEMENT_3D('',#51377,#23295,#23296);
#19397=AXIS2_PLACEMENT_3D('',#51380,#23297,#23298);
#19398=AXIS2_PLACEMENT_3D('',#51384,#23300,#23301);
#19399=AXIS2_PLACEMENT_3D('',#51386,#23303,#23304);
#19400=AXIS2_PLACEMENT_3D('',#51389,#23306,#23307);
#19401=AXIS2_PLACEMENT_3D('',#51390,#23308,#23309);
#19402=AXIS2_PLACEMENT_3D('',#51392,#23310,#23311);
#19403=AXIS2_PLACEMENT_3D('',#51394,#23313,#23314);
#19404=AXIS2_PLACEMENT_3D('',#51533,#23317,#23318);
#19405=AXIS2_PLACEMENT_3D('',#51543,#23321,#23322);
#19406=AXIS2_PLACEMENT_3D('',#51545,#23323,#23324);
#19407=AXIS2_PLACEMENT_3D('',#51547,#23325,#23326);
#19408=AXIS2_PLACEMENT_3D('',#51548,#23327,#23328);
#19409=AXIS2_PLACEMENT_3D('',#51553,#23330,#23331);
#19410=AXIS2_PLACEMENT_3D('',#51556,#23333,#23334);
#19411=AXIS2_PLACEMENT_3D('',#51557,#23335,#23336);
#19412=AXIS2_PLACEMENT_3D('',#51563,#23340,#23341);
#19413=AXIS2_PLACEMENT_3D('',#51723,#23345,#23346);
#19414=AXIS2_PLACEMENT_3D('',#51958,#23347,#23348);
#19415=AXIS2_PLACEMENT_3D('',#52649,#23349,#23350);
#19416=AXIS2_PLACEMENT_3D('',#52691,#23351,#23352);
#19417=AXIS2_PLACEMENT_3D('',#53230,#23353,#23354);
#19418=AXIS2_PLACEMENT_3D('',#53342,#23355,#23356);
#19419=AXIS2_PLACEMENT_3D('',#53450,#23357,#23358);
#19420=AXIS2_PLACEMENT_3D('',#53451,#23359,#23360);
#19421=AXIS2_PLACEMENT_3D('',#53575,#23361,#23362);
#19422=AXIS2_PLACEMENT_3D('',#53576,#23363,#23364);
#19423=AXIS2_PLACEMENT_3D('',#53577,#23365,#23366);
#19424=AXIS2_PLACEMENT_3D('',#53578,#23367,#23368);
#19425=AXIS2_PLACEMENT_3D('',#53579,#23369,#23370);
#19426=AXIS2_PLACEMENT_3D('',#53580,#23371,#23372);
#19427=AXIS2_PLACEMENT_3D('',#53581,#23373,#23374);
#19428=AXIS2_PLACEMENT_3D('',#53582,#23375,#23376);
#19429=AXIS2_PLACEMENT_3D('',#53583,#23377,#23378);
#19430=AXIS2_PLACEMENT_3D('',#53596,#23379,#23380);
#19431=AXIS2_PLACEMENT_3D('',#53597,#23381,#23382);
#19432=AXIS2_PLACEMENT_3D('',#53598,#23383,#23384);
#19433=AXIS2_PLACEMENT_3D('',#53599,#23385,#23386);
#19434=AXIS2_PLACEMENT_3D('',#53600,#23387,#23388);
#19435=AXIS2_PLACEMENT_3D('',#53601,#23389,#23390);
#19436=AXIS2_PLACEMENT_3D('',#53602,#23391,#23392);
#19437=AXIS2_PLACEMENT_3D('',#53603,#23393,#23394);
#19438=AXIS2_PLACEMENT_3D('',#53618,#23395,#23396);
#19439=AXIS2_PLACEMENT_3D('',#53633,#23397,#23398);
#19440=AXIS2_PLACEMENT_3D('',#53634,#23399,#23400);
#19441=AXIS2_PLACEMENT_3D('',#53635,#23401,#23402);
#19442=AXIS2_PLACEMENT_3D('',#53636,#23403,#23404);
#19443=AXIS2_PLACEMENT_3D('',#53637,#23405,#23406);
#19444=AXIS2_PLACEMENT_3D('',#53638,#23407,#23408);
#19445=AXIS2_PLACEMENT_3D('',#53639,#23409,#23410);
#19446=AXIS2_PLACEMENT_3D('',#53640,#23411,#23412);
#19447=AXIS2_PLACEMENT_3D('',#53653,#23413,#23414);
#19448=AXIS2_PLACEMENT_3D('',#53654,#23415,#23416);
#19449=AXIS2_PLACEMENT_3D('',#53655,#23417,#23418);
#19450=AXIS2_PLACEMENT_3D('',#53656,#23419,#23420);
#19451=AXIS2_PLACEMENT_3D('',#53657,#23421,#23422);
#19452=AXIS2_PLACEMENT_3D('',#53658,#23423,#23424);
#19453=AXIS2_PLACEMENT_3D('',#53659,#23425,#23426);
#19454=AXIS2_PLACEMENT_3D('',#53660,#23427,#23428);
#19455=AXIS2_PLACEMENT_3D('',#53680,#23429,#23430);
#19456=AXIS2_PLACEMENT_3D('',#53681,#23431,#23432);
#19457=AXIS2_PLACEMENT_3D('',#53682,#23433,#23434);
#19458=AXIS2_PLACEMENT_3D('',#53683,#23435,#23436);
#19459=AXIS2_PLACEMENT_3D('',#53684,#23437,#23438);
#19460=AXIS2_PLACEMENT_3D('',#53724,#23439,#23440);
#19461=AXIS2_PLACEMENT_3D('',#53725,#23441,#23442);
#19462=AXIS2_PLACEMENT_3D('',#53726,#23443,#23444);
#19463=AXIS2_PLACEMENT_3D('',#53727,#23445,#23446);
#19464=AXIS2_PLACEMENT_3D('',#53728,#23447,#23448);
#19465=AXIS2_PLACEMENT_3D('',#53729,#23449,#23450);
#19466=AXIS2_PLACEMENT_3D('',#53730,#23451,#23452);
#19467=AXIS2_PLACEMENT_3D('',#53731,#23453,#23454);
#19468=AXIS2_PLACEMENT_3D('',#53732,#23455,#23456);
#19469=AXIS2_PLACEMENT_3D('',#53733,#23457,#23458);
#19470=AXIS2_PLACEMENT_3D('',#53749,#23459,#23460);
#19471=AXIS2_PLACEMENT_3D('',#53750,#23461,#23462);
#19472=AXIS2_PLACEMENT_3D('',#53751,#23463,#23464);
#19473=AXIS2_PLACEMENT_3D('',#53752,#23465,#23466);
#19474=AXIS2_PLACEMENT_3D('',#53753,#23467,#23468);
#19475=AXIS2_PLACEMENT_3D('',#53754,#23469,#23470);
#19476=AXIS2_PLACEMENT_3D('',#53755,#23471,#23472);
#19477=AXIS2_PLACEMENT_3D('',#53756,#23473,#23474);
#19478=AXIS2_PLACEMENT_3D('',#53757,#23475,#23476);
#19479=AXIS2_PLACEMENT_3D('',#53758,#23477,#23478);
#19480=AXIS2_PLACEMENT_3D('',#53759,#23479,#23480);
#19481=AXIS2_PLACEMENT_3D('',#53760,#23481,#23482);
#19482=AXIS2_PLACEMENT_3D('',#53761,#23483,#23484);
#19483=AXIS2_PLACEMENT_3D('',#53762,#23485,#23486);
#19484=AXIS2_PLACEMENT_3D('',#53763,#23487,#23488);
#19485=AXIS2_PLACEMENT_3D('',#53764,#23489,#23490);
#19486=AXIS2_PLACEMENT_3D('',#53765,#23491,#23492);
#19487=AXIS2_PLACEMENT_3D('',#53785,#23493,#23494);
#19488=AXIS2_PLACEMENT_3D('',#53786,#23495,#23496);
#19489=AXIS2_PLACEMENT_3D('',#53787,#23497,#23498);
#19490=AXIS2_PLACEMENT_3D('',#53788,#23499,#23500);
#19491=AXIS2_PLACEMENT_3D('',#53789,#23501,#23502);
#19492=AXIS2_PLACEMENT_3D('',#53790,#23503,#23504);
#19493=AXIS2_PLACEMENT_3D('',#53791,#23505,#23506);
#19494=AXIS2_PLACEMENT_3D('',#53831,#23507,#23508);
#19495=AXIS2_PLACEMENT_3D('',#53832,#23509,#23510);
#19496=AXIS2_PLACEMENT_3D('',#53833,#23511,#23512);
#19497=AXIS2_PLACEMENT_3D('',#53834,#23513,#23514);
#19498=AXIS2_PLACEMENT_3D('',#53835,#23515,#23516);
#19499=AXIS2_PLACEMENT_3D('',#53851,#23517,#23518);
#19500=AXIS2_PLACEMENT_3D('',#53852,#23519,#23520);
#19501=AXIS2_PLACEMENT_3D('',#53853,#23521,#23522);
#19502=AXIS2_PLACEMENT_3D('',#53854,#23523,#23524);
#19503=AXIS2_PLACEMENT_3D('',#53855,#23525,#23526);
#19504=AXIS2_PLACEMENT_3D('',#53856,#23527,#23528);
#19505=AXIS2_PLACEMENT_3D('',#53857,#23529,#23530);
#19506=AXIS2_PLACEMENT_3D('',#53858,#23531,#23532);
#19507=AXIS2_PLACEMENT_3D('',#53859,#23533,#23534);
#19508=AXIS2_PLACEMENT_3D('',#53879,#23535,#23536);
#19509=AXIS2_PLACEMENT_3D('',#53880,#23537,#23538);
#19510=AXIS2_PLACEMENT_3D('',#53929,#23539,#23540);
#19511=AXIS2_PLACEMENT_3D('',#53945,#23541,#23542);
#19512=AXIS2_PLACEMENT_3D('',#53946,#23543,#23544);
#19513=AXIS2_PLACEMENT_3D('',#53947,#23545,#23546);
#19514=AXIS2_PLACEMENT_3D('',#53948,#23547,#23548);
#19515=AXIS2_PLACEMENT_3D('',#53949,#23549,#23550);
#19516=AXIS2_PLACEMENT_3D('',#53950,#23551,#23552);
#19517=AXIS2_PLACEMENT_3D('',#53951,#23553,#23554);
#19518=AXIS2_PLACEMENT_3D('',#53967,#23555,#23556);
#19519=AXIS2_PLACEMENT_3D('',#53968,#23557,#23558);
#19520=AXIS2_PLACEMENT_3D('',#53969,#23559,#23560);
#19521=AXIS2_PLACEMENT_3D('',#53989,#23561,#23562);
#19522=AXIS2_PLACEMENT_3D('',#53990,#23563,#23564);
#19523=AXIS2_PLACEMENT_3D('',#53991,#23565,#23566);
#19524=AXIS2_PLACEMENT_3D('',#54031,#23567,#23568);
#19525=AXIS2_PLACEMENT_3D('',#54032,#23569,#23570);
#19526=AXIS2_PLACEMENT_3D('',#54033,#23571,#23572);
#19527=AXIS2_PLACEMENT_3D('',#54062,#23573,#23574);
#19528=AXIS2_PLACEMENT_3D('',#54063,#23575,#23576);
#19529=AXIS2_PLACEMENT_3D('',#54064,#23577,#23578);
#19530=AXIS2_PLACEMENT_3D('',#54065,#23579,#23580);
#19531=AXIS2_PLACEMENT_3D('',#54066,#23581,#23582);
#19532=AXIS2_PLACEMENT_3D('',#54067,#23583,#23584);
#19533=AXIS2_PLACEMENT_3D('',#54068,#23585,#23586);
#19534=AXIS2_PLACEMENT_3D('',#54069,#23587,#23588);
#19535=AXIS2_PLACEMENT_3D('',#54070,#23589,#23590);
#19536=AXIS2_PLACEMENT_3D('',#54071,#23591,#23592);
#19537=AXIS2_PLACEMENT_3D('',#54072,#23593,#23594);
#19538=AXIS2_PLACEMENT_3D('',#54073,#23595,#23596);
#19539=AXIS2_PLACEMENT_3D('',#54074,#23597,#23598);
#19540=AXIS2_PLACEMENT_3D('',#54075,#23599,#23600);
#19541=AXIS2_PLACEMENT_3D('',#54076,#23601,#23602);
#19542=AXIS2_PLACEMENT_3D('',#54077,#23603,#23604);
#19543=AXIS2_PLACEMENT_3D('',#54078,#23605,#23606);
#19544=AXIS2_PLACEMENT_3D('',#54110,#23607,#23608);
#19545=AXIS2_PLACEMENT_3D('',#54133,#23609,#23610);
#19546=AXIS2_PLACEMENT_3D('',#54134,#23611,#23612);
#19547=AXIS2_PLACEMENT_3D('',#54300,#23613,#23614);
#19548=AXIS2_PLACEMENT_3D('',#54301,#23615,#23616);
#19549=AXIS2_PLACEMENT_3D('',#54326,#23617,#23618);
#19550=AXIS2_PLACEMENT_3D('',#54348,#23619,#23620);
#19551=AXIS2_PLACEMENT_3D('',#54349,#23621,#23622);
#19552=AXIS2_PLACEMENT_3D('',#54350,#23623,#23624);
#19553=AXIS2_PLACEMENT_3D('',#54351,#23625,#23626);
#19554=AXIS2_PLACEMENT_3D('',#54352,#23627,#23628);
#19555=AXIS2_PLACEMENT_3D('',#54377,#23629,#23630);
#19556=AXIS2_PLACEMENT_3D('',#54402,#23631,#23632);
#19557=AXIS2_PLACEMENT_3D('',#54403,#23633,#23634);
#19558=AXIS2_PLACEMENT_3D('',#54404,#23635,#23636);
#19559=AXIS2_PLACEMENT_3D('',#54405,#23637,#23638);
#19560=AXIS2_PLACEMENT_3D('',#54430,#23639,#23640);
#19561=AXIS2_PLACEMENT_3D('',#54455,#23641,#23642);
#19562=AXIS2_PLACEMENT_3D('',#54456,#23643,#23644);
#19563=AXIS2_PLACEMENT_3D('',#54457,#23645,#23646);
#19564=AXIS2_PLACEMENT_3D('',#54458,#23647,#23648);
#19565=AXIS2_PLACEMENT_3D('',#54459,#23649,#23650);
#19566=AXIS2_PLACEMENT_3D('',#54460,#23651,#23652);
#19567=AXIS2_PLACEMENT_3D('',#54461,#23653,#23654);
#19568=AXIS2_PLACEMENT_3D('',#54483,#23655,#23656);
#19569=AXIS2_PLACEMENT_3D('',#54508,#23657,#23658);
#19570=AXIS2_PLACEMENT_3D('',#54509,#23659,#23660);
#19571=AXIS2_PLACEMENT_3D('',#54510,#23661,#23662);
#19572=AXIS2_PLACEMENT_3D('',#54512,#23664,#23665);
#19573=AXIS2_PLACEMENT_3D('',#54514,#23667,#23668);
#19574=AXIS2_PLACEMENT_3D('',#54516,#23670,#23671);
#19575=AXIS2_PLACEMENT_3D('',#54518,#23673,#23674);
#19576=AXIS2_PLACEMENT_3D('',#54519,#23675,#23676);
#19577=AXIS2_PLACEMENT_3D('',#54520,#23677,#23678);
#19578=AXIS2_PLACEMENT_3D('',#54521,#23679,#23680);
#19579=AXIS2_PLACEMENT_3D('',#54523,#23681,#23682);
#19580=AXIS2_PLACEMENT_3D('',#54525,#23683,#23684);
#19581=AXIS2_PLACEMENT_3D('',#54526,#23685,#23686);
#19582=AXIS2_PLACEMENT_3D('',#54528,#23687,#23688);
#19583=AXIS2_PLACEMENT_3D('',#54529,#23689,#23690);
#19584=AXIS2_PLACEMENT_3D('',#54531,#23691,#23692);
#19585=AXIS2_PLACEMENT_3D('',#54533,#23694,#23695);
#19586=AXIS2_PLACEMENT_3D('',#54534,#23696,#23697);
#19587=AXIS2_PLACEMENT_3D('',#54535,#23698,#23699);
#19588=AXIS2_PLACEMENT_3D('',#54536,#23700,#23701);
#19589=AXIS2_PLACEMENT_3D('',#54537,#23702,#23703);
#19590=AXIS2_PLACEMENT_3D('',#54538,#23704,#23705);
#19591=AXIS2_PLACEMENT_3D('',#54539,#23706,#23707);
#19592=AXIS2_PLACEMENT_3D('',#54540,#23708,#23709);
#19593=AXIS2_PLACEMENT_3D('',#54541,#23710,#23711);
#19594=AXIS2_PLACEMENT_3D('',#54542,#23712,#23713);
#19595=AXIS2_PLACEMENT_3D('',#54543,#23714,#23715);
#19596=AXIS2_PLACEMENT_3D('',#54544,#23716,#23717);
#19597=AXIS2_PLACEMENT_3D('',#54545,#23718,#23719);
#19598=AXIS2_PLACEMENT_3D('',#54546,#23720,#23721);
#19599=AXIS2_PLACEMENT_3D('',#54547,#23722,#23723);
#19600=AXIS2_PLACEMENT_3D('',#54548,#23724,#23725);
#19601=DIRECTION('axis',(0.,0.,1.));
#19602=DIRECTION('refdir',(1.,0.,0.));
#19603=DIRECTION('axis',(0.,0.,1.));
#19604=DIRECTION('refdir',(1.,0.,0.));
#19605=DIRECTION('center_axis',(-1.,0.,0.));
#19606=DIRECTION('ref_axis',(0.,0.,1.));
#19607=DIRECTION('center_axis',(-1.,0.,0.));
#19608=DIRECTION('ref_axis',(0.,0.997668769190539,0.0682424133646747));
#19609=DIRECTION('center_axis',(-1.,0.,0.));
#19610=DIRECTION('ref_axis',(0.,0.997668769190539,0.0682424133646747));
#19611=DIRECTION('center_axis',(-1.,0.,0.));
#19612=DIRECTION('ref_axis',(0.,0.997668769190539,0.0682424133646747));
#19613=DIRECTION('center_axis',(-1.,0.,0.));
#19614=DIRECTION('ref_axis',(0.,0.,1.));
#19615=DIRECTION('center_axis',(-1.,0.,0.));
#19616=DIRECTION('ref_axis',(0.,0.979084087682322,0.203456013052637));
#19617=DIRECTION('center_axis',(-1.,0.,0.));
#19618=DIRECTION('ref_axis',(0.,0.979084087682322,0.203456013052637));
#19619=DIRECTION('center_axis',(-1.,0.,0.));
#19620=DIRECTION('ref_axis',(0.,0.979084087682322,0.203456013052637));
#19621=DIRECTION('center_axis',(-1.,0.,0.));
#19622=DIRECTION('ref_axis',(0.,0.,1.));
#19623=DIRECTION('center_axis',(-1.,0.,0.));
#19624=DIRECTION('ref_axis',(0.,0.942260922118819,0.33487961217099));
#19625=DIRECTION('center_axis',(-1.,0.,0.));
#19626=DIRECTION('ref_axis',(0.,0.942260922118819,0.33487961217099));
#19627=DIRECTION('center_axis',(-1.,0.,0.));
#19628=DIRECTION('ref_axis',(0.,0.942260922118819,0.33487961217099));
#19629=DIRECTION('center_axis',(-1.,0.,0.));
#19630=DIRECTION('ref_axis',(0.,0.,1.));
#19631=DIRECTION('center_axis',(-1.,0.,0.));
#19632=DIRECTION('ref_axis',(0.,0.887885218402373,0.460065037731156));
#19633=DIRECTION('center_axis',(-1.,0.,0.));
#19634=DIRECTION('ref_axis',(0.,0.887885218402373,0.460065037731156));
#19635=DIRECTION('center_axis',(-1.,0.,0.));
#19636=DIRECTION('ref_axis',(0.,0.887885218402373,0.460065037731156));
#19637=DIRECTION('center_axis',(-1.,0.,0.));
#19638=DIRECTION('ref_axis',(0.,0.,1.));
#19639=DIRECTION('center_axis',(-1.,0.,0.));
#19640=DIRECTION('ref_axis',(0.,0.816969893010439,0.576680322114871));
#19641=DIRECTION('center_axis',(-1.,0.,0.));
#19642=DIRECTION('ref_axis',(0.,0.816969893010439,0.576680322114871));
#19643=DIRECTION('center_axis',(-1.,0.,0.));
#19644=DIRECTION('ref_axis',(0.,0.816969893010439,0.576680322114871));
#19645=DIRECTION('center_axis',(-1.,0.,0.));
#19646=DIRECTION('ref_axis',(0.,0.,1.));
#19647=DIRECTION('center_axis',(-1.,0.,0.));
#19648=DIRECTION('ref_axis',(0.,0.730835964278121,0.682553143218658));
#19649=DIRECTION('center_axis',(-1.,0.,0.));
#19650=DIRECTION('ref_axis',(0.,0.730835964278121,0.682553143218658));
#19651=DIRECTION('center_axis',(-1.,0.,0.));
#19652=DIRECTION('ref_axis',(0.,0.730835964278121,0.682553143218658));
#19653=DIRECTION('center_axis',(-1.,0.,0.));
#19654=DIRECTION('ref_axis',(0.,0.,1.));
#19655=DIRECTION('center_axis',(-1.,0.,0.));
#19656=DIRECTION('ref_axis',(0.,0.631087944326049,0.775711290704423));
#19657=DIRECTION('center_axis',(-1.,0.,0.));
#19658=DIRECTION('ref_axis',(0.,0.631087944326049,0.775711290704423));
#19659=DIRECTION('center_axis',(-1.,0.,0.));
#19660=DIRECTION('ref_axis',(0.,0.631087944326049,0.775711290704423));
#19661=DIRECTION('center_axis',(-1.,0.,0.));
#19662=DIRECTION('ref_axis',(0.,0.,1.));
#19663=DIRECTION('center_axis',(-1.,0.,0.));
#19664=DIRECTION('ref_axis',(0.,0.519583950035429,0.854419404546491));
#19665=DIRECTION('center_axis',(-1.,0.,0.));
#19666=DIRECTION('ref_axis',(0.,0.519583950035429,0.854419404546491));
#19667=DIRECTION('center_axis',(-1.,0.,0.));
#19668=DIRECTION('ref_axis',(0.,0.519583950035429,0.854419404546491));
#19669=DIRECTION('center_axis',(-1.,0.,0.));
#19670=DIRECTION('ref_axis',(0.,0.,1.));
#19671=DIRECTION('center_axis',(-1.,0.,0.));
#19672=DIRECTION('ref_axis',(0.,0.398401089846236,0.917211301505455));
#19673=DIRECTION('center_axis',(-1.,0.,0.));
#19674=DIRECTION('ref_axis',(0.,0.398401089846236,0.917211301505455));
#19675=DIRECTION('center_axis',(-1.,0.,0.));
#19676=DIRECTION('ref_axis',(0.,0.398401089846236,0.917211301505455));
#19677=DIRECTION('center_axis',(-1.,0.,0.));
#19678=DIRECTION('ref_axis',(0.,0.,1.));
#19679=DIRECTION('center_axis',(-1.,0.,0.));
#19680=DIRECTION('ref_axis',(0.,0.269796771157019,0.962917287347801));
#19681=DIRECTION('center_axis',(-1.,0.,0.));
#19682=DIRECTION('ref_axis',(0.,0.269796771157019,0.962917287347801));
#19683=DIRECTION('center_axis',(-1.,0.,0.));
#19684=DIRECTION('ref_axis',(0.,0.269796771157019,0.962917287347801));
#19685=DIRECTION('center_axis',(-1.,0.,0.));
#19686=DIRECTION('ref_axis',(0.,0.,1.));
#19687=DIRECTION('center_axis',(-1.,0.,0.));
#19688=DIRECTION('ref_axis',(0.,0.13616664909624,0.990685946036332));
#19689=DIRECTION('center_axis',(-1.,0.,0.));
#19690=DIRECTION('ref_axis',(0.,0.13616664909624,0.990685946036332));
#19691=DIRECTION('center_axis',(-1.,0.,0.));
#19692=DIRECTION('ref_axis',(0.,0.13616664909624,0.990685946036332));
#19693=DIRECTION('center_axis',(-1.,0.,0.));
#19694=DIRECTION('ref_axis',(0.,0.,1.));
#19695=DIRECTION('center_axis',(-1.,0.,0.));
#19696=DIRECTION('ref_axis',(0.,-6.98296267768627E-15,1.));
#19697=DIRECTION('center_axis',(-1.,0.,0.));
#19698=DIRECTION('ref_axis',(0.,-6.98296267768627E-15,1.));
#19699=DIRECTION('center_axis',(-1.,0.,0.));
#19700=DIRECTION('ref_axis',(0.,-6.98296267768627E-15,1.));
#19701=DIRECTION('center_axis',(-1.,0.,0.));
#19702=DIRECTION('ref_axis',(0.,0.,1.));
#19703=DIRECTION('center_axis',(-1.,0.,0.));
#19704=DIRECTION('ref_axis',(0.,-0.136166649096254,0.99068594603633));
#19705=DIRECTION('center_axis',(-1.,0.,0.));
#19706=DIRECTION('ref_axis',(0.,-0.136166649096254,0.99068594603633));
#19707=DIRECTION('center_axis',(-1.,0.,0.));
#19708=DIRECTION('ref_axis',(0.,-0.136166649096254,0.99068594603633));
#19709=DIRECTION('center_axis',(-1.,0.,0.));
#19710=DIRECTION('ref_axis',(0.,0.,1.));
#19711=DIRECTION('center_axis',(-1.,0.,0.));
#19712=DIRECTION('ref_axis',(0.,-0.269796771157031,0.962917287347797));
#19713=DIRECTION('center_axis',(-1.,0.,0.));
#19714=DIRECTION('ref_axis',(0.,-0.269796771157031,0.962917287347797));
#19715=DIRECTION('center_axis',(-1.,0.,0.));
#19716=DIRECTION('ref_axis',(0.,-0.269796771157031,0.962917287347797));
#19717=DIRECTION('center_axis',(-1.,0.,0.));
#19718=DIRECTION('ref_axis',(0.,0.,1.));
#19719=DIRECTION('center_axis',(-1.,0.,0.));
#19720=DIRECTION('ref_axis',(0.,-0.398401089846249,0.91721130150545));
#19721=DIRECTION('center_axis',(-1.,0.,0.));
#19722=DIRECTION('ref_axis',(0.,-0.398401089846249,0.91721130150545));
#19723=DIRECTION('center_axis',(-1.,0.,0.));
#19724=DIRECTION('ref_axis',(0.,-0.398401089846249,0.91721130150545));
#19725=DIRECTION('center_axis',(-1.,0.,0.));
#19726=DIRECTION('ref_axis',(0.,0.,1.));
#19727=DIRECTION('center_axis',(-1.,0.,0.));
#19728=DIRECTION('ref_axis',(0.,-0.51958395003544,0.854419404546485));
#19729=DIRECTION('center_axis',(-1.,0.,0.));
#19730=DIRECTION('ref_axis',(0.,-0.51958395003544,0.854419404546485));
#19731=DIRECTION('center_axis',(-1.,0.,0.));
#19732=DIRECTION('ref_axis',(0.,-0.51958395003544,0.854419404546485));
#19733=DIRECTION('center_axis',(-1.,0.,0.));
#19734=DIRECTION('ref_axis',(0.,0.,1.));
#19735=DIRECTION('center_axis',(-1.,0.,0.));
#19736=DIRECTION('ref_axis',(0.,-0.631087944326059,0.775711290704415));
#19737=DIRECTION('center_axis',(-1.,0.,0.));
#19738=DIRECTION('ref_axis',(0.,-0.631087944326059,0.775711290704415));
#19739=DIRECTION('center_axis',(-1.,0.,0.));
#19740=DIRECTION('ref_axis',(0.,-0.631087944326059,0.775711290704415));
#19741=DIRECTION('center_axis',(-1.,0.,0.));
#19742=DIRECTION('ref_axis',(0.,0.,1.));
#19743=DIRECTION('center_axis',(-1.,0.,0.));
#19744=DIRECTION('ref_axis',(0.,-0.73083596427813,0.682553143218648));
#19745=DIRECTION('center_axis',(-1.,0.,0.));
#19746=DIRECTION('ref_axis',(0.,-0.73083596427813,0.682553143218648));
#19747=DIRECTION('center_axis',(-1.,0.,0.));
#19748=DIRECTION('ref_axis',(0.,-0.73083596427813,0.682553143218648));
#19749=DIRECTION('center_axis',(-1.,0.,0.));
#19750=DIRECTION('ref_axis',(0.,0.,1.));
#19751=DIRECTION('center_axis',(-1.,0.,0.));
#19752=DIRECTION('ref_axis',(0.,-0.816969893010447,0.57668032211486));
#19753=DIRECTION('center_axis',(-1.,0.,0.));
#19754=DIRECTION('ref_axis',(0.,-0.816969893010447,0.57668032211486));
#19755=DIRECTION('center_axis',(-1.,0.,0.));
#19756=DIRECTION('ref_axis',(0.,-0.816969893010447,0.57668032211486));
#19757=DIRECTION('center_axis',(-1.,0.,0.));
#19758=DIRECTION('ref_axis',(0.,0.,1.));
#19759=DIRECTION('center_axis',(-1.,0.,0.));
#19760=DIRECTION('ref_axis',(0.,-0.887885218402379,0.460065037731144));
#19761=DIRECTION('center_axis',(-1.,0.,0.));
#19762=DIRECTION('ref_axis',(0.,-0.887885218402379,0.460065037731144));
#19763=DIRECTION('center_axis',(-1.,0.,0.));
#19764=DIRECTION('ref_axis',(0.,-0.887885218402379,0.460065037731144));
#19765=DIRECTION('center_axis',(-1.,0.,0.));
#19766=DIRECTION('ref_axis',(0.,0.,1.));
#19767=DIRECTION('center_axis',(-1.,0.,0.));
#19768=DIRECTION('ref_axis',(0.,-0.942260922118824,0.334879612170977));
#19769=DIRECTION('center_axis',(-1.,0.,0.));
#19770=DIRECTION('ref_axis',(0.,-0.942260922118824,0.334879612170977));
#19771=DIRECTION('center_axis',(-1.,0.,0.));
#19772=DIRECTION('ref_axis',(0.,-0.942260922118824,0.334879612170977));
#19773=DIRECTION('center_axis',(-1.,0.,0.));
#19774=DIRECTION('ref_axis',(0.,0.,1.));
#19775=DIRECTION('center_axis',(-1.,0.,0.));
#19776=DIRECTION('ref_axis',(0.,-0.979084087682325,0.203456013052624));
#19777=DIRECTION('center_axis',(-1.,0.,0.));
#19778=DIRECTION('ref_axis',(0.,-0.979084087682325,0.203456013052624));
#19779=DIRECTION('center_axis',(-1.,0.,0.));
#19780=DIRECTION('ref_axis',(0.,-0.979084087682325,0.203456013052624));
#19781=DIRECTION('center_axis',(-1.,0.,0.));
#19782=DIRECTION('ref_axis',(0.,0.,1.));
#19783=DIRECTION('center_axis',(-1.,0.,0.));
#19784=DIRECTION('ref_axis',(0.,-0.99766876919054,0.0682424133646607));
#19785=DIRECTION('center_axis',(-1.,0.,0.));
#19786=DIRECTION('ref_axis',(0.,-0.99766876919054,0.0682424133646607));
#19787=DIRECTION('center_axis',(-1.,0.,0.));
#19788=DIRECTION('ref_axis',(0.,-0.99766876919054,0.0682424133646607));
#19789=DIRECTION('center_axis',(-1.,0.,0.));
#19790=DIRECTION('ref_axis',(0.,0.,1.));
#19791=DIRECTION('center_axis',(-1.,0.,0.));
#19792=DIRECTION('ref_axis',(0.,-0.997668769190538,-0.0682424133646816));
#19793=DIRECTION('center_axis',(-1.,0.,0.));
#19794=DIRECTION('ref_axis',(0.,-0.997668769190538,-0.0682424133646816));
#19795=DIRECTION('center_axis',(-1.,0.,0.));
#19796=DIRECTION('ref_axis',(0.,-0.997668769190538,-0.0682424133646816));
#19797=DIRECTION('center_axis',(-1.,0.,0.));
#19798=DIRECTION('ref_axis',(0.,0.,1.));
#19799=DIRECTION('center_axis',(-1.,0.,0.));
#19800=DIRECTION('ref_axis',(0.,-0.979084087682321,-0.203456013052644));
#19801=DIRECTION('center_axis',(-1.,0.,0.));
#19802=DIRECTION('ref_axis',(0.,-0.979084087682321,-0.203456013052644));
#19803=DIRECTION('center_axis',(-1.,0.,0.));
#19804=DIRECTION('ref_axis',(0.,-0.979084087682321,-0.203456013052644));
#19805=DIRECTION('center_axis',(-1.,0.,0.));
#19806=DIRECTION('ref_axis',(0.,0.,1.));
#19807=DIRECTION('center_axis',(-1.,0.,0.));
#19808=DIRECTION('ref_axis',(0.,-0.942260922118817,-0.334879612170997));
#19809=DIRECTION('center_axis',(-1.,0.,0.));
#19810=DIRECTION('ref_axis',(0.,-0.942260922118817,-0.334879612170997));
#19811=DIRECTION('center_axis',(-1.,0.,0.));
#19812=DIRECTION('ref_axis',(0.,-0.942260922118817,-0.334879612170997));
#19813=DIRECTION('center_axis',(-1.,0.,0.));
#19814=DIRECTION('ref_axis',(0.,0.,1.));
#19815=DIRECTION('center_axis',(-1.,0.,0.));
#19816=DIRECTION('ref_axis',(0.,-0.88788521840237,-0.460065037731162));
#19817=DIRECTION('center_axis',(-1.,0.,0.));
#19818=DIRECTION('ref_axis',(0.,-0.88788521840237,-0.460065037731162));
#19819=DIRECTION('center_axis',(-1.,0.,0.));
#19820=DIRECTION('ref_axis',(0.,-0.88788521840237,-0.460065037731162));
#19821=DIRECTION('center_axis',(-1.,0.,0.));
#19822=DIRECTION('ref_axis',(0.,0.,1.));
#19823=DIRECTION('center_axis',(-1.,0.,0.));
#19824=DIRECTION('ref_axis',(0.,-0.816969893010436,-0.576680322114876));
#19825=DIRECTION('center_axis',(-1.,0.,0.));
#19826=DIRECTION('ref_axis',(0.,-0.816969893010436,-0.576680322114876));
#19827=DIRECTION('center_axis',(-1.,0.,0.));
#19828=DIRECTION('ref_axis',(0.,-0.816969893010436,-0.576680322114876));
#19829=DIRECTION('center_axis',(-1.,0.,0.));
#19830=DIRECTION('ref_axis',(0.,0.,1.));
#19831=DIRECTION('center_axis',(-1.,0.,0.));
#19832=DIRECTION('ref_axis',(0.,-0.730835964278116,-0.682553143218663));
#19833=DIRECTION('center_axis',(-1.,0.,0.));
#19834=DIRECTION('ref_axis',(0.,-0.730835964278116,-0.682553143218663));
#19835=DIRECTION('center_axis',(-1.,0.,0.));
#19836=DIRECTION('ref_axis',(0.,-0.730835964278116,-0.682553143218663));
#19837=DIRECTION('center_axis',(-1.,0.,0.));
#19838=DIRECTION('ref_axis',(0.,0.,1.));
#19839=DIRECTION('center_axis',(-1.,0.,0.));
#19840=DIRECTION('ref_axis',(0.,-0.631087944326043,-0.775711290704428));
#19841=DIRECTION('center_axis',(-1.,0.,0.));
#19842=DIRECTION('ref_axis',(0.,-0.631087944326043,-0.775711290704428));
#19843=DIRECTION('center_axis',(-1.,0.,0.));
#19844=DIRECTION('ref_axis',(0.,-0.631087944326043,-0.775711290704428));
#19845=DIRECTION('center_axis',(-1.,0.,0.));
#19846=DIRECTION('ref_axis',(0.,0.,1.));
#19847=DIRECTION('center_axis',(-1.,0.,0.));
#19848=DIRECTION('ref_axis',(0.,-0.519583950035423,-0.854419404546495));
#19849=DIRECTION('center_axis',(-1.,0.,0.));
#19850=DIRECTION('ref_axis',(0.,-0.519583950035423,-0.854419404546495));
#19851=DIRECTION('center_axis',(-1.,0.,0.));
#19852=DIRECTION('ref_axis',(0.,-0.519583950035423,-0.854419404546495));
#19853=DIRECTION('center_axis',(-1.,0.,0.));
#19854=DIRECTION('ref_axis',(0.,0.,1.));
#19855=DIRECTION('center_axis',(-1.,0.,0.));
#19856=DIRECTION('ref_axis',(0.,-0.398401089846229,-0.917211301505458));
#19857=DIRECTION('center_axis',(-1.,0.,0.));
#19858=DIRECTION('ref_axis',(0.,-0.398401089846229,-0.917211301505458));
#19859=DIRECTION('center_axis',(-1.,0.,0.));
#19860=DIRECTION('ref_axis',(0.,-0.398401089846229,-0.917211301505458));
#19861=DIRECTION('center_axis',(-1.,0.,0.));
#19862=DIRECTION('ref_axis',(0.,0.,1.));
#19863=DIRECTION('center_axis',(-1.,0.,0.));
#19864=DIRECTION('ref_axis',(0.,-0.269796771157012,-0.962917287347803));
#19865=DIRECTION('center_axis',(-1.,0.,0.));
#19866=DIRECTION('ref_axis',(0.,-0.269796771157012,-0.962917287347803));
#19867=DIRECTION('center_axis',(-1.,0.,0.));
#19868=DIRECTION('ref_axis',(0.,-0.269796771157012,-0.962917287347803));
#19869=DIRECTION('center_axis',(-1.,0.,0.));
#19870=DIRECTION('ref_axis',(0.,0.,1.));
#19871=DIRECTION('center_axis',(-1.,0.,0.));
#19872=DIRECTION('ref_axis',(0.,-0.136166649096233,-0.990685946036333));
#19873=DIRECTION('center_axis',(-1.,0.,0.));
#19874=DIRECTION('ref_axis',(0.,-0.136166649096233,-0.990685946036333));
#19875=DIRECTION('center_axis',(-1.,0.,0.));
#19876=DIRECTION('ref_axis',(0.,-0.136166649096233,-0.990685946036333));
#19877=DIRECTION('center_axis',(-1.,0.,0.));
#19878=DIRECTION('ref_axis',(0.,0.,1.));
#19879=DIRECTION('center_axis',(-1.,0.,0.));
#19880=DIRECTION('ref_axis',(0.,0.,-1.));
#19881=DIRECTION('center_axis',(-1.,0.,0.));
#19882=DIRECTION('ref_axis',(0.,0.,-1.));
#19883=DIRECTION('center_axis',(-1.,0.,0.));
#19884=DIRECTION('ref_axis',(0.,0.,-1.));
#19885=DIRECTION('center_axis',(-1.,0.,0.));
#19886=DIRECTION('ref_axis',(0.,0.,1.));
#19887=DIRECTION('center_axis',(-1.,0.,0.));
#19888=DIRECTION('ref_axis',(0.,0.136166649096247,-0.990685946036331));
#19889=DIRECTION('center_axis',(-1.,0.,0.));
#19890=DIRECTION('ref_axis',(0.,0.136166649096247,-0.990685946036331));
#19891=DIRECTION('center_axis',(-1.,0.,0.));
#19892=DIRECTION('ref_axis',(0.,0.136166649096247,-0.990685946036331));
#19893=DIRECTION('center_axis',(-1.,0.,0.));
#19894=DIRECTION('ref_axis',(0.,0.,1.));
#19895=DIRECTION('center_axis',(-1.,0.,0.));
#19896=DIRECTION('ref_axis',(0.,0.269796771157025,-0.962917287347799));
#19897=DIRECTION('center_axis',(-1.,0.,0.));
#19898=DIRECTION('ref_axis',(0.,0.269796771157025,-0.962917287347799));
#19899=DIRECTION('center_axis',(-1.,0.,0.));
#19900=DIRECTION('ref_axis',(0.,0.269796771157025,-0.962917287347799));
#19901=DIRECTION('center_axis',(-1.,0.,0.));
#19902=DIRECTION('ref_axis',(0.,0.,1.));
#19903=DIRECTION('center_axis',(-1.,0.,0.));
#19904=DIRECTION('ref_axis',(0.,0.398401089846243,-0.917211301505452));
#19905=DIRECTION('center_axis',(-1.,0.,0.));
#19906=DIRECTION('ref_axis',(0.,0.398401089846243,-0.917211301505452));
#19907=DIRECTION('center_axis',(-1.,0.,0.));
#19908=DIRECTION('ref_axis',(0.,0.398401089846243,-0.917211301505452));
#19909=DIRECTION('center_axis',(-1.,0.,0.));
#19910=DIRECTION('ref_axis',(0.,0.,1.));
#19911=DIRECTION('center_axis',(-1.,0.,0.));
#19912=DIRECTION('ref_axis',(0.,0.519583950035435,-0.854419404546488));
#19913=DIRECTION('center_axis',(-1.,0.,0.));
#19914=DIRECTION('ref_axis',(0.,0.519583950035435,-0.854419404546488));
#19915=DIRECTION('center_axis',(-1.,0.,0.));
#19916=DIRECTION('ref_axis',(0.,0.519583950035435,-0.854419404546488));
#19917=DIRECTION('center_axis',(-1.,0.,0.));
#19918=DIRECTION('ref_axis',(0.,0.,1.));
#19919=DIRECTION('center_axis',(-1.,0.,0.));
#19920=DIRECTION('ref_axis',(0.,0.631087944326054,-0.775711290704419));
#19921=DIRECTION('center_axis',(-1.,0.,0.));
#19922=DIRECTION('ref_axis',(0.,0.631087944326054,-0.775711290704419));
#19923=DIRECTION('center_axis',(-1.,0.,0.));
#19924=DIRECTION('ref_axis',(0.,0.631087944326054,-0.775711290704419));
#19925=DIRECTION('center_axis',(-1.,0.,0.));
#19926=DIRECTION('ref_axis',(0.,0.,1.));
#19927=DIRECTION('center_axis',(-1.,0.,0.));
#19928=DIRECTION('ref_axis',(0.,0.730835964278126,-0.682553143218653));
#19929=DIRECTION('center_axis',(-1.,0.,0.));
#19930=DIRECTION('ref_axis',(0.,0.730835964278126,-0.682553143218653));
#19931=DIRECTION('center_axis',(-1.,0.,0.));
#19932=DIRECTION('ref_axis',(0.,0.730835964278126,-0.682553143218653));
#19933=DIRECTION('center_axis',(-1.,0.,0.));
#19934=DIRECTION('ref_axis',(0.,0.,1.));
#19935=DIRECTION('center_axis',(-1.,0.,0.));
#19936=DIRECTION('ref_axis',(0.,0.816969893010443,-0.576680322114865));
#19937=DIRECTION('center_axis',(-1.,0.,0.));
#19938=DIRECTION('ref_axis',(0.,0.816969893010443,-0.576680322114865));
#19939=DIRECTION('center_axis',(-1.,0.,0.));
#19940=DIRECTION('ref_axis',(0.,0.816969893010443,-0.576680322114865));
#19941=DIRECTION('center_axis',(-1.,0.,0.));
#19942=DIRECTION('ref_axis',(0.,0.,1.));
#19943=DIRECTION('center_axis',(-1.,0.,0.));
#19944=DIRECTION('ref_axis',(0.,0.887885218402376,-0.46006503773115));
#19945=DIRECTION('center_axis',(-1.,0.,0.));
#19946=DIRECTION('ref_axis',(0.,0.887885218402376,-0.46006503773115));
#19947=DIRECTION('center_axis',(-1.,0.,0.));
#19948=DIRECTION('ref_axis',(0.,0.887885218402376,-0.46006503773115));
#19949=DIRECTION('center_axis',(-1.,0.,0.));
#19950=DIRECTION('ref_axis',(0.,0.,1.));
#19951=DIRECTION('center_axis',(-1.,0.,0.));
#19952=DIRECTION('ref_axis',(0.,0.942260922118822,-0.334879612170983));
#19953=DIRECTION('center_axis',(-1.,0.,0.));
#19954=DIRECTION('ref_axis',(0.,0.942260922118822,-0.334879612170983));
#19955=DIRECTION('center_axis',(-1.,0.,0.));
#19956=DIRECTION('ref_axis',(0.,0.942260922118822,-0.334879612170983));
#19957=DIRECTION('center_axis',(-1.,0.,0.));
#19958=DIRECTION('ref_axis',(0.,0.,1.));
#19959=DIRECTION('center_axis',(-1.,0.,0.));
#19960=DIRECTION('ref_axis',(0.,0.979084087682324,-0.203456013052631));
#19961=DIRECTION('center_axis',(-1.,0.,0.));
#19962=DIRECTION('ref_axis',(0.,0.979084087682323,-0.203456013052631));
#19963=DIRECTION('center_axis',(-1.,0.,0.));
#19964=DIRECTION('ref_axis',(0.,0.979084087682324,-0.203456013052631));
#19965=DIRECTION('center_axis',(-1.,0.,0.));
#19966=DIRECTION('ref_axis',(0.,0.,1.));
#19967=DIRECTION('center_axis',(-1.,0.,0.));
#19968=DIRECTION('ref_axis',(0.,0.997668769190539,-0.0682424133646677));
#19969=DIRECTION('center_axis',(-1.,0.,0.));
#19970=DIRECTION('ref_axis',(0.,0.997668769190539,-0.0682424133646677));
#19971=DIRECTION('center_axis',(-1.,0.,0.));
#19972=DIRECTION('ref_axis',(0.,0.997668769190539,-0.0682424133646677));
#19973=DIRECTION('center_axis',(-1.,0.,0.));
#19974=DIRECTION('ref_axis',(0.,0.,1.));
#19975=DIRECTION('center_axis',(-1.,0.,0.));
#19976=DIRECTION('ref_axis',(0.,0.,1.));
#19977=DIRECTION('center_axis',(-1.,0.,0.));
#19978=DIRECTION('ref_axis',(0.,0.,1.));
#19979=DIRECTION('',(-1.,0.,0.));
#19980=DIRECTION('',(-1.,0.,0.));
#19981=DIRECTION('center_axis',(-1.,0.,0.));
#19982=DIRECTION('ref_axis',(0.,0.,1.));
#19983=DIRECTION('center_axis',(-1.,0.,0.));
#19984=DIRECTION('ref_axis',(0.,0.,1.));
#19985=DIRECTION('',(-1.,0.,0.));
#19986=DIRECTION('center_axis',(-1.,0.,0.));
#19987=DIRECTION('ref_axis',(0.,0.,1.));
#19988=DIRECTION('',(-1.,0.,0.));
#19989=DIRECTION('center_axis',(-1.,0.,0.));
#19990=DIRECTION('ref_axis',(0.,0.,1.));
#19991=DIRECTION('',(-1.,0.,0.));
#19992=DIRECTION('',(-1.,0.,0.));
#19993=DIRECTION('center_axis',(-1.,0.,0.));
#19994=DIRECTION('ref_axis',(0.,0.,1.));
#19995=DIRECTION('center_axis',(-1.,0.,0.));
#19996=DIRECTION('ref_axis',(0.,0.,1.));
#19997=DIRECTION('',(-1.,0.,0.));
#19998=DIRECTION('',(-1.,0.,0.));
#19999=DIRECTION('center_axis',(-1.,0.,0.));
#20000=DIRECTION('ref_axis',(0.,0.,1.));
#20001=DIRECTION('center_axis',(-1.,0.,0.));
#20002=DIRECTION('ref_axis',(0.,0.,1.));
#20003=DIRECTION('',(-1.,0.,0.));
#20004=DIRECTION('',(-1.,0.,0.));
#20005=DIRECTION('center_axis',(-1.,0.,0.));
#20006=DIRECTION('ref_axis',(0.,0.,1.));
#20007=DIRECTION('center_axis',(-1.,0.,0.));
#20008=DIRECTION('ref_axis',(0.,0.,1.));
#20009=DIRECTION('',(-1.,0.,0.));
#20010=DIRECTION('center_axis',(-1.,0.,0.));
#20011=DIRECTION('ref_axis',(0.,0.,1.));
#20012=DIRECTION('',(-1.,0.,0.));
#20013=DIRECTION('center_axis',(-1.,0.,0.));
#20014=DIRECTION('ref_axis',(0.,0.,1.));
#20015=DIRECTION('',(-1.,0.,0.));
#20016=DIRECTION('center_axis',(-1.,0.,0.));
#20017=DIRECTION('ref_axis',(0.,0.,1.));
#20018=DIRECTION('',(-1.,0.,0.));
#20019=DIRECTION('center_axis',(-1.,0.,0.));
#20020=DIRECTION('ref_axis',(0.,0.,1.));
#20021=DIRECTION('',(-1.,0.,0.));
#20022=DIRECTION('',(-1.,0.,0.));
#20023=DIRECTION('center_axis',(-1.,0.,0.));
#20024=DIRECTION('ref_axis',(0.,0.,1.));
#20025=DIRECTION('center_axis',(-1.,0.,0.));
#20026=DIRECTION('ref_axis',(0.,0.,1.));
#20027=DIRECTION('',(-1.,0.,0.));
#20028=DIRECTION('center_axis',(-1.,0.,0.));
#20029=DIRECTION('ref_axis',(0.,0.,1.));
#20030=DIRECTION('',(-1.,0.,0.));
#20031=DIRECTION('center_axis',(-1.,0.,0.));
#20032=DIRECTION('ref_axis',(0.,0.,1.));
#20033=DIRECTION('',(-1.,0.,0.));
#20034=DIRECTION('',(-1.,0.,0.));
#20035=DIRECTION('center_axis',(-1.,0.,0.));
#20036=DIRECTION('ref_axis',(0.,0.,1.));
#20037=DIRECTION('center_axis',(-1.,0.,0.));
#20038=DIRECTION('ref_axis',(0.,0.,1.));
#20039=DIRECTION('',(-1.,0.,0.));
#20040=DIRECTION('',(-1.,0.,0.));
#20041=DIRECTION('center_axis',(-1.,0.,0.));
#20042=DIRECTION('ref_axis',(0.,0.,1.));
#20043=DIRECTION('center_axis',(-1.,0.,0.));
#20044=DIRECTION('ref_axis',(0.,0.,1.));
#20045=DIRECTION('',(-1.,0.,0.));
#20046=DIRECTION('',(-1.,0.,0.));
#20047=DIRECTION('center_axis',(-1.,0.,0.));
#20048=DIRECTION('ref_axis',(0.,0.,1.));
#20049=DIRECTION('center_axis',(-1.,0.,0.));
#20050=DIRECTION('ref_axis',(0.,0.,1.));
#20051=DIRECTION('',(-1.,0.,0.));
#20052=DIRECTION('',(-1.,0.,0.));
#20053=DIRECTION('center_axis',(-1.,0.,0.));
#20054=DIRECTION('ref_axis',(0.,0.,1.));
#20055=DIRECTION('center_axis',(-1.,0.,0.));
#20056=DIRECTION('ref_axis',(0.,0.,1.));
#20057=DIRECTION('',(-1.,0.,0.));
#20058=DIRECTION('center_axis',(-1.,0.,0.));
#20059=DIRECTION('ref_axis',(0.,0.,1.));
#20060=DIRECTION('',(-1.,0.,0.));
#20061=DIRECTION('center_axis',(-1.,0.,0.));
#20062=DIRECTION('ref_axis',(0.,0.,1.));
#20063=DIRECTION('',(-1.,0.,0.));
#20064=DIRECTION('',(-1.,0.,0.));
#20065=DIRECTION('center_axis',(-1.,0.,0.));
#20066=DIRECTION('ref_axis',(0.,0.,1.));
#20067=DIRECTION('center_axis',(-1.,0.,0.));
#20068=DIRECTION('ref_axis',(0.,0.,1.));
#20069=DIRECTION('',(-1.,0.,0.));
#20070=DIRECTION('',(-1.,0.,0.));
#20071=DIRECTION('center_axis',(-1.,0.,0.));
#20072=DIRECTION('ref_axis',(0.,0.,1.));
#20073=DIRECTION('center_axis',(-1.,0.,0.));
#20074=DIRECTION('ref_axis',(0.,0.,1.));
#20075=DIRECTION('',(-1.,0.,0.));
#20076=DIRECTION('',(-1.,0.,0.));
#20077=DIRECTION('center_axis',(-1.,0.,0.));
#20078=DIRECTION('ref_axis',(0.,0.,1.));
#20079=DIRECTION('center_axis',(-1.,0.,0.));
#20080=DIRECTION('ref_axis',(0.,0.,1.));
#20081=DIRECTION('',(-1.,0.,0.));
#20082=DIRECTION('center_axis',(-1.,0.,0.));
#20083=DIRECTION('ref_axis',(0.,0.,1.));
#20084=DIRECTION('',(-1.,0.,0.));
#20085=DIRECTION('center_axis',(-1.,0.,0.));
#20086=DIRECTION('ref_axis',(0.,0.,1.));
#20087=DIRECTION('',(-1.,0.,0.));
#20088=DIRECTION('center_axis',(-1.,0.,0.));
#20089=DIRECTION('ref_axis',(0.,0.,1.));
#20090=DIRECTION('',(-1.,0.,0.));
#20091=DIRECTION('center_axis',(-1.,0.,0.));
#20092=DIRECTION('ref_axis',(0.,0.,1.));
#20093=DIRECTION('',(-1.,0.,0.));
#20094=DIRECTION('',(-1.,0.,0.));
#20095=DIRECTION('center_axis',(-1.,0.,0.));
#20096=DIRECTION('ref_axis',(0.,0.,1.));
#20097=DIRECTION('center_axis',(-1.,0.,0.));
#20098=DIRECTION('ref_axis',(0.,0.,1.));
#20099=DIRECTION('',(-1.,0.,0.));
#20100=DIRECTION('center_axis',(-1.,0.,0.));
#20101=DIRECTION('ref_axis',(0.,0.,1.));
#20102=DIRECTION('',(-1.,0.,0.));
#20103=DIRECTION('center_axis',(-1.,0.,0.));
#20104=DIRECTION('ref_axis',(0.,0.,1.));
#20105=DIRECTION('',(-1.,0.,0.));
#20106=DIRECTION('',(-1.,0.,0.));
#20107=DIRECTION('center_axis',(-1.,0.,0.));
#20108=DIRECTION('ref_axis',(0.,0.,1.));
#20109=DIRECTION('center_axis',(-1.,0.,0.));
#20110=DIRECTION('ref_axis',(0.,0.,1.));
#20111=DIRECTION('',(-1.,0.,0.));
#20112=DIRECTION('',(-1.,0.,0.));
#20113=DIRECTION('center_axis',(-1.,0.,0.));
#20114=DIRECTION('ref_axis',(0.,0.,1.));
#20115=DIRECTION('center_axis',(-1.,0.,0.));
#20116=DIRECTION('ref_axis',(0.,0.,1.));
#20117=DIRECTION('',(-1.,0.,0.));
#20118=DIRECTION('',(-1.,0.,0.));
#20119=DIRECTION('center_axis',(-1.,0.,0.));
#20120=DIRECTION('ref_axis',(0.,0.,1.));
#20121=DIRECTION('center_axis',(-1.,0.,0.));
#20122=DIRECTION('ref_axis',(0.,1.05356763564868E-14,-1.));
#20123=DIRECTION('',(-1.,0.,0.));
#20124=DIRECTION('center_axis',(-1.,0.,0.));
#20125=DIRECTION('ref_axis',(0.,0.,1.));
#20126=DIRECTION('',(-1.,0.,0.));
#20127=DIRECTION('center_axis',(-1.,0.,0.));
#20128=DIRECTION('ref_axis',(0.,0.,1.));
#20129=DIRECTION('',(-1.,0.,0.));
#20130=DIRECTION('',(-1.,0.,0.));
#20131=DIRECTION('center_axis',(-1.,0.,0.));
#20132=DIRECTION('ref_axis',(0.,0.,1.));
#20133=DIRECTION('center_axis',(-1.,0.,0.));
#20134=DIRECTION('ref_axis',(0.,0.,1.));
#20135=DIRECTION('',(-1.,0.,0.));
#20136=DIRECTION('',(-1.,0.,0.));
#20137=DIRECTION('center_axis',(-1.,0.,0.));
#20138=DIRECTION('ref_axis',(0.,0.,1.));
#20139=DIRECTION('center_axis',(-1.,0.,0.));
#20140=DIRECTION('ref_axis',(0.,0.,1.));
#20141=DIRECTION('',(-1.,0.,0.));
#20142=DIRECTION('',(-1.,0.,0.));
#20143=DIRECTION('center_axis',(-1.,0.,0.));
#20144=DIRECTION('ref_axis',(0.,0.,1.));
#20145=DIRECTION('center_axis',(-1.,0.,0.));
#20146=DIRECTION('ref_axis',(0.,0.,1.));
#20147=DIRECTION('',(-1.,0.,0.));
#20148=DIRECTION('center_axis',(-1.,0.,0.));
#20149=DIRECTION('ref_axis',(0.,0.,1.));
#20150=DIRECTION('',(-1.,0.,0.));
#20151=DIRECTION('center_axis',(-1.,0.,0.));
#20152=DIRECTION('ref_axis',(0.,0.,1.));
#20153=DIRECTION('',(-1.,0.,0.));
#20154=DIRECTION('',(-1.,0.,0.));
#20155=DIRECTION('center_axis',(-1.,0.,0.));
#20156=DIRECTION('ref_axis',(0.,0.,1.));
#20157=DIRECTION('center_axis',(-1.,0.,0.));
#20158=DIRECTION('ref_axis',(0.,0.,1.));
#20159=DIRECTION('',(-1.,0.,0.));
#20160=DIRECTION('',(-1.,0.,0.));
#20161=DIRECTION('center_axis',(-1.,0.,0.));
#20162=DIRECTION('ref_axis',(0.,0.,1.));
#20163=DIRECTION('center_axis',(-1.,0.,0.));
#20164=DIRECTION('ref_axis',(0.,0.,1.));
#20165=DIRECTION('',(-1.,0.,0.));
#20166=DIRECTION('center_axis',(-1.,0.,0.));
#20167=DIRECTION('ref_axis',(0.,0.,1.));
#20168=DIRECTION('',(-1.,0.,0.));
#20169=DIRECTION('center_axis',(-1.,0.,0.));
#20170=DIRECTION('ref_axis',(0.,0.,1.));
#20171=DIRECTION('',(-1.,0.,0.));
#20172=DIRECTION('',(-1.,0.,0.));
#20173=DIRECTION('center_axis',(-1.,0.,0.));
#20174=DIRECTION('ref_axis',(0.,0.,1.));
#20175=DIRECTION('center_axis',(-1.,0.,0.));
#20176=DIRECTION('ref_axis',(0.,0.,1.));
#20177=DIRECTION('',(-1.,0.,0.));
#20178=DIRECTION('',(-1.,0.,0.));
#20179=DIRECTION('center_axis',(-1.,0.,0.));
#20180=DIRECTION('ref_axis',(0.,0.,1.));
#20181=DIRECTION('center_axis',(-1.,0.,0.));
#20182=DIRECTION('ref_axis',(0.,0.,1.));
#20183=DIRECTION('',(-1.,0.,0.));
#20184=DIRECTION('',(-1.,0.,0.));
#20185=DIRECTION('center_axis',(-1.,0.,0.));
#20186=DIRECTION('ref_axis',(0.,0.,1.));
#20187=DIRECTION('center_axis',(-1.,0.,0.));
#20188=DIRECTION('ref_axis',(0.,0.,1.));
#20189=DIRECTION('',(-1.,0.,0.));
#20190=DIRECTION('center_axis',(-1.,0.,0.));
#20191=DIRECTION('ref_axis',(0.,0.,1.));
#20192=DIRECTION('',(-1.,0.,0.));
#20193=DIRECTION('center_axis',(-1.,0.,0.));
#20194=DIRECTION('ref_axis',(0.,0.,1.));
#20195=DIRECTION('',(-1.,0.,0.));
#20196=DIRECTION('',(-1.,0.,0.));
#20197=DIRECTION('center_axis',(-1.,0.,0.));
#20198=DIRECTION('ref_axis',(0.,0.,1.));
#20199=DIRECTION('center_axis',(-1.,0.,0.));
#20200=DIRECTION('ref_axis',(0.,0.,1.));
#20201=DIRECTION('',(-1.,0.,0.));
#20202=DIRECTION('',(-1.,0.,0.));
#20203=DIRECTION('center_axis',(-1.,0.,0.));
#20204=DIRECTION('ref_axis',(0.,0.,1.));
#20205=DIRECTION('center_axis',(-1.,0.,0.));
#20206=DIRECTION('ref_axis',(0.,0.,1.));
#20207=DIRECTION('',(-1.,0.,0.));
#20208=DIRECTION('',(-1.,0.,0.));
#20209=DIRECTION('center_axis',(-1.,0.,0.));
#20210=DIRECTION('ref_axis',(0.,0.,1.));
#20211=DIRECTION('center_axis',(-1.,0.,0.));
#20212=DIRECTION('ref_axis',(0.,0.,1.));
#20213=DIRECTION('',(-1.,0.,0.));
#20214=DIRECTION('center_axis',(-1.,0.,0.));
#20215=DIRECTION('ref_axis',(0.,0.,1.));
#20216=DIRECTION('',(-1.,0.,0.));
#20217=DIRECTION('center_axis',(-1.,0.,0.));
#20218=DIRECTION('ref_axis',(0.,0.,1.));
#20219=DIRECTION('',(-1.,0.,0.));
#20220=DIRECTION('',(-1.,0.,0.));
#20221=DIRECTION('center_axis',(-1.,0.,0.));
#20222=DIRECTION('ref_axis',(0.,0.,1.));
#20223=DIRECTION('center_axis',(-1.,0.,0.));
#20224=DIRECTION('ref_axis',(0.,0.,1.));
#20225=DIRECTION('',(-1.,0.,0.));
#20226=DIRECTION('',(-1.,0.,0.));
#20227=DIRECTION('center_axis',(-1.,0.,0.));
#20228=DIRECTION('ref_axis',(0.,0.,1.));
#20229=DIRECTION('center_axis',(-1.,0.,0.));
#20230=DIRECTION('ref_axis',(0.,0.,1.));
#20231=DIRECTION('',(-1.,0.,0.));
#20232=DIRECTION('center_axis',(-1.,0.,0.));
#20233=DIRECTION('ref_axis',(0.,0.,1.));
#20234=DIRECTION('',(-1.,0.,0.));
#20235=DIRECTION('center_axis',(-1.,0.,0.));
#20236=DIRECTION('ref_axis',(0.,0.,1.));
#20237=DIRECTION('',(-1.,0.,0.));
#20238=DIRECTION('',(-1.,0.,0.));
#20239=DIRECTION('center_axis',(-1.,0.,0.));
#20240=DIRECTION('ref_axis',(0.,0.,1.));
#20241=DIRECTION('center_axis',(-1.,0.,0.));
#20242=DIRECTION('ref_axis',(0.,0.,1.));
#20243=DIRECTION('',(-1.,0.,0.));
#20244=DIRECTION('',(-1.,0.,0.));
#20245=DIRECTION('center_axis',(-1.,0.,0.));
#20246=DIRECTION('ref_axis',(0.,0.,1.));
#20247=DIRECTION('center_axis',(1.,0.,0.));
#20248=DIRECTION('ref_axis',(0.,0.,-1.));
#20249=DIRECTION('center_axis',(-1.,0.,0.));
#20250=DIRECTION('ref_axis',(0.,0.997668769190539,0.0682424133646747));
#20251=DIRECTION('center_axis',(1.,0.,0.));
#20252=DIRECTION('ref_axis',(0.,0.,-1.));
#20253=DIRECTION('center_axis',(-1.,0.,0.));
#20254=DIRECTION('ref_axis',(0.,0.997668769190539,-0.0682424133646677));
#20255=DIRECTION('center_axis',(-1.,0.,0.));
#20256=DIRECTION('ref_axis',(0.,0.997668769190539,-0.0682424133646677));
#20257=DIRECTION('center_axis',(1.,0.,0.));
#20258=DIRECTION('ref_axis',(0.,0.,-1.));
#20259=DIRECTION('center_axis',(-1.,0.,0.));
#20260=DIRECTION('ref_axis',(0.,0.979084087682323,-0.203456013052631));
#20261=DIRECTION('center_axis',(-1.,0.,0.));
#20262=DIRECTION('ref_axis',(0.,0.979084087682324,-0.203456013052631));
#20263=DIRECTION('center_axis',(1.,0.,0.));
#20264=DIRECTION('ref_axis',(0.,0.,-1.));
#20265=DIRECTION('center_axis',(-1.,0.,0.));
#20266=DIRECTION('ref_axis',(0.,0.942260922118822,-0.334879612170983));
#20267=DIRECTION('center_axis',(-1.,0.,0.));
#20268=DIRECTION('ref_axis',(0.,0.942260922118822,-0.334879612170983));
#20269=DIRECTION('center_axis',(1.,0.,0.));
#20270=DIRECTION('ref_axis',(0.,0.,-1.));
#20271=DIRECTION('center_axis',(-1.,0.,0.));
#20272=DIRECTION('ref_axis',(0.,0.887885218402376,-0.46006503773115));
#20273=DIRECTION('center_axis',(-1.,0.,0.));
#20274=DIRECTION('ref_axis',(0.,0.887885218402376,-0.46006503773115));
#20275=DIRECTION('center_axis',(1.,0.,0.));
#20276=DIRECTION('ref_axis',(0.,0.,-1.));
#20277=DIRECTION('center_axis',(-1.,0.,0.));
#20278=DIRECTION('ref_axis',(0.,0.816969893010443,-0.576680322114865));
#20279=DIRECTION('center_axis',(-1.,0.,0.));
#20280=DIRECTION('ref_axis',(0.,0.816969893010443,-0.576680322114865));
#20281=DIRECTION('center_axis',(1.,0.,0.));
#20282=DIRECTION('ref_axis',(0.,0.,-1.));
#20283=DIRECTION('center_axis',(-1.,0.,0.));
#20284=DIRECTION('ref_axis',(0.,0.730835964278126,-0.682553143218653));
#20285=DIRECTION('center_axis',(-1.,0.,0.));
#20286=DIRECTION('ref_axis',(0.,0.730835964278126,-0.682553143218653));
#20287=DIRECTION('center_axis',(1.,0.,0.));
#20288=DIRECTION('ref_axis',(0.,0.,-1.));
#20289=DIRECTION('center_axis',(-1.,0.,0.));
#20290=DIRECTION('ref_axis',(0.,0.631087944326054,-0.775711290704419));
#20291=DIRECTION('center_axis',(-1.,0.,0.));
#20292=DIRECTION('ref_axis',(0.,0.631087944326054,-0.775711290704419));
#20293=DIRECTION('center_axis',(1.,0.,0.));
#20294=DIRECTION('ref_axis',(0.,0.,-1.));
#20295=DIRECTION('center_axis',(-1.,0.,0.));
#20296=DIRECTION('ref_axis',(0.,0.519583950035435,-0.854419404546488));
#20297=DIRECTION('center_axis',(-1.,0.,0.));
#20298=DIRECTION('ref_axis',(0.,0.519583950035435,-0.854419404546488));
#20299=DIRECTION('center_axis',(1.,0.,0.));
#20300=DIRECTION('ref_axis',(0.,0.,-1.));
#20301=DIRECTION('center_axis',(-1.,0.,0.));
#20302=DIRECTION('ref_axis',(0.,0.398401089846243,-0.917211301505452));
#20303=DIRECTION('center_axis',(-1.,0.,0.));
#20304=DIRECTION('ref_axis',(0.,0.398401089846243,-0.917211301505452));
#20305=DIRECTION('center_axis',(1.,0.,0.));
#20306=DIRECTION('ref_axis',(0.,0.,-1.));
#20307=DIRECTION('center_axis',(-1.,0.,0.));
#20308=DIRECTION('ref_axis',(0.,0.269796771157025,-0.962917287347799));
#20309=DIRECTION('center_axis',(-1.,0.,0.));
#20310=DIRECTION('ref_axis',(0.,0.269796771157025,-0.962917287347799));
#20311=DIRECTION('center_axis',(1.,0.,0.));
#20312=DIRECTION('ref_axis',(0.,0.,-1.));
#20313=DIRECTION('center_axis',(-1.,0.,0.));
#20314=DIRECTION('ref_axis',(0.,0.136166649096247,-0.990685946036331));
#20315=DIRECTION('center_axis',(-1.,0.,0.));
#20316=DIRECTION('ref_axis',(0.,0.136166649096247,-0.990685946036331));
#20317=DIRECTION('center_axis',(-1.,0.,0.));
#20318=DIRECTION('ref_axis',(0.,0.,1.));
#20319=DIRECTION('center_axis',(1.,0.,0.));
#20320=DIRECTION('ref_axis',(0.,0.,-1.));
#20321=DIRECTION('center_axis',(-1.,0.,0.));
#20322=DIRECTION('ref_axis',(0.,0.,-1.));
#20323=DIRECTION('center_axis',(-1.,0.,0.));
#20324=DIRECTION('ref_axis',(0.,0.,-1.));
#20325=DIRECTION('center_axis',(1.,0.,0.));
#20326=DIRECTION('ref_axis',(0.,0.,-1.));
#20327=DIRECTION('center_axis',(-1.,0.,0.));
#20328=DIRECTION('ref_axis',(0.,-0.136166649096233,-0.990685946036333));
#20329=DIRECTION('center_axis',(-1.,0.,0.));
#20330=DIRECTION('ref_axis',(0.,-0.136166649096233,-0.990685946036333));
#20331=DIRECTION('center_axis',(1.,0.,0.));
#20332=DIRECTION('ref_axis',(0.,0.,-1.));
#20333=DIRECTION('center_axis',(-1.,0.,0.));
#20334=DIRECTION('ref_axis',(0.,-0.269796771157012,-0.962917287347803));
#20335=DIRECTION('center_axis',(-1.,0.,0.));
#20336=DIRECTION('ref_axis',(0.,-0.269796771157012,-0.962917287347803));
#20337=DIRECTION('center_axis',(1.,0.,0.));
#20338=DIRECTION('ref_axis',(0.,0.,-1.));
#20339=DIRECTION('center_axis',(-1.,0.,0.));
#20340=DIRECTION('ref_axis',(0.,-0.398401089846229,-0.917211301505458));
#20341=DIRECTION('center_axis',(-1.,0.,0.));
#20342=DIRECTION('ref_axis',(0.,-0.398401089846229,-0.917211301505458));
#20343=DIRECTION('center_axis',(1.,0.,0.));
#20344=DIRECTION('ref_axis',(0.,0.,-1.));
#20345=DIRECTION('center_axis',(-1.,0.,0.));
#20346=DIRECTION('ref_axis',(0.,-0.519583950035423,-0.854419404546495));
#20347=DIRECTION('center_axis',(-1.,0.,0.));
#20348=DIRECTION('ref_axis',(0.,-0.519583950035423,-0.854419404546495));
#20349=DIRECTION('center_axis',(1.,0.,0.));
#20350=DIRECTION('ref_axis',(0.,0.,-1.));
#20351=DIRECTION('center_axis',(-1.,0.,0.));
#20352=DIRECTION('ref_axis',(0.,-0.631087944326043,-0.775711290704428));
#20353=DIRECTION('center_axis',(-1.,0.,0.));
#20354=DIRECTION('ref_axis',(0.,-0.631087944326043,-0.775711290704428));
#20355=DIRECTION('center_axis',(1.,0.,0.));
#20356=DIRECTION('ref_axis',(0.,0.,-1.));
#20357=DIRECTION('center_axis',(-1.,0.,0.));
#20358=DIRECTION('ref_axis',(0.,-0.730835964278116,-0.682553143218663));
#20359=DIRECTION('center_axis',(-1.,0.,0.));
#20360=DIRECTION('ref_axis',(0.,-0.730835964278116,-0.682553143218663));
#20361=DIRECTION('center_axis',(1.,0.,0.));
#20362=DIRECTION('ref_axis',(0.,0.,-1.));
#20363=DIRECTION('center_axis',(-1.,0.,0.));
#20364=DIRECTION('ref_axis',(0.,-0.816969893010436,-0.576680322114876));
#20365=DIRECTION('center_axis',(-1.,0.,0.));
#20366=DIRECTION('ref_axis',(0.,-0.816969893010436,-0.576680322114876));
#20367=DIRECTION('center_axis',(1.,0.,0.));
#20368=DIRECTION('ref_axis',(0.,0.,-1.));
#20369=DIRECTION('center_axis',(-1.,0.,0.));
#20370=DIRECTION('ref_axis',(0.,-0.88788521840237,-0.460065037731162));
#20371=DIRECTION('center_axis',(-1.,0.,0.));
#20372=DIRECTION('ref_axis',(0.,-0.88788521840237,-0.460065037731162));
#20373=DIRECTION('center_axis',(1.,0.,0.));
#20374=DIRECTION('ref_axis',(0.,0.,-1.));
#20375=DIRECTION('center_axis',(-1.,0.,0.));
#20376=DIRECTION('ref_axis',(0.,-0.942260922118817,-0.334879612170997));
#20377=DIRECTION('center_axis',(-1.,0.,0.));
#20378=DIRECTION('ref_axis',(0.,-0.942260922118817,-0.334879612170997));
#20379=DIRECTION('center_axis',(1.,0.,0.));
#20380=DIRECTION('ref_axis',(0.,0.,-1.));
#20381=DIRECTION('center_axis',(-1.,0.,0.));
#20382=DIRECTION('ref_axis',(0.,-0.979084087682321,-0.203456013052644));
#20383=DIRECTION('center_axis',(-1.,0.,0.));
#20384=DIRECTION('ref_axis',(0.,-0.979084087682321,-0.203456013052644));
#20385=DIRECTION('center_axis',(1.,0.,0.));
#20386=DIRECTION('ref_axis',(0.,0.,-1.));
#20387=DIRECTION('center_axis',(-1.,0.,0.));
#20388=DIRECTION('ref_axis',(0.,-0.997668769190538,-0.0682424133646816));
#20389=DIRECTION('center_axis',(-1.,0.,0.));
#20390=DIRECTION('ref_axis',(0.,-0.997668769190538,-0.0682424133646816));
#20391=DIRECTION('center_axis',(1.,0.,0.));
#20392=DIRECTION('ref_axis',(0.,0.,-1.));
#20393=DIRECTION('center_axis',(-1.,0.,0.));
#20394=DIRECTION('ref_axis',(0.,-0.99766876919054,0.0682424133646607));
#20395=DIRECTION('center_axis',(-1.,0.,0.));
#20396=DIRECTION('ref_axis',(0.,-0.99766876919054,0.0682424133646607));
#20397=DIRECTION('center_axis',(1.,0.,0.));
#20398=DIRECTION('ref_axis',(0.,0.,-1.));
#20399=DIRECTION('center_axis',(-1.,0.,0.));
#20400=DIRECTION('ref_axis',(0.,-0.979084087682325,0.203456013052624));
#20401=DIRECTION('center_axis',(-1.,0.,0.));
#20402=DIRECTION('ref_axis',(0.,-0.979084087682325,0.203456013052624));
#20403=DIRECTION('center_axis',(1.,0.,0.));
#20404=DIRECTION('ref_axis',(0.,0.,-1.));
#20405=DIRECTION('center_axis',(-1.,0.,0.));
#20406=DIRECTION('ref_axis',(0.,-0.942260922118824,0.334879612170977));
#20407=DIRECTION('center_axis',(-1.,0.,0.));
#20408=DIRECTION('ref_axis',(0.,-0.942260922118824,0.334879612170977));
#20409=DIRECTION('center_axis',(1.,0.,0.));
#20410=DIRECTION('ref_axis',(0.,0.,-1.));
#20411=DIRECTION('center_axis',(-1.,0.,0.));
#20412=DIRECTION('ref_axis',(0.,-0.887885218402379,0.460065037731144));
#20413=DIRECTION('center_axis',(-1.,0.,0.));
#20414=DIRECTION('ref_axis',(0.,-0.887885218402379,0.460065037731144));
#20415=DIRECTION('center_axis',(1.,0.,0.));
#20416=DIRECTION('ref_axis',(0.,0.,-1.));
#20417=DIRECTION('center_axis',(-1.,0.,0.));
#20418=DIRECTION('ref_axis',(0.,-0.816969893010447,0.57668032211486));
#20419=DIRECTION('center_axis',(-1.,0.,0.));
#20420=DIRECTION('ref_axis',(0.,-0.816969893010447,0.57668032211486));
#20421=DIRECTION('center_axis',(1.,0.,0.));
#20422=DIRECTION('ref_axis',(0.,0.,-1.));
#20423=DIRECTION('center_axis',(-1.,0.,0.));
#20424=DIRECTION('ref_axis',(0.,-0.73083596427813,0.682553143218648));
#20425=DIRECTION('center_axis',(-1.,0.,0.));
#20426=DIRECTION('ref_axis',(0.,-0.73083596427813,0.682553143218648));
#20427=DIRECTION('center_axis',(1.,0.,0.));
#20428=DIRECTION('ref_axis',(0.,0.,-1.));
#20429=DIRECTION('center_axis',(-1.,0.,0.));
#20430=DIRECTION('ref_axis',(0.,-0.631087944326059,0.775711290704415));
#20431=DIRECTION('center_axis',(-1.,0.,0.));
#20432=DIRECTION('ref_axis',(0.,-0.631087944326059,0.775711290704415));
#20433=DIRECTION('center_axis',(1.,0.,0.));
#20434=DIRECTION('ref_axis',(0.,0.,-1.));
#20435=DIRECTION('center_axis',(-1.,0.,0.));
#20436=DIRECTION('ref_axis',(0.,-0.51958395003544,0.854419404546485));
#20437=DIRECTION('center_axis',(-1.,0.,0.));
#20438=DIRECTION('ref_axis',(0.,-0.51958395003544,0.854419404546485));
#20439=DIRECTION('center_axis',(1.,0.,0.));
#20440=DIRECTION('ref_axis',(0.,0.,-1.));
#20441=DIRECTION('center_axis',(-1.,0.,0.));
#20442=DIRECTION('ref_axis',(0.,-0.398401089846249,0.91721130150545));
#20443=DIRECTION('center_axis',(-1.,0.,0.));
#20444=DIRECTION('ref_axis',(0.,-0.398401089846249,0.91721130150545));
#20445=DIRECTION('center_axis',(1.,0.,0.));
#20446=DIRECTION('ref_axis',(0.,0.,-1.));
#20447=DIRECTION('center_axis',(-1.,0.,0.));
#20448=DIRECTION('ref_axis',(0.,-0.269796771157031,0.962917287347797));
#20449=DIRECTION('center_axis',(-1.,0.,0.));
#20450=DIRECTION('ref_axis',(0.,-0.269796771157031,0.962917287347797));
#20451=DIRECTION('center_axis',(1.,0.,0.));
#20452=DIRECTION('ref_axis',(0.,0.,-1.));
#20453=DIRECTION('center_axis',(-1.,0.,0.));
#20454=DIRECTION('ref_axis',(0.,-0.136166649096254,0.99068594603633));
#20455=DIRECTION('center_axis',(-1.,0.,0.));
#20456=DIRECTION('ref_axis',(0.,-0.136166649096254,0.99068594603633));
#20457=DIRECTION('center_axis',(1.,0.,0.));
#20458=DIRECTION('ref_axis',(0.,0.,-1.));
#20459=DIRECTION('center_axis',(-1.,0.,0.));
#20460=DIRECTION('ref_axis',(0.,-6.98296267768627E-15,1.));
#20461=DIRECTION('center_axis',(-1.,0.,0.));
#20462=DIRECTION('ref_axis',(0.,-6.98296267768627E-15,1.));
#20463=DIRECTION('center_axis',(1.,0.,0.));
#20464=DIRECTION('ref_axis',(0.,0.,-1.));
#20465=DIRECTION('center_axis',(-1.,0.,0.));
#20466=DIRECTION('ref_axis',(0.,0.13616664909624,0.990685946036332));
#20467=DIRECTION('center_axis',(-1.,0.,0.));
#20468=DIRECTION('ref_axis',(0.,0.13616664909624,0.990685946036332));
#20469=DIRECTION('center_axis',(1.,0.,0.));
#20470=DIRECTION('ref_axis',(0.,0.,-1.));
#20471=DIRECTION('center_axis',(-1.,0.,0.));
#20472=DIRECTION('ref_axis',(0.,0.269796771157019,0.962917287347801));
#20473=DIRECTION('center_axis',(-1.,0.,0.));
#20474=DIRECTION('ref_axis',(0.,0.269796771157019,0.962917287347801));
#20475=DIRECTION('center_axis',(1.,0.,0.));
#20476=DIRECTION('ref_axis',(0.,0.,-1.));
#20477=DIRECTION('center_axis',(-1.,0.,0.));
#20478=DIRECTION('ref_axis',(0.,0.398401089846236,0.917211301505455));
#20479=DIRECTION('center_axis',(-1.,0.,0.));
#20480=DIRECTION('ref_axis',(0.,0.398401089846236,0.917211301505455));
#20481=DIRECTION('center_axis',(1.,0.,0.));
#20482=DIRECTION('ref_axis',(0.,0.,-1.));
#20483=DIRECTION('center_axis',(-1.,0.,0.));
#20484=DIRECTION('ref_axis',(0.,0.519583950035429,0.854419404546491));
#20485=DIRECTION('center_axis',(-1.,0.,0.));
#20486=DIRECTION('ref_axis',(0.,0.519583950035429,0.854419404546491));
#20487=DIRECTION('center_axis',(1.,0.,0.));
#20488=DIRECTION('ref_axis',(0.,0.,-1.));
#20489=DIRECTION('center_axis',(-1.,0.,0.));
#20490=DIRECTION('ref_axis',(0.,0.631087944326049,0.775711290704423));
#20491=DIRECTION('center_axis',(-1.,0.,0.));
#20492=DIRECTION('ref_axis',(0.,0.631087944326049,0.775711290704423));
#20493=DIRECTION('center_axis',(1.,0.,0.));
#20494=DIRECTION('ref_axis',(0.,0.,-1.));
#20495=DIRECTION('center_axis',(-1.,0.,0.));
#20496=DIRECTION('ref_axis',(0.,0.730835964278121,0.682553143218658));
#20497=DIRECTION('center_axis',(-1.,0.,0.));
#20498=DIRECTION('ref_axis',(0.,0.730835964278121,0.682553143218658));
#20499=DIRECTION('center_axis',(1.,0.,0.));
#20500=DIRECTION('ref_axis',(0.,0.,-1.));
#20501=DIRECTION('center_axis',(-1.,0.,0.));
#20502=DIRECTION('ref_axis',(0.,0.816969893010439,0.576680322114871));
#20503=DIRECTION('center_axis',(-1.,0.,0.));
#20504=DIRECTION('ref_axis',(0.,0.816969893010439,0.576680322114871));
#20505=DIRECTION('center_axis',(1.,0.,0.));
#20506=DIRECTION('ref_axis',(0.,0.,-1.));
#20507=DIRECTION('center_axis',(-1.,0.,0.));
#20508=DIRECTION('ref_axis',(0.,0.887885218402373,0.460065037731156));
#20509=DIRECTION('center_axis',(-1.,0.,0.));
#20510=DIRECTION('ref_axis',(0.,0.887885218402373,0.460065037731156));
#20511=DIRECTION('center_axis',(1.,0.,0.));
#20512=DIRECTION('ref_axis',(0.,0.,-1.));
#20513=DIRECTION('center_axis',(-1.,0.,0.));
#20514=DIRECTION('ref_axis',(0.,0.942260922118819,0.33487961217099));
#20515=DIRECTION('center_axis',(-1.,0.,0.));
#20516=DIRECTION('ref_axis',(0.,0.942260922118819,0.33487961217099));
#20517=DIRECTION('center_axis',(1.,0.,0.));
#20518=DIRECTION('ref_axis',(0.,0.,-1.));
#20519=DIRECTION('center_axis',(-1.,0.,0.));
#20520=DIRECTION('ref_axis',(0.,0.979084087682322,0.203456013052637));
#20521=DIRECTION('center_axis',(-1.,0.,0.));
#20522=DIRECTION('ref_axis',(0.,0.979084087682322,0.203456013052637));
#20523=DIRECTION('center_axis',(1.,0.,0.));
#20524=DIRECTION('ref_axis',(0.,0.,-1.));
#20525=DIRECTION('center_axis',(-1.,0.,0.));
#20526=DIRECTION('ref_axis',(0.,0.997668769190539,0.0682424133646747));
#20527=DIRECTION('center_axis',(1.,0.,0.));
#20528=DIRECTION('ref_axis',(0.,0.,-1.));
#20529=DIRECTION('center_axis',(-1.,0.,0.));
#20530=DIRECTION('ref_axis',(0.,0.,1.));
#20531=DIRECTION('',(-1.,0.,0.));
#20532=DIRECTION('',(-1.,0.,0.));
#20533=DIRECTION('center_axis',(-1.,0.,0.));
#20534=DIRECTION('ref_axis',(0.,0.,1.));
#20535=DIRECTION('',(-1.,0.,0.));
#20536=DIRECTION('center_axis',(-1.,0.,0.));
#20537=DIRECTION('ref_axis',(0.,0.,1.));
#20538=DIRECTION('',(-1.,0.,0.));
#20539=DIRECTION('center_axis',(-1.,0.,0.));
#20540=DIRECTION('ref_axis',(0.,0.,1.));
#20541=DIRECTION('center_axis',(-1.,0.,0.));
#20542=DIRECTION('ref_axis',(0.,0.,1.));
#20543=DIRECTION('',(-1.,0.,0.));
#20544=DIRECTION('center_axis',(-1.,0.,0.));
#20545=DIRECTION('ref_axis',(0.,0.,1.));
#20546=DIRECTION('',(-1.,0.,0.));
#20547=DIRECTION('center_axis',(-1.,0.,0.));
#20548=DIRECTION('ref_axis',(0.,0.,1.));
#20549=DIRECTION('center_axis',(-1.,0.,0.));
#20550=DIRECTION('ref_axis',(0.,0.,1.));
#20551=DIRECTION('',(-1.,0.,0.));
#20552=DIRECTION('center_axis',(-1.,0.,0.));
#20553=DIRECTION('ref_axis',(0.,0.,1.));
#20554=DIRECTION('',(-1.,0.,0.));
#20555=DIRECTION('center_axis',(-1.,0.,0.));
#20556=DIRECTION('ref_axis',(0.,0.,1.));
#20557=DIRECTION('center_axis',(-1.,0.,0.));
#20558=DIRECTION('ref_axis',(0.,0.,1.));
#20559=DIRECTION('',(-1.,0.,0.));
#20560=DIRECTION('center_axis',(-1.,0.,0.));
#20561=DIRECTION('ref_axis',(0.,0.,1.));
#20562=DIRECTION('',(-1.,0.,0.));
#20563=DIRECTION('center_axis',(-1.,0.,0.));
#20564=DIRECTION('ref_axis',(0.,0.,1.));
#20565=DIRECTION('center_axis',(-1.,0.,0.));
#20566=DIRECTION('ref_axis',(0.,0.,1.));
#20567=DIRECTION('',(-1.,0.,0.));
#20568=DIRECTION('center_axis',(-1.,0.,0.));
#20569=DIRECTION('ref_axis',(0.,0.,1.));
#20570=DIRECTION('',(-1.,0.,0.));
#20571=DIRECTION('center_axis',(-1.,0.,0.));
#20572=DIRECTION('ref_axis',(0.,0.,1.));
#20573=DIRECTION('center_axis',(-1.,0.,0.));
#20574=DIRECTION('ref_axis',(0.,0.,1.));
#20575=DIRECTION('',(-1.,0.,0.));
#20576=DIRECTION('center_axis',(-1.,0.,0.));
#20577=DIRECTION('ref_axis',(0.,0.,1.));
#20578=DIRECTION('',(-1.,0.,0.));
#20579=DIRECTION('center_axis',(-1.,0.,0.));
#20580=DIRECTION('ref_axis',(0.,0.,1.));
#20581=DIRECTION('center_axis',(-1.,0.,0.));
#20582=DIRECTION('ref_axis',(0.,0.,1.));
#20583=DIRECTION('',(-1.,0.,0.));
#20584=DIRECTION('center_axis',(-1.,0.,0.));
#20585=DIRECTION('ref_axis',(0.,0.,1.));
#20586=DIRECTION('',(-1.,0.,0.));
#20587=DIRECTION('center_axis',(-1.,0.,0.));
#20588=DIRECTION('ref_axis',(0.,0.,1.));
#20589=DIRECTION('center_axis',(-1.,0.,0.));
#20590=DIRECTION('ref_axis',(0.,0.,1.));
#20591=DIRECTION('',(-1.,0.,0.));
#20592=DIRECTION('center_axis',(-1.,0.,0.));
#20593=DIRECTION('ref_axis',(0.,0.,1.));
#20594=DIRECTION('',(-1.,0.,0.));
#20595=DIRECTION('center_axis',(-1.,0.,0.));
#20596=DIRECTION('ref_axis',(0.,0.,1.));
#20597=DIRECTION('center_axis',(-1.,0.,0.));
#20598=DIRECTION('ref_axis',(0.,0.,1.));
#20599=DIRECTION('',(-1.,0.,0.));
#20600=DIRECTION('center_axis',(-1.,0.,0.));
#20601=DIRECTION('ref_axis',(0.,0.,1.));
#20602=DIRECTION('',(-1.,0.,0.));
#20603=DIRECTION('center_axis',(-1.,0.,0.));
#20604=DIRECTION('ref_axis',(0.,0.,1.));
#20605=DIRECTION('center_axis',(-1.,0.,0.));
#20606=DIRECTION('ref_axis',(0.,0.,1.));
#20607=DIRECTION('',(-1.,0.,0.));
#20608=DIRECTION('center_axis',(-1.,0.,0.));
#20609=DIRECTION('ref_axis',(0.,0.,1.));
#20610=DIRECTION('',(-1.,0.,0.));
#20611=DIRECTION('center_axis',(-1.,0.,0.));
#20612=DIRECTION('ref_axis',(0.,0.,1.));
#20613=DIRECTION('center_axis',(-1.,0.,0.));
#20614=DIRECTION('ref_axis',(0.,0.,1.));
#20615=DIRECTION('',(-1.,0.,0.));
#20616=DIRECTION('center_axis',(-1.,0.,0.));
#20617=DIRECTION('ref_axis',(0.,-0.0311419921241395,-0.99951497053648));
#20618=DIRECTION('',(-1.,0.,0.));
#20619=DIRECTION('center_axis',(-1.,0.,0.));
#20620=DIRECTION('ref_axis',(0.,0.,1.));
#20621=DIRECTION('center_axis',(-1.,0.,0.));
#20622=DIRECTION('ref_axis',(0.,0.,1.));
#20623=DIRECTION('',(-1.,0.,0.));
#20624=DIRECTION('center_axis',(-1.,0.,0.));
#20625=DIRECTION('ref_axis',(0.,0.105248670330541,-0.994445934877132));
#20626=DIRECTION('',(-1.,0.,0.));
#20627=DIRECTION('center_axis',(-1.,0.,0.));
#20628=DIRECTION('ref_axis',(0.,0.,1.));
#20629=DIRECTION('center_axis',(-1.,0.,0.));
#20630=DIRECTION('ref_axis',(0.,0.,1.));
#20631=DIRECTION('',(-1.,0.,0.));
#20632=DIRECTION('center_axis',(-1.,0.,0.));
#20633=DIRECTION('ref_axis',(0.,0.,1.));
#20634=DIRECTION('',(-1.,0.,0.));
#20635=DIRECTION('center_axis',(-1.,0.,0.));
#20636=DIRECTION('ref_axis',(0.,0.,1.));
#20637=DIRECTION('center_axis',(-1.,0.,0.));
#20638=DIRECTION('ref_axis',(0.,0.,1.));
#20639=DIRECTION('',(-1.,0.,0.));
#20640=DIRECTION('center_axis',(-1.,0.,0.));
#20641=DIRECTION('ref_axis',(0.,0.,1.));
#20642=DIRECTION('',(-1.,0.,0.));
#20643=DIRECTION('center_axis',(-1.,0.,0.));
#20644=DIRECTION('ref_axis',(0.,0.,1.));
#20645=DIRECTION('center_axis',(-1.,0.,0.));
#20646=DIRECTION('ref_axis',(0.,-0.105248670330508,-0.994445934877136));
#20647=DIRECTION('',(-1.,0.,0.));
#20648=DIRECTION('center_axis',(-1.,0.,0.));
#20649=DIRECTION('ref_axis',(0.,0.,1.));
#20650=DIRECTION('',(-1.,0.,0.));
#20651=DIRECTION('center_axis',(-1.,0.,0.));
#20652=DIRECTION('ref_axis',(0.,0.,1.));
#20653=DIRECTION('center_axis',(-1.,0.,0.));
#20654=DIRECTION('ref_axis',(0.,0.0311419921241608,-0.999514970536479));
#20655=DIRECTION('',(-1.,0.,0.));
#20656=DIRECTION('center_axis',(-1.,0.,0.));
#20657=DIRECTION('ref_axis',(0.,0.,1.));
#20658=DIRECTION('',(-1.,0.,0.));
#20659=DIRECTION('center_axis',(-1.,0.,0.));
#20660=DIRECTION('ref_axis',(0.,0.,1.));
#20661=DIRECTION('center_axis',(-1.,0.,0.));
#20662=DIRECTION('ref_axis',(0.,0.,1.));
#20663=DIRECTION('',(-1.,0.,0.));
#20664=DIRECTION('center_axis',(-1.,0.,0.));
#20665=DIRECTION('ref_axis',(0.,0.,1.));
#20666=DIRECTION('',(-1.,0.,0.));
#20667=DIRECTION('center_axis',(-1.,0.,0.));
#20668=DIRECTION('ref_axis',(0.,0.,1.));
#20669=DIRECTION('center_axis',(-1.,0.,0.));
#20670=DIRECTION('ref_axis',(0.,0.,1.));
#20671=DIRECTION('',(-1.,0.,0.));
#20672=DIRECTION('center_axis',(-1.,0.,0.));
#20673=DIRECTION('ref_axis',(0.,0.,1.));
#20674=DIRECTION('',(-1.,0.,0.));
#20675=DIRECTION('center_axis',(-1.,0.,0.));
#20676=DIRECTION('ref_axis',(0.,0.,1.));
#20677=DIRECTION('center_axis',(-1.,0.,0.));
#20678=DIRECTION('ref_axis',(0.,0.,1.));
#20679=DIRECTION('',(-1.,0.,0.));
#20680=DIRECTION('center_axis',(-1.,0.,0.));
#20681=DIRECTION('ref_axis',(0.,0.,1.));
#20682=DIRECTION('',(-1.,0.,0.));
#20683=DIRECTION('center_axis',(-1.,0.,0.));
#20684=DIRECTION('ref_axis',(0.,0.,1.));
#20685=DIRECTION('center_axis',(-1.,0.,0.));
#20686=DIRECTION('ref_axis',(0.,0.,1.));
#20687=DIRECTION('',(-1.,0.,0.));
#20688=DIRECTION('center_axis',(-1.,0.,0.));
#20689=DIRECTION('ref_axis',(0.,0.,1.));
#20690=DIRECTION('',(-1.,0.,0.));
#20691=DIRECTION('center_axis',(-1.,0.,0.));
#20692=DIRECTION('ref_axis',(0.,0.,1.));
#20693=DIRECTION('center_axis',(-1.,0.,0.));
#20694=DIRECTION('ref_axis',(0.,0.,1.));
#20695=DIRECTION('',(-1.,0.,0.));
#20696=DIRECTION('center_axis',(-1.,0.,0.));
#20697=DIRECTION('ref_axis',(0.,0.,1.));
#20698=DIRECTION('',(-1.,0.,0.));
#20699=DIRECTION('center_axis',(-1.,0.,0.));
#20700=DIRECTION('ref_axis',(0.,0.,1.));
#20701=DIRECTION('center_axis',(-1.,0.,0.));
#20702=DIRECTION('ref_axis',(0.,0.,1.));
#20703=DIRECTION('',(-1.,0.,0.));
#20704=DIRECTION('center_axis',(-1.,0.,0.));
#20705=DIRECTION('ref_axis',(0.,0.,1.));
#20706=DIRECTION('',(-1.,0.,0.));
#20707=DIRECTION('center_axis',(-1.,0.,0.));
#20708=DIRECTION('ref_axis',(0.,0.,1.));
#20709=DIRECTION('center_axis',(-1.,0.,0.));
#20710=DIRECTION('ref_axis',(0.,0.,1.));
#20711=DIRECTION('',(-1.,0.,0.));
#20712=DIRECTION('center_axis',(-1.,0.,0.));
#20713=DIRECTION('ref_axis',(0.,0.,1.));
#20714=DIRECTION('',(-1.,0.,0.));
#20715=DIRECTION('center_axis',(-1.,0.,0.));
#20716=DIRECTION('ref_axis',(0.,0.,1.));
#20717=DIRECTION('center_axis',(-1.,0.,0.));
#20718=DIRECTION('ref_axis',(0.,0.,1.));
#20719=DIRECTION('',(-1.,0.,0.));
#20720=DIRECTION('center_axis',(-1.,0.,0.));
#20721=DIRECTION('ref_axis',(0.,0.,1.));
#20722=DIRECTION('',(-1.,0.,0.));
#20723=DIRECTION('center_axis',(-1.,0.,0.));
#20724=DIRECTION('ref_axis',(0.,0.,1.));
#20725=DIRECTION('center_axis',(-1.,0.,0.));
#20726=DIRECTION('ref_axis',(0.,0.,1.));
#20727=DIRECTION('',(-1.,0.,0.));
#20728=DIRECTION('center_axis',(-1.,0.,0.));
#20729=DIRECTION('ref_axis',(0.,0.,1.));
#20730=DIRECTION('',(-1.,0.,0.));
#20731=DIRECTION('center_axis',(-1.,0.,0.));
#20732=DIRECTION('ref_axis',(0.,0.,1.));
#20733=DIRECTION('center_axis',(-1.,0.,0.));
#20734=DIRECTION('ref_axis',(0.,0.,1.));
#20735=DIRECTION('',(-1.,0.,0.));
#20736=DIRECTION('center_axis',(-1.,0.,0.));
#20737=DIRECTION('ref_axis',(0.,0.,1.));
#20738=DIRECTION('',(-1.,0.,0.));
#20739=DIRECTION('center_axis',(-1.,0.,0.));
#20740=DIRECTION('ref_axis',(0.,0.,1.));
#20741=DIRECTION('center_axis',(-1.,0.,0.));
#20742=DIRECTION('ref_axis',(0.,0.,1.));
#20743=DIRECTION('',(-1.,0.,0.));
#20744=DIRECTION('center_axis',(-1.,0.,0.));
#20745=DIRECTION('ref_axis',(0.,0.,1.));
#20746=DIRECTION('',(-1.,0.,0.));
#20747=DIRECTION('center_axis',(-1.,0.,0.));
#20748=DIRECTION('ref_axis',(0.,0.,1.));
#20749=DIRECTION('center_axis',(-1.,0.,0.));
#20750=DIRECTION('ref_axis',(0.,0.,1.));
#20751=DIRECTION('',(-1.,0.,0.));
#20752=DIRECTION('center_axis',(-1.,0.,0.));
#20753=DIRECTION('ref_axis',(0.,0.,1.));
#20754=DIRECTION('',(-1.,0.,0.));
#20755=DIRECTION('center_axis',(-1.,0.,0.));
#20756=DIRECTION('ref_axis',(0.,0.,1.));
#20757=DIRECTION('center_axis',(-1.,0.,0.));
#20758=DIRECTION('ref_axis',(0.,0.,1.));
#20759=DIRECTION('',(-1.,0.,0.));
#20760=DIRECTION('center_axis',(-1.,0.,0.));
#20761=DIRECTION('ref_axis',(0.,0.,1.));
#20762=DIRECTION('',(-1.,0.,0.));
#20763=DIRECTION('center_axis',(-1.,0.,0.));
#20764=DIRECTION('ref_axis',(0.,0.,1.));
#20765=DIRECTION('center_axis',(-1.,0.,0.));
#20766=DIRECTION('ref_axis',(0.,0.,1.));
#20767=DIRECTION('',(-1.,0.,0.));
#20768=DIRECTION('center_axis',(-1.,0.,0.));
#20769=DIRECTION('ref_axis',(0.,0.,1.));
#20770=DIRECTION('',(-1.,0.,0.));
#20771=DIRECTION('center_axis',(-1.,0.,0.));
#20772=DIRECTION('ref_axis',(0.,0.,1.));
#20773=DIRECTION('center_axis',(-1.,0.,0.));
#20774=DIRECTION('ref_axis',(0.,0.,1.));
#20775=DIRECTION('',(-1.,0.,0.));
#20776=DIRECTION('center_axis',(-1.,0.,0.));
#20777=DIRECTION('ref_axis',(0.,0.,1.));
#20778=DIRECTION('',(-1.,0.,0.));
#20779=DIRECTION('center_axis',(-1.,0.,0.));
#20780=DIRECTION('ref_axis',(0.,0.,1.));
#20781=DIRECTION('center_axis',(-1.,0.,0.));
#20782=DIRECTION('ref_axis',(0.,0.,1.));
#20783=DIRECTION('',(-1.,0.,0.));
#20784=DIRECTION('center_axis',(-1.,0.,0.));
#20785=DIRECTION('ref_axis',(0.,0.,1.));
#20786=DIRECTION('',(-1.,0.,0.));
#20787=DIRECTION('center_axis',(-1.,0.,0.));
#20788=DIRECTION('ref_axis',(0.,0.,1.));
#20789=DIRECTION('center_axis',(-1.,0.,0.));
#20790=DIRECTION('ref_axis',(0.,0.,1.));
#20791=DIRECTION('',(-1.,0.,0.));
#20792=DIRECTION('center_axis',(-1.,0.,0.));
#20793=DIRECTION('ref_axis',(0.,0.,1.));
#20794=DIRECTION('',(-1.,0.,0.));
#20795=DIRECTION('center_axis',(-1.,0.,0.));
#20796=DIRECTION('ref_axis',(0.,0.,1.));
#20797=DIRECTION('center_axis',(-1.,0.,0.));
#20798=DIRECTION('ref_axis',(0.,0.,1.));
#20799=DIRECTION('',(-1.,0.,0.));
#20800=DIRECTION('center_axis',(-1.,0.,0.));
#20801=DIRECTION('ref_axis',(0.,0.,1.));
#20802=DIRECTION('',(-1.,0.,0.));
#20803=DIRECTION('center_axis',(-1.,0.,0.));
#20804=DIRECTION('ref_axis',(0.,0.,1.));
#20805=DIRECTION('center_axis',(-1.,0.,0.));
#20806=DIRECTION('ref_axis',(0.,0.,1.));
#20807=DIRECTION('',(-1.,0.,0.));
#20808=DIRECTION('center_axis',(-1.,0.,0.));
#20809=DIRECTION('ref_axis',(0.,0.,1.));
#20810=DIRECTION('',(-1.,0.,0.));
#20811=DIRECTION('center_axis',(-1.,0.,0.));
#20812=DIRECTION('ref_axis',(0.,0.,1.));
#20813=DIRECTION('center_axis',(-1.,0.,0.));
#20814=DIRECTION('ref_axis',(0.,0.,1.));
#20815=DIRECTION('',(-1.,0.,0.));
#20816=DIRECTION('center_axis',(-1.,0.,0.));
#20817=DIRECTION('ref_axis',(0.,0.,1.));
#20818=DIRECTION('',(-1.,0.,0.));
#20819=DIRECTION('center_axis',(-1.,0.,0.));
#20820=DIRECTION('ref_axis',(0.,0.,1.));
#20821=DIRECTION('center_axis',(-1.,0.,0.));
#20822=DIRECTION('ref_axis',(0.,0.,1.));
#20823=DIRECTION('',(-1.,0.,0.));
#20824=DIRECTION('center_axis',(-1.,0.,0.));
#20825=DIRECTION('ref_axis',(0.,0.,1.));
#20826=DIRECTION('',(-1.,0.,0.));
#20827=DIRECTION('center_axis',(-1.,0.,0.));
#20828=DIRECTION('ref_axis',(0.,0.,1.));
#20829=DIRECTION('center_axis',(-1.,0.,0.));
#20830=DIRECTION('ref_axis',(0.,0.,1.));
#20831=DIRECTION('',(-1.,0.,0.));
#20832=DIRECTION('center_axis',(-1.,0.,0.));
#20833=DIRECTION('ref_axis',(0.,0.,1.));
#20834=DIRECTION('',(-1.,0.,0.));
#20835=DIRECTION('center_axis',(-1.,0.,0.));
#20836=DIRECTION('ref_axis',(0.,0.,1.));
#20837=DIRECTION('center_axis',(-1.,0.,0.));
#20838=DIRECTION('ref_axis',(0.,0.,1.));
#20839=DIRECTION('',(-1.,0.,0.));
#20840=DIRECTION('center_axis',(-1.,0.,0.));
#20841=DIRECTION('ref_axis',(0.,0.,1.));
#20842=DIRECTION('',(-1.,0.,0.));
#20843=DIRECTION('center_axis',(-1.,0.,0.));
#20844=DIRECTION('ref_axis',(0.,0.,1.));
#20845=DIRECTION('center_axis',(-1.,0.,0.));
#20846=DIRECTION('ref_axis',(0.,0.,1.));
#20847=DIRECTION('',(-1.,0.,0.));
#20848=DIRECTION('center_axis',(-1.,0.,0.));
#20849=DIRECTION('ref_axis',(0.,0.,1.));
#20850=DIRECTION('',(-1.,0.,0.));
#20851=DIRECTION('center_axis',(-1.,0.,0.));
#20852=DIRECTION('ref_axis',(0.,0.,1.));
#20853=DIRECTION('center_axis',(-1.,0.,0.));
#20854=DIRECTION('ref_axis',(0.,0.,1.));
#20855=DIRECTION('',(-1.,0.,0.));
#20856=DIRECTION('center_axis',(-1.,0.,0.));
#20857=DIRECTION('ref_axis',(0.,0.,1.));
#20858=DIRECTION('',(-1.,0.,0.));
#20859=DIRECTION('center_axis',(-1.,0.,0.));
#20860=DIRECTION('ref_axis',(0.,0.,1.));
#20861=DIRECTION('center_axis',(-1.,0.,0.));
#20862=DIRECTION('ref_axis',(0.,0.,1.));
#20863=DIRECTION('',(-1.,0.,0.));
#20864=DIRECTION('center_axis',(-1.,0.,0.));
#20865=DIRECTION('ref_axis',(0.,0.,1.));
#20866=DIRECTION('',(-1.,0.,0.));
#20867=DIRECTION('center_axis',(-1.,0.,0.));
#20868=DIRECTION('ref_axis',(0.,0.,1.));
#20869=DIRECTION('center_axis',(-1.,0.,0.));
#20870=DIRECTION('ref_axis',(0.,0.,1.));
#20871=DIRECTION('',(-1.,0.,0.));
#20872=DIRECTION('center_axis',(-1.,0.,0.));
#20873=DIRECTION('ref_axis',(0.,0.,1.));
#20874=DIRECTION('',(-1.,0.,0.));
#20875=DIRECTION('center_axis',(-1.,0.,0.));
#20876=DIRECTION('ref_axis',(0.,0.,1.));
#20877=DIRECTION('center_axis',(-1.,0.,0.));
#20878=DIRECTION('ref_axis',(0.,0.,1.));
#20879=DIRECTION('',(-1.,0.,0.));
#20880=DIRECTION('center_axis',(-1.,0.,0.));
#20881=DIRECTION('ref_axis',(0.,0.,1.));
#20882=DIRECTION('',(-1.,0.,0.));
#20883=DIRECTION('center_axis',(-1.,0.,0.));
#20884=DIRECTION('ref_axis',(0.,0.,1.));
#20885=DIRECTION('center_axis',(-1.,0.,0.));
#20886=DIRECTION('ref_axis',(0.,0.,1.));
#20887=DIRECTION('',(-1.,0.,0.));
#20888=DIRECTION('center_axis',(-1.,0.,0.));
#20889=DIRECTION('ref_axis',(0.,0.,1.));
#20890=DIRECTION('',(-1.,0.,0.));
#20891=DIRECTION('center_axis',(-1.,0.,0.));
#20892=DIRECTION('ref_axis',(0.,0.,1.));
#20893=DIRECTION('center_axis',(-1.,0.,0.));
#20894=DIRECTION('ref_axis',(0.,0.,1.));
#20895=DIRECTION('',(-1.,0.,0.));
#20896=DIRECTION('center_axis',(-1.,0.,0.));
#20897=DIRECTION('ref_axis',(0.,0.,1.));
#20898=DIRECTION('',(-1.,0.,0.));
#20899=DIRECTION('center_axis',(-1.,0.,0.));
#20900=DIRECTION('ref_axis',(0.,0.,1.));
#20901=DIRECTION('center_axis',(-1.,0.,0.));
#20902=DIRECTION('ref_axis',(0.,0.,1.));
#20903=DIRECTION('',(-1.,0.,0.));
#20904=DIRECTION('axis',(0.,0.,1.));
#20905=DIRECTION('refdir',(1.,0.,0.));
#20906=DIRECTION('center_axis',(1.,0.,0.));
#20907=DIRECTION('ref_axis',(0.,0.,-1.));
#20908=DIRECTION('center_axis',(-1.,0.,0.));
#20909=DIRECTION('ref_axis',(0.,0.,1.));
#20910=DIRECTION('center_axis',(-1.,0.,0.));
#20911=DIRECTION('ref_axis',(0.,0.,1.));
#20912=DIRECTION('',(1.,0.,0.));
#20913=DIRECTION('center_axis',(-1.,0.,0.));
#20914=DIRECTION('ref_axis',(0.,0.,1.));
#20915=DIRECTION('center_axis',(-1.,0.,0.));
#20916=DIRECTION('ref_axis',(0.,0.,1.));
#20917=DIRECTION('center_axis',(1.,0.,0.));
#20918=DIRECTION('ref_axis',(0.,0.,-1.));
#20919=DIRECTION('center_axis',(-1.,0.,0.));
#20920=DIRECTION('ref_axis',(0.,0.,1.));
#20921=DIRECTION('',(-1.,0.,0.));
#20922=DIRECTION('center_axis',(-1.,0.,0.));
#20923=DIRECTION('ref_axis',(0.,0.,1.));
#20924=DIRECTION('center_axis',(-1.,0.,0.));
#20925=DIRECTION('ref_axis',(0.,0.,1.));
#20926=DIRECTION('center_axis',(1.,0.,0.));
#20927=DIRECTION('ref_axis',(0.,0.,-1.));
#20928=DIRECTION('center_axis',(-1.,0.,0.));
#20929=DIRECTION('ref_axis',(0.,0.,1.));
#20930=DIRECTION('center_axis',(-1.,0.,0.));
#20931=DIRECTION('ref_axis',(0.,0.,1.));
#20932=DIRECTION('',(-1.,0.,0.));
#20933=DIRECTION('center_axis',(-1.,0.,0.));
#20934=DIRECTION('ref_axis',(0.,0.,1.));
#20935=DIRECTION('center_axis',(-1.,0.,0.));
#20936=DIRECTION('ref_axis',(0.,0.,1.));
#20937=DIRECTION('center_axis',(1.,0.,0.));
#20938=DIRECTION('ref_axis',(0.,0.,-1.));
#20939=DIRECTION('center_axis',(1.,0.,0.));
#20940=DIRECTION('ref_axis',(0.,0.,-1.));
#20941=DIRECTION('',(-1.,0.,0.));
#20942=DIRECTION('center_axis',(-1.,0.,0.));
#20943=DIRECTION('ref_axis',(0.,0.,1.));
#20944=DIRECTION('center_axis',(-1.,0.,0.));
#20945=DIRECTION('ref_axis',(0.,0.,1.));
#20946=DIRECTION('center_axis',(-1.,0.,0.));
#20947=DIRECTION('ref_axis',(0.,0.,1.));
#20948=DIRECTION('center_axis',(-1.,0.,0.));
#20949=DIRECTION('ref_axis',(0.,0.,1.));
#20950=DIRECTION('center_axis',(-1.,0.,0.));
#20951=DIRECTION('ref_axis',(0.,0.,1.));
#20952=DIRECTION('center_axis',(-1.,0.,0.));
#20953=DIRECTION('ref_axis',(0.,0.,1.));
#20954=DIRECTION('center_axis',(-1.,0.,0.));
#20955=DIRECTION('ref_axis',(0.,0.,1.));
#20956=DIRECTION('center_axis',(1.,0.,0.));
#20957=DIRECTION('ref_axis',(0.,0.,-1.));
#20958=DIRECTION('center_axis',(1.,0.,0.));
#20959=DIRECTION('ref_axis',(0.,0.,-1.));
#20960=DIRECTION('center_axis',(1.,0.,0.));
#20961=DIRECTION('ref_axis',(0.,0.,-1.));
#20962=DIRECTION('',(-1.,0.,0.));
#20963=DIRECTION('center_axis',(1.,0.,0.));
#20964=DIRECTION('ref_axis',(0.,0.,-1.));
#20965=DIRECTION('center_axis',(1.,0.,0.));
#20966=DIRECTION('ref_axis',(0.,0.,-1.));
#20967=DIRECTION('center_axis',(1.,0.,0.));
#20968=DIRECTION('ref_axis',(0.,0.,-1.));
#20969=DIRECTION('center_axis',(1.,0.,0.));
#20970=DIRECTION('ref_axis',(0.,0.,-1.));
#20971=DIRECTION('',(-1.,0.,0.));
#20972=DIRECTION('center_axis',(1.,0.,0.));
#20973=DIRECTION('ref_axis',(0.,0.,-1.));
#20974=DIRECTION('center_axis',(1.,0.,0.));
#20975=DIRECTION('ref_axis',(0.,0.,-1.));
#20976=DIRECTION('center_axis',(1.,0.,0.));
#20977=DIRECTION('ref_axis',(0.,0.,-1.));
#20978=DIRECTION('',(-1.,0.,0.));
#20979=DIRECTION('center_axis',(-1.,0.,0.));
#20980=DIRECTION('ref_axis',(0.,0.,1.));
#20981=DIRECTION('center_axis',(-1.,0.,0.));
#20982=DIRECTION('ref_axis',(0.,0.,1.));
#20983=DIRECTION('center_axis',(1.,0.,0.));
#20984=DIRECTION('ref_axis',(0.,0.,-1.));
#20985=DIRECTION('center_axis',(1.,0.,0.));
#20986=DIRECTION('ref_axis',(0.,0.,-1.));
#20987=DIRECTION('',(-1.,0.,0.));
#20988=DIRECTION('center_axis',(-1.,0.,0.));
#20989=DIRECTION('ref_axis',(0.,0.,1.));
#20990=DIRECTION('center_axis',(-1.,0.,0.));
#20991=DIRECTION('ref_axis',(0.,0.,1.));
#20992=DIRECTION('center_axis',(1.,0.,0.));
#20993=DIRECTION('ref_axis',(0.,0.,-1.));
#20994=DIRECTION('center_axis',(1.,0.,0.));
#20995=DIRECTION('ref_axis',(0.,0.,-1.));
#20996=DIRECTION('center_axis',(1.,0.,0.));
#20997=DIRECTION('ref_axis',(0.,0.,-1.));
#20998=DIRECTION('',(-1.,0.,0.));
#20999=DIRECTION('center_axis',(1.,0.,0.));
#21000=DIRECTION('ref_axis',(0.,0.,-1.));
#21001=DIRECTION('center_axis',(1.,0.,0.));
#21002=DIRECTION('ref_axis',(0.,0.,-1.));
#21003=DIRECTION('center_axis',(1.,0.,0.));
#21004=DIRECTION('ref_axis',(0.,0.,-1.));
#21005=DIRECTION('center_axis',(1.,0.,0.));
#21006=DIRECTION('ref_axis',(0.,0.,-1.));
#21007=DIRECTION('',(-1.,0.,0.));
#21008=DIRECTION('center_axis',(1.,0.,0.));
#21009=DIRECTION('ref_axis',(0.,0.,-1.));
#21010=DIRECTION('center_axis',(1.,0.,0.));
#21011=DIRECTION('ref_axis',(0.,0.,-1.));
#21012=DIRECTION('center_axis',(1.,0.,0.));
#21013=DIRECTION('ref_axis',(0.,0.,-1.));
#21014=DIRECTION('',(-1.,0.,0.));
#21015=DIRECTION('center_axis',(-1.,0.,0.));
#21016=DIRECTION('ref_axis',(0.,0.,1.));
#21017=DIRECTION('center_axis',(-1.,0.,0.));
#21018=DIRECTION('ref_axis',(0.,0.,1.));
#21019=DIRECTION('center_axis',(1.,0.,0.));
#21020=DIRECTION('ref_axis',(0.,0.,-1.));
#21021=DIRECTION('center_axis',(1.,0.,0.));
#21022=DIRECTION('ref_axis',(0.,0.,-1.));
#21023=DIRECTION('center_axis',(1.,0.,0.));
#21024=DIRECTION('ref_axis',(0.,0.,-1.));
#21025=DIRECTION('',(-1.,0.,0.));
#21026=DIRECTION('center_axis',(1.,0.,0.));
#21027=DIRECTION('ref_axis',(0.,0.,-1.));
#21028=DIRECTION('center_axis',(1.,0.,0.));
#21029=DIRECTION('ref_axis',(0.,0.,-1.));
#21030=DIRECTION('center_axis',(1.,0.,0.));
#21031=DIRECTION('ref_axis',(0.,0.,-1.));
#21032=DIRECTION('',(-1.,0.,0.));
#21033=DIRECTION('center_axis',(-1.,0.,0.));
#21034=DIRECTION('ref_axis',(0.,0.,1.));
#21035=DIRECTION('center_axis',(-1.,0.,0.));
#21036=DIRECTION('ref_axis',(0.,0.,1.));
#21037=DIRECTION('center_axis',(1.,0.,0.));
#21038=DIRECTION('ref_axis',(0.,0.,-1.));
#21039=DIRECTION('center_axis',(1.,0.,0.));
#21040=DIRECTION('ref_axis',(0.,0.,-1.));
#21041=DIRECTION('center_axis',(1.,0.,0.));
#21042=DIRECTION('ref_axis',(0.,0.,-1.));
#21043=DIRECTION('',(-1.,0.,0.));
#21044=DIRECTION('center_axis',(1.,0.,0.));
#21045=DIRECTION('ref_axis',(0.,0.,-1.));
#21046=DIRECTION('center_axis',(1.,0.,0.));
#21047=DIRECTION('ref_axis',(0.,0.,-1.));
#21048=DIRECTION('center_axis',(1.,0.,0.));
#21049=DIRECTION('ref_axis',(0.,0.,-1.));
#21050=DIRECTION('',(-1.,0.,0.));
#21051=DIRECTION('center_axis',(-1.,0.,0.));
#21052=DIRECTION('ref_axis',(0.,0.,1.));
#21053=DIRECTION('center_axis',(-1.,0.,0.));
#21054=DIRECTION('ref_axis',(0.,0.,1.));
#21055=DIRECTION('center_axis',(1.,0.,0.));
#21056=DIRECTION('ref_axis',(0.,0.,-1.));
#21057=DIRECTION('center_axis',(1.,0.,0.));
#21058=DIRECTION('ref_axis',(0.,0.,-1.));
#21059=DIRECTION('center_axis',(1.,0.,0.));
#21060=DIRECTION('ref_axis',(0.,0.,-1.));
#21061=DIRECTION('',(-1.,0.,0.));
#21062=DIRECTION('center_axis',(1.,0.,0.));
#21063=DIRECTION('ref_axis',(0.,0.,-1.));
#21064=DIRECTION('center_axis',(1.,0.,0.));
#21065=DIRECTION('ref_axis',(0.,0.,-1.));
#21066=DIRECTION('center_axis',(1.,0.,0.));
#21067=DIRECTION('ref_axis',(0.,0.,-1.));
#21068=DIRECTION('',(-1.,0.,0.));
#21069=DIRECTION('center_axis',(-1.,0.,0.));
#21070=DIRECTION('ref_axis',(0.,0.,1.));
#21071=DIRECTION('center_axis',(-1.,0.,0.));
#21072=DIRECTION('ref_axis',(0.,0.,1.));
#21073=DIRECTION('center_axis',(-1.,0.,0.));
#21074=DIRECTION('ref_axis',(0.,0.,1.));
#21075=DIRECTION('center_axis',(-1.,0.,0.));
#21076=DIRECTION('ref_axis',(0.,0.,1.));
#21077=DIRECTION('center_axis',(-1.,0.,0.));
#21078=DIRECTION('ref_axis',(0.,0.,1.));
#21079=DIRECTION('center_axis',(-1.,0.,0.));
#21080=DIRECTION('ref_axis',(0.,0.,1.));
#21081=DIRECTION('center_axis',(-1.,0.,0.));
#21082=DIRECTION('ref_axis',(0.,0.,1.));
#21083=DIRECTION('center_axis',(-5.01652904731627E-15,2.04600742668907E-13,
1.));
#21084=DIRECTION('ref_axis',(0.,-1.,2.04600742668907E-13));
#21085=DIRECTION('center_axis',(0.999999999999512,3.64455443991191E-10,
9.88227092522604E-7));
#21086=DIRECTION('ref_axis',(-9.88227091978951E-7,2.02026683180761E-10,
0.999999999999512));
#21087=DIRECTION('center_axis',(0.999999999999512,-3.64455669902473E-10,
-9.88227186270797E-7));
#21088=DIRECTION('ref_axis',(-9.88227185993996E-7,0.,-0.999999999999512));
#21089=DIRECTION('center_axis',(3.96697174057741E-14,2.06573350065547E-12,
1.));
#21090=DIRECTION('ref_axis',(0.,-1.,2.06573350065547E-12));
#21091=DIRECTION('center_axis',(-1.,0.,0.));
#21092=DIRECTION('ref_axis',(0.,0.,1.));
#21093=DIRECTION('center_axis',(0.,1.,-1.30989755110808E-16));
#21094=DIRECTION('ref_axis',(0.,-1.30989755110808E-16,-1.));
#21095=DIRECTION('center_axis',(-1.,0.,0.));
#21096=DIRECTION('ref_axis',(0.,0.,1.));
#21097=DIRECTION('center_axis',(0.,1.,-2.22044604925031E-16));
#21098=DIRECTION('ref_axis',(0.,-2.22044604925031E-16,-1.));
#21099=DIRECTION('center_axis',(-1.,0.,0.));
#21100=DIRECTION('ref_axis',(0.,0.,1.));
#21101=DIRECTION('center_axis',(0.,-1.,1.85037170770859E-16));
#21102=DIRECTION('ref_axis',(0.,-1.85037170770859E-16,-1.));
#21103=DIRECTION('center_axis',(-1.,0.,0.));
#21104=DIRECTION('ref_axis',(0.,0.,1.));
#21105=DIRECTION('center_axis',(0.,-1.,1.19009136371855E-16));
#21106=DIRECTION('ref_axis',(0.,-1.19009136371855E-16,-1.));
#21107=DIRECTION('center_axis',(-1.,0.,0.));
#21108=DIRECTION('ref_axis',(0.,0.,1.));
#21109=DIRECTION('center_axis',(0.,-1.,1.19009136371855E-16));
#21110=DIRECTION('ref_axis',(0.,-1.19009136371855E-16,-1.));
#21111=DIRECTION('center_axis',(-1.,0.,0.));
#21112=DIRECTION('ref_axis',(0.,0.,1.));
#21113=DIRECTION('center_axis',(0.,-1.,1.19009136371855E-16));
#21114=DIRECTION('ref_axis',(0.,-1.19009136371855E-16,-1.));
#21115=DIRECTION('center_axis',(1.,0.,0.));
#21116=DIRECTION('ref_axis',(0.,0.,-1.));
#21117=DIRECTION('center_axis',(0.,-1.,-1.19009136371855E-16));
#21118=DIRECTION('ref_axis',(0.,-1.19009136371855E-16,1.));
#21119=DIRECTION('center_axis',(-1.,0.,0.));
#21120=DIRECTION('ref_axis',(0.,0.,1.));
#21121=DIRECTION('center_axis',(0.,-1.,1.19009136371855E-16));
#21122=DIRECTION('ref_axis',(0.,-1.19009136371855E-16,-1.));
#21123=DIRECTION('center_axis',(1.,0.,0.));
#21124=DIRECTION('ref_axis',(0.,0.,-1.));
#21125=DIRECTION('center_axis',(0.,-1.,-1.19009136371855E-16));
#21126=DIRECTION('ref_axis',(0.,-1.19009136371855E-16,1.));
#21127=DIRECTION('center_axis',(-1.,0.,0.));
#21128=DIRECTION('ref_axis',(0.,0.,1.));
#21129=DIRECTION('center_axis',(0.,-1.,1.19009136371855E-16));
#21130=DIRECTION('ref_axis',(0.,-1.19009136371855E-16,-1.));
#21131=DIRECTION('center_axis',(1.,0.,0.));
#21132=DIRECTION('ref_axis',(0.,0.,-1.));
#21133=DIRECTION('center_axis',(0.,-1.,-1.19009136371855E-16));
#21134=DIRECTION('ref_axis',(0.,-1.19009136371855E-16,1.));
#21135=DIRECTION('center_axis',(1.,0.,0.));
#21136=DIRECTION('ref_axis',(0.,0.,-1.));
#21137=DIRECTION('center_axis',(0.,-1.,-1.19009136371855E-16));
#21138=DIRECTION('ref_axis',(0.,-1.19009136371855E-16,1.));
#21139=DIRECTION('center_axis',(-1.,0.,0.));
#21140=DIRECTION('ref_axis',(0.,0.,1.));
#21141=DIRECTION('center_axis',(0.,-1.,1.19009136371855E-16));
#21142=DIRECTION('ref_axis',(0.,-1.19009136371855E-16,-1.));
#21143=DIRECTION('center_axis',(1.,0.,0.));
#21144=DIRECTION('ref_axis',(0.,0.,-1.));
#21145=DIRECTION('center_axis',(0.,-1.,-1.19009136371855E-16));
#21146=DIRECTION('ref_axis',(0.,-1.19009136371855E-16,1.));
#21147=DIRECTION('center_axis',(-1.,0.,0.));
#21148=DIRECTION('ref_axis',(0.,0.,1.));
#21149=DIRECTION('center_axis',(0.,-1.,1.19009136371855E-16));
#21150=DIRECTION('ref_axis',(0.,-1.19009136371855E-16,-1.));
#21151=DIRECTION('center_axis',(-1.,0.,0.));
#21152=DIRECTION('ref_axis',(0.,0.,1.));
#21153=DIRECTION('center_axis',(0.,-1.,1.19009136371855E-16));
#21154=DIRECTION('ref_axis',(0.,-1.19009136371855E-16,-1.));
#21155=DIRECTION('center_axis',(1.,0.,0.));
#21156=DIRECTION('ref_axis',(0.,0.,-1.));
#21157=DIRECTION('center_axis',(0.,-1.,-1.19009136371855E-16));
#21158=DIRECTION('ref_axis',(0.,-1.19009136371855E-16,1.));
#21159=DIRECTION('center_axis',(-1.,0.,0.));
#21160=DIRECTION('ref_axis',(0.,0.,1.));
#21161=DIRECTION('center_axis',(0.,-1.,1.19009136371855E-16));
#21162=DIRECTION('ref_axis',(0.,-1.19009136371855E-16,-1.));
#21163=DIRECTION('center_axis',(1.,0.,0.));
#21164=DIRECTION('ref_axis',(0.,0.,-1.));
#21165=DIRECTION('center_axis',(0.,-1.,-1.19009136371855E-16));
#21166=DIRECTION('ref_axis',(0.,-1.19009136371855E-16,1.));
#21167=DIRECTION('axis',(0.,0.,1.));
#21168=DIRECTION('refdir',(1.,0.,0.));
#21169=DIRECTION('center_axis',(0.,1.,0.));
#21170=DIRECTION('ref_axis',(1.,0.,0.));
#21171=DIRECTION('center_axis',(1.22464679914735E-16,1.97778073784536E-32,
1.));
#21172=DIRECTION('ref_axis',(-1.,0.,1.22464679914735E-16));
#21173=DIRECTION('axis',(0.,0.,1.));
#21174=DIRECTION('refdir',(1.,0.,0.));
#21175=DIRECTION('center_axis',(0.0825919163630432,-0.996583451272946,6.19384420193564E-7));
#21176=DIRECTION('ref_axis',(0.765754157887476,0.0634623218806236,0.639994611992603));
#21177=DIRECTION('center_axis',(0.966179703385848,0.0733338853286848,-0.247222414088678));
#21178=DIRECTION('ref_axis',(0.153476402600925,0.606887091524721,0.779828860703003));
#21179=DIRECTION('',(-0.999797265210905,-0.00157571520789441,0.0200735048852593));
#21180=DIRECTION('',(-0.999795009940132,-0.00177423967236348,0.0201690399472964));
#21181=DIRECTION('',(-0.999814419433609,-0.00074299116254352,0.0192503157576034));
#21182=DIRECTION('',(-0.99930375064088,0.0370923483029995,-0.00402139931355867));
#21183=DIRECTION('',(0.999799569502936,0.000143273756301408,-0.0200199973619988));
#21184=DIRECTION('',(0.999795159155772,0.000550483968732209,-0.0202320709786369));
#21185=DIRECTION('',(0.999794381564603,0.000677070304206123,-0.0202666269432168));
#21186=DIRECTION('',(0.999794667552926,0.00072470430475225,-0.0202508650779472));
#21187=DIRECTION('',(0.99979559762733,0.000724626511420293,-0.0202048974614902));
#21188=DIRECTION('',(0.999794934842533,0.000845975517364629,-0.0202329579804895));
#21189=DIRECTION('',(0.999795478082445,0.000877544516035547,-0.0202047499741565));
#21190=DIRECTION('',(0.999792750698211,0.00115574151218025,-0.02032535148188));
#21191=DIRECTION('',(0.999796795370114,0.000927130164533834,-0.0201372390686534));
#21192=DIRECTION('',(0.999789554301239,0.00153991797600282,-0.0204566801499491));
#21193=DIRECTION('',(0.999799696863398,0.000859242700217791,-0.0199956958828443));
#21194=DIRECTION('center_axis',(-0.966520755854356,0.0727166375962521,0.246068931641969));
#21195=DIRECTION('ref_axis',(0.15568482121692,-0.596109982412235,0.787664348127514));
#21196=DIRECTION('center_axis',(0.965616313298931,-0.0694925699401865,-0.250511313545094));
#21197=DIRECTION('ref_axis',(0.147415368320144,-0.647349895074982,0.747801325573475));
#21198=DIRECTION('center_axis',(0.999750119804914,-3.4619426304031E-5,-0.0223538979051964));
#21199=DIRECTION('ref_axis',(0.0223537576222625,-0.00231815432474148,0.999747435946045));
#21200=DIRECTION('',(-0.999798518286744,0.000907194296559704,0.0200524270386368));
#21201=DIRECTION('',(-0.999797847151546,0.000882664687892492,0.0200869543281969));
#21202=DIRECTION('',(-0.999794527097293,0.00105818090835443,0.020243118323649));
#21203=DIRECTION('',(-0.999793960532759,0.00102594036328993,0.0202727385567707));
#21204=DIRECTION('',(-0.99979281884068,0.00103697298612291,0.0203284057819104));
#21205=DIRECTION('',(-0.999790073544858,0.00116543286722787,0.0204560652961453));
#21206=DIRECTION('',(-0.999792172359634,0.000941112379170086,0.0203648323315679));
#21207=DIRECTION('',(-0.999792286411407,0.000862374111952732,0.0203627194436703));
#21208=DIRECTION('',(-0.999788908874571,0.00103939132471049,0.0205196821873228));
#21209=DIRECTION('',(-0.999783724751033,0.00133812018306296,0.0207536299794865));
#21210=DIRECTION('',(-0.999792998568771,0.000603868432621,0.0203370439292827));
#21211=DIRECTION('',(0.999255736399573,0.0382175248776868,0.00523393396688128));
#21212=DIRECTION('',(0.999811045660937,-0.000922877743517363,-0.019417035588743));
#21213=DIRECTION('',(0.999809716706824,-0.000927106074859977,-0.0194851444168618));
#21214=DIRECTION('',(0.999816314546287,-0.000464324184849131,-0.0191604167525331));
#21215=DIRECTION('center_axis',(0.96683239686865,-0.0708748078028809,-0.245381087258425));
#21216=DIRECTION('ref_axis',(0.140042328661989,-0.656336014011258,0.741357661924891));
#21217=DIRECTION('center_axis',(0.957113823248678,-0.0400659616184508,0.286928297778184));
#21218=DIRECTION('ref_axis',(0.204108305786598,-0.609609959396545,-0.765973561497698));
#21219=DIRECTION('',(-0.999796968581146,0.00159150450853508,-0.0200870288830814));
#21220=DIRECTION('center_axis',(-0.965247781539032,0.0691046739050647,-0.252034252192936));
#21221=DIRECTION('ref_axis',(0.146842758004779,-0.654350158212197,-0.741797192546064));
#21222=DIRECTION('',(0.999816280485641,0.000465769226166559,0.0191621589307047));
#21223=DIRECTION('center_axis',(0.966757680149406,0.0705404390428106,0.245771508380827));
#21224=DIRECTION('ref_axis',(0.140547052978298,0.656363572024975,-0.741237740011753));
#21225=DIRECTION('',(0.999794903114167,-0.000848133911591957,0.0202344353961459));
#21226=DIRECTION('',(-0.999790098322183,-0.00116340831296703,-0.020454969518826));
#21227=DIRECTION('',(0.999795574158484,-0.000726169871118148,0.02020600332638));
#21228=DIRECTION('',(-0.999792175797662,-0.000940634061937126,-0.0203646856430204));
#21229=DIRECTION('',(0.999794642017327,-0.000726392539479541,0.0202520652607186));
#21230=DIRECTION('',(-0.999792264776137,-0.000863745000872394,-0.0203637235881719));
#21231=DIRECTION('',(0.999794385721742,-0.000676521551207557,0.0202664401875626));
#21232=DIRECTION('',(-0.999788865344958,-0.00104230550305824,-0.0205216551837372));
#21233=DIRECTION('',(0.999799527208902,-0.000872277300359709,0.0200036128028985));
#21234=DIRECTION('',(-0.9997980790357,-0.000940170020731757,-0.0200727984311172));
#21235=DIRECTION('',(0.999799571229728,-0.000142906932253215,0.0200199137476009));
#21236=DIRECTION('',(-0.999792941420028,-0.000607873253951516,-0.0203397339411044));
#21237=DIRECTION('',(-0.99979517235786,0.00176498749919714,-0.020161799251162));
#21238=DIRECTION('',(0.999809462767171,0.000941297182692076,0.0194974901162665));
#21239=DIRECTION('',(0.999795158107842,-0.000550333259916924,0.0202321268634491));
#21240=DIRECTION('',(-0.999783669579685,-0.00134174073953075,-0.020756053901623));
#21241=DIRECTION('',(0.999795442584518,-0.000879999821241033,0.020206399667981));
#21242=DIRECTION('',(-0.999792869478343,-0.00103298086046051,-0.0203261184391759));
#21243=DIRECTION('',(0.999792702399425,-0.00115909618973122,0.0203275361241377));
#21244=DIRECTION('',(-0.999794065485702,-0.00101784417227304,-0.0202679701206788));
#21245=DIRECTION('',(0.999796734453382,-0.000931561542189858,0.0201400588243195));
#21246=DIRECTION('',(-0.999794878993418,-0.00103154307653973,-0.0202271069957695));
#21247=DIRECTION('',(0.99978945409093,-0.00154695287703341,0.020461046536212));
#21248=DIRECTION('',(-0.99979917188903,-0.00078031983021078,-0.0200251589500104));
#21249=DIRECTION('',(-0.999814422778328,0.000742280540990978,-0.0192501694547673));
#21250=DIRECTION('',(0.999810938682864,0.000928619335546645,0.0194222695949644));
#21251=DIRECTION('',(-0.999303691614598,-0.0370938856343022,0.00402188686874901));
#21252=DIRECTION('',(0.999255934071334,-0.0382128842081673,-0.0052300768368433));
#21253=DIRECTION('',(0.0225950194900106,-0.0017788380133363,0.999743117420454));
#21254=DIRECTION('',(-0.0208097837600092,0.313767956481563,-0.94927162729392));
#21255=DIRECTION('center_axis',(-0.974667565771182,0.0286954385344785,-0.221810072000784));
#21256=DIRECTION('ref_axis',(-0.221901450770903,4.90925569561603E-18,0.975069098139085));
#21257=DIRECTION('center_axis',(6.93889390390723E-16,0.,1.));
#21258=DIRECTION('ref_axis',(1.,0.,-6.93889390390723E-16));
#21259=DIRECTION('center_axis',(6.93889390390723E-16,0.,1.));
#21260=DIRECTION('ref_axis',(1.,0.,-6.93889390390723E-16));
#21261=DIRECTION('',(0.,1.,0.));
#21262=DIRECTION('center_axis',(6.93889390390723E-16,0.,1.));
#21263=DIRECTION('ref_axis',(1.,0.,-6.93889390390723E-16));
#21264=DIRECTION('',(0.,1.,0.));
#21265=DIRECTION('center_axis',(6.93889390390723E-16,0.,1.));
#21266=DIRECTION('ref_axis',(1.,0.,-6.93889390390723E-16));
#21267=DIRECTION('center_axis',(6.93889390390723E-16,0.,-1.));
#21268=DIRECTION('ref_axis',(-1.,0.,-6.93889390390723E-16));
#21269=DIRECTION('',(0.,1.,0.));
#21270=DIRECTION('center_axis',(6.93889390390723E-16,0.,-1.));
#21271=DIRECTION('ref_axis',(-1.,0.,-6.93889390390723E-16));
#21272=DIRECTION('center_axis',(6.93889390390723E-16,0.,-1.));
#21273=DIRECTION('ref_axis',(-1.,0.,-6.93889390390723E-16));
#21274=DIRECTION('',(0.,1.,0.));
#21275=DIRECTION('center_axis',(0.999750166148961,-4.73635043611131E-5,
0.0223518017578594));
#21276=DIRECTION('ref_axis',(0.0223518017829303,3.33694979789914E-21,-0.999750167270332));
#21277=DIRECTION('center_axis',(0.0825919163630432,-0.996583451272946,6.19384420193564E-7));
#21278=DIRECTION('ref_axis',(0.765754157887476,0.0634623218806236,0.639994611992603));
#21279=DIRECTION('center_axis',(0.0825919165140713,0.996583451260439,-6.0402864252192E-7));
#21280=DIRECTION('ref_axis',(0.765754157790578,-0.0634623121281307,-0.639994613075606));
#21281=DIRECTION('center_axis',(-0.98075579440661,5.32973170040097E-6,0.195238499557471));
#21282=DIRECTION('ref_axis',(0.19443017895973,0.0909288071299902,0.976692816367359));
#21283=DIRECTION('center_axis',(-0.981482829121148,-3.75634276483288E-6,
-0.191550139979688));
#21284=DIRECTION('ref_axis',(0.190757106872796,-0.0909203347980143,-0.977417627679048));
#21285=DIRECTION('center_axis',(-4.86886864449402E-15,1.,-2.1379377376203E-14));
#21286=DIRECTION('ref_axis',(-4.04680781916367E-45,2.1379377376203E-14,
1.));
#21287=DIRECTION('center_axis',(0.,1.,0.));
#21288=DIRECTION('ref_axis',(-1.,0.,-4.22123945207479E-11));
#21289=DIRECTION('center_axis',(0.,1.,0.));
#21290=DIRECTION('ref_axis',(-1.,0.,-2.83604770904466E-14));
#21291=DIRECTION('center_axis',(1.47522099208952E-16,1.,-6.09726439183545E-15));
#21292=DIRECTION('ref_axis',(8.40782393547547E-47,6.09726439183545E-15,
1.));
#21293=DIRECTION('center_axis',(0.982692008587054,-0.00050387605033863,
0.185246220927898));
#21294=DIRECTION('ref_axis',(-0.0160368225195314,-0.996473482954562,0.0823615085575891));
#21295=DIRECTION('center_axis',(0.76964097577498,0.,-0.638476912979738));
#21296=DIRECTION('ref_axis',(-0.638476912979738,0.,-0.76964097577498));
#21297=DIRECTION('',(0.,1.,0.));
#21298=DIRECTION('',(0.,1.,0.));
#21299=DIRECTION('center_axis',(0.,1.,0.));
#21300=DIRECTION('ref_axis',(0.,0.,1.));
#21301=DIRECTION('',(0.,1.,0.));
#21302=DIRECTION('center_axis',(0.,1.,0.));
#21303=DIRECTION('ref_axis',(0.,0.,1.));
#21304=DIRECTION('',(0.,1.,0.));
#21305=DIRECTION('center_axis',(0.76964097577498,0.,0.638476912979738));
#21306=DIRECTION('ref_axis',(0.638476912979738,0.,-0.76964097577498));
#21307=DIRECTION('center_axis',(0.,0.,1.));
#21308=DIRECTION('ref_axis',(1.,0.,0.));
#21309=DIRECTION('center_axis',(6.93889390390723E-16,0.,-1.));
#21310=DIRECTION('ref_axis',(-1.,0.,-6.93889390390723E-16));
#21311=DIRECTION('center_axis',(0.,0.,1.));
#21312=DIRECTION('ref_axis',(1.,0.,0.));
#21313=DIRECTION('center_axis',(0.,0.,1.));
#21314=DIRECTION('ref_axis',(1.,0.,0.));
#21315=DIRECTION('center_axis',(6.93889390390723E-16,0.,1.));
#21316=DIRECTION('ref_axis',(1.,0.,-6.93889390390723E-16));
#21317=DIRECTION('center_axis',(0.,0.,1.));
#21318=DIRECTION('ref_axis',(1.,0.,0.));
#21319=DIRECTION('center_axis',(6.93889390390723E-16,0.,1.));
#21320=DIRECTION('ref_axis',(1.,0.,-6.93889390390723E-16));
#21321=DIRECTION('center_axis',(0.999993789125747,0.00350648594152928,-0.000355339658387565));
#21322=DIRECTION('ref_axis',(-0.00326396958594675,0.883331083394255,-0.468738246372188));
#21323=DIRECTION('center_axis',(0.99999378903564,0.00350650862306363,0.00035536941415181));
#21324=DIRECTION('ref_axis',(-0.000355367205935845,-1.25282104470708E-6,
0.999999936856288));
#21325=DIRECTION('center_axis',(0.999992536376844,0.00385800221437534,0.000207387369863947));
#21326=DIRECTION('ref_axis',(-0.00385800229734076,0.999992557881444,0.));
#21327=DIRECTION('center_axis',(0.999992536598678,0.00385794601180392,-0.000207363237830676));
#21328=DIRECTION('ref_axis',(-0.00385794609474882,0.999992558098274,0.));
#21329=DIRECTION('center_axis',(0.999990310769996,0.00440207548560395,-9.87651888418822E-6));
#21330=DIRECTION('ref_axis',(-0.0036207108715852,0.821212665146659,-0.570610768436336));
#21331=DIRECTION('center_axis',(-0.909784343381186,-0.228750702611131,-0.346360454719326));
#21332=DIRECTION('ref_axis',(-0.355794328393026,3.2321890514358E-17,0.93456428130084));
#21333=DIRECTION('center_axis',(0.981482840368801,6.94690961148907E-5,0.191550069787602));
#21334=DIRECTION('ref_axis',(0.191550070249807,0.,-0.981482842737098));
#21335=DIRECTION('center_axis',(0.98075583355353,-0.000125702323698021,
-0.195238262514414));
#21336=DIRECTION('ref_axis',(0.195238265280273,1.00024838000881E-5,0.980755841007485));
#21337=DIRECTION('center_axis',(-0.909784105944603,0.228750295766247,0.346361347089185));
#21338=DIRECTION('ref_axis',(0.355795210127735,-5.10614014417012E-17,0.934563945618576));
#21339=DIRECTION('center_axis',(0.909784343381305,-0.228750702611003,0.346360454719098));
#21340=DIRECTION('ref_axis',(0.355794328392781,1.06760012694273E-16,-0.934564281300933));
#21341=DIRECTION('center_axis',(0.999992536382172,-0.00385800090220185,
0.000207386085645872));
#21342=DIRECTION('ref_axis',(0.00385800098516621,0.999992557886507,0.));
#21343=DIRECTION('center_axis',(0.999990310574524,-0.00440211987885248,
9.88122079760886E-6));
#21344=DIRECTION('ref_axis',(-0.00362072769721535,-0.821207579688302,0.570618087159375));
#21345=DIRECTION('center_axis',(0.999993789045476,-0.00350650580089381,
0.000355369583883258));
#21346=DIRECTION('ref_axis',(-0.00326400780572816,-0.883333427384614,0.468733828860255));
#21347=DIRECTION('center_axis',(0.999992536601163,-0.0038579454128945,-0.000207362394964344));
#21348=DIRECTION('ref_axis',(0.00385794549583871,0.999992558100585,0.));
#21349=DIRECTION('center_axis',(0.999990310770151,-0.00440207545088307,
-9.87630342248303E-6));
#21350=DIRECTION('ref_axis',(-5.67743328359544E-5,-0.0106536201675253,-0.999943246966547));
#21351=DIRECTION('center_axis',(0.999993789133264,-0.00350648377631366,
-0.000355339871731304));
#21352=DIRECTION('ref_axis',(-0.000355337663693595,1.25270705322677E-6,
-0.999999936866786));
#21353=DIRECTION('center_axis',(0.0825919165140834,0.996583451260439,-6.02271343951247E-7));
#21354=DIRECTION('ref_axis',(0.996583451260621,-0.082591916514075,3.89962523269363E-8));
#21355=DIRECTION('center_axis',(-0.0825919163630573,0.996583451272945,-6.20081085572316E-7));
#21356=DIRECTION('ref_axis',(0.996583451273137,0.0825919163630472,-4.26522010047437E-8));
#21357=DIRECTION('center_axis',(1.,0.,0.));
#21358=DIRECTION('ref_axis',(0.,-1.,0.));
#21359=DIRECTION('center_axis',(-0.969814393901857,0.243844297412866,-1.75042618129133E-12));
#21360=DIRECTION('ref_axis',(-0.243844297412866,-0.969814393901857,-1.66055871266714E-29));
#21361=DIRECTION('center_axis',(6.93889390390723E-16,0.,1.));
#21362=DIRECTION('ref_axis',(1.,0.,-6.37059463001412E-16));
#21363=DIRECTION('center_axis',(-0.984842147348564,0.173453004603174,6.83371517254786E-16));
#21364=DIRECTION('ref_axis',(-0.173453004603174,-0.984842147348564,7.55355110189228E-33));
#21365=DIRECTION('center_axis',(0.999993711234398,-0.00354647500652752,
-2.58533075644835E-6));
#21366=DIRECTION('ref_axis',(0.00354647500653937,0.99999371123774,-7.29885891232207E-24));
#21367=DIRECTION('center_axis',(-0.999993447039029,0.00361187934263431,
0.000245370360983865));
#21368=DIRECTION('ref_axis',(-0.000245366581733725,1.4894891990769E-6,-0.999999969896511));
#21369=DIRECTION('center_axis',(0.999995302234954,-0.00306520929522128,
-3.17016093720866E-13));
#21370=DIRECTION('ref_axis',(0.00271824782984711,0.88680243276121,0.462140732220754));
#21371=DIRECTION('center_axis',(0.999995302242941,-0.00306520668935977,
1.41267078951194E-12));
#21372=DIRECTION('ref_axis',(2.87570856016762E-8,9.38219006929373E-6,0.999999999955987));
#21373=DIRECTION('center_axis',(0.999993711188974,-0.00354648781441971,
2.58552001539276E-6));
#21374=DIRECTION('ref_axis',(0.00354648781443156,0.999993711192317,-1.16816817935139E-23));
#21375=DIRECTION('center_axis',(-0.999993257216905,0.00366579675322716,
-0.00021784143289343));
#21376=DIRECTION('ref_axis',(0.00319184891825971,0.838306860871718,-0.545189342445255));
#21377=DIRECTION('center_axis',(-0.951640608285474,-0.167605461698958,-0.25746565182706));
#21378=DIRECTION('ref_axis',(-0.261159981199218,7.93998114470773E-18,0.965295532062603));
#21379=DIRECTION('center_axis',(-0.244892111977192,-0.956154896867404,-0.160610294464068));
#21380=DIRECTION('ref_axis',(0.968731061165788,-0.248113141797458,1.27019149305754E-16));
#21381=DIRECTION('center_axis',(-0.244864748752396,0.95616063541462,-0.160617851130988));
#21382=DIRECTION('ref_axis',(-0.968738082088973,-0.24808572774462,-1.42728691652663E-16));
#21383=DIRECTION('center_axis',(-0.951640608283787,0.167605461701957,-0.257465651831341));
#21384=DIRECTION('ref_axis',(-0.261159981203695,8.13263164653001E-17,0.965295532061392));
#21385=DIRECTION('center_axis',(1.,0.,0.));
#21386=DIRECTION('ref_axis',(0.,0.876535239907724,-0.481337691439087));
#21387=DIRECTION('center_axis',(-0.244892182585915,0.956154863195271,0.160610387261659));
#21388=DIRECTION('ref_axis',(-0.968731041871288,-0.248113217130746,-1.42505471275098E-17));
#21389=DIRECTION('center_axis',(-0.951640551025411,0.167605051542164,0.257466130474672));
#21390=DIRECTION('ref_axis',(0.261160448242619,4.15284970329584E-18,0.965295405704241));
#21391=DIRECTION('center_axis',(1.,0.,0.));
#21392=DIRECTION('ref_axis',(0.,0.87657024749419,0.481273935724733));
#21393=DIRECTION('center_axis',(0.984842218075142,-0.173452603026977,-9.02676907320607E-15));
#21394=DIRECTION('ref_axis',(0.173452603026977,0.984842218075142,2.17217989749286E-31));
#21395=DIRECTION('center_axis',(6.93889390390723E-16,0.,-1.));
#21396=DIRECTION('ref_axis',(-1.,0.,-6.37059463001412E-16));
#21397=DIRECTION('center_axis',(0.96981448141323,-0.243843949363496,2.90327682891753E-13));
#21398=DIRECTION('ref_axis',(0.243843949363496,0.96981448141323,4.72120435553235E-31));
#21399=DIRECTION('center_axis',(1.,0.,0.));
#21400=DIRECTION('ref_axis',(0.,-1.,0.));
#21401=DIRECTION('center_axis',(-0.244864821889913,-0.956160598919634,0.16061795688673));
#21402=DIRECTION('ref_axis',(0.968738062004926,-0.248085806169841,3.77743453549349E-19));
#21403=DIRECTION('center_axis',(0.999993662978143,0.00356005563298786,2.72893016458924E-6));
#21404=DIRECTION('ref_axis',(0.00311111586717999,-0.874261870422573,0.485444644509841));
#21405=DIRECTION('center_axis',(0.999995302242957,0.00306520668415282,-1.74781900008877E-12));
#21406=DIRECTION('ref_axis',(0.00271825281217274,-0.886804813943252,-0.462136162909508));
#21407=DIRECTION('center_axis',(0.999995302234954,0.00306520929503774,1.39698738163942E-14));
#21408=DIRECTION('ref_axis',(2.8755664516212E-8,-9.38124145866162E-6,-0.999999999955996));
#21409=DIRECTION('center_axis',(0.999993711234403,0.00354647500511862,-2.58533131823476E-6));
#21410=DIRECTION('ref_axis',(0.0031007485640922,-0.874666312378887,-0.484715614920607));
#21411=DIRECTION('center_axis',(-0.999993447038901,-0.00361187937971174,
0.000245370340625091));
#21412=DIRECTION('ref_axis',(0.00317944976032623,-0.843814728946945,0.536625189784654));
#21413=DIRECTION('center_axis',(1.,0.,0.));
#21414=DIRECTION('ref_axis',(0.,-1.,0.));
#21415=DIRECTION('center_axis',(0.984842147375681,0.173453004449208,-1.64841417546653E-10));
#21416=DIRECTION('ref_axis',(-0.173453004449208,0.984842147375681,-1.94987819100897E-27));
#21417=DIRECTION('center_axis',(6.93889390390723E-16,0.,1.));
#21418=DIRECTION('ref_axis',(1.,0.,-6.37059463001412E-16));
#21419=DIRECTION('center_axis',(0.969814393902275,0.243844297411202,-2.84511405416877E-13));
#21420=DIRECTION('ref_axis',(-0.243844297411202,0.969814393902275,1.27098327284467E-30));
#21421=DIRECTION('center_axis',(1.,0.,0.));
#21422=DIRECTION('ref_axis',(0.,-1.,0.));
#21423=DIRECTION('center_axis',(-0.0823386574739372,0.996604407719049,5.95150216138491E-7));
#21424=DIRECTION('ref_axis',(0.996604407719226,0.0823386574739416,1.7269978458749E-8));
#21425=DIRECTION('center_axis',(0.63736849112035,0.0611262158547342,-0.768130843191607));
#21426=DIRECTION('ref_axis',(-0.00927097489734817,0.997384807118265,0.0716770224975518));
#21427=DIRECTION('center_axis',(0.637368185944156,0.0611271411090484,0.768131022785885));
#21428=DIRECTION('ref_axis',(-0.769570799631323,1.71699639970919E-5,0.638561495910925));
#21429=DIRECTION('center_axis',(0.637368456188137,-0.0611270399883367,0.768130806593913));
#21430=DIRECTION('ref_axis',(-0.00927098015071904,-0.997384730640923,-0.0716780859913101));
#21431=DIRECTION('center_axis',(0.637368220895556,-0.0611263169692591,-0.768131059368262));
#21432=DIRECTION('ref_axis',(-0.769570797403229,-1.717109277194E-5,-0.638561498596111));
#21433=DIRECTION('center_axis',(0.0823386573805061,0.996604407726757,6.13355466221133E-7));
#21434=DIRECTION('ref_axis',(0.996604407726945,-0.082338657380496,-4.12451842793918E-8));
#21435=DIRECTION('center_axis',(-0.975990677738216,-0.0251890228193663,
-0.216350895763117));
#21436=DIRECTION('ref_axis',(-0.216419564343231,-5.31751016061812E-18,0.976300451792114));
#21437=DIRECTION('center_axis',(-0.966447028925014,-0.0723817684077612,
-0.246456933122562));
#21438=DIRECTION('ref_axis',(0.156314970820748,0.595634525008648,-0.787899195655783));
#21439=DIRECTION('center_axis',(0.965411969008708,0.0686536407204188,0.251528144967043));
#21440=DIRECTION('ref_axis',(0.148704659736293,0.64743602524561,-0.747471415765767));
#21441=DIRECTION('center_axis',(0.999764710177655,4.72949843663878E-6,0.0216915711976085));
#21442=DIRECTION('ref_axis',(0.0216915711978511,3.37899635702931E-23,-0.999764710188837));
#21443=DIRECTION('center_axis',(0.99976438521954,4.08870955359827E-6,0.0217065434806438));
#21444=DIRECTION('ref_axis',(0.0217065434808252,-2.19008514488595E-22,-0.999764385227897));
#21445=DIRECTION('center_axis',(0.999764064843307,3.40730474217083E-6,0.0217212945373594));
#21446=DIRECTION('ref_axis',(0.0217212945374855,-7.6410513036406E-23,-0.99976406484911));
#21447=DIRECTION('center_axis',(0.99976374924311,2.90109501624487E-6,0.0217358158564165));
#21448=DIRECTION('ref_axis',(0.021735815856508,-1.05284018011641E-22,-0.999763749247317));
#21449=DIRECTION('center_axis',(0.99976640399297,4.0363566896332E-6,0.0216133623176406));
#21450=DIRECTION('ref_axis',(0.0216133623178167,-1.60742745341573E-22,-0.999766404001114));
#21451=DIRECTION('center_axis',(0.999763129384452,8.25018479049991E-7,0.0217643084596511));
#21452=DIRECTION('ref_axis',(0.0217643084596585,2.45472806930464E-24,-0.999763129384792));
#21453=DIRECTION('center_axis',(0.999769417791993,1.50007309598972E-5,0.0214734958224482));
#21454=DIRECTION('ref_axis',(0.0214734958248642,5.20388214323119E-24,-0.999769417904478));
#21455=DIRECTION('center_axis',(0.999763438172819,2.16269669590136E-6,0.0217501192683182));
#21456=DIRECTION('ref_axis',(0.0217501192683691,-1.26685871371197E-22,-0.999763438175157));
#21457=DIRECTION('center_axis',(0.99976503922338,5.12733989460498E-6,0.0216764000789616));
#21458=DIRECTION('ref_axis',(0.0216764000792465,1.99825578127218E-22,-0.999765039236522));
#21459=DIRECTION('center_axis',(0.999765375453303,5.10299320466825E-6,0.0216608868395403));
#21460=DIRECTION('ref_axis',(0.0216608868398223,1.61235729862652E-22,-0.99976537546632));
#21461=DIRECTION('center_axis',(0.999765713346224,5.51245434595147E-6,0.0216452855589496));
#21462=DIRECTION('ref_axis',(0.0216452855592785,-1.64937072290126E-22,-0.999765713361414));
#21463=DIRECTION('center_axis',(0.999766057463275,4.50676636095009E-6,0.0216293856599718));
#21464=DIRECTION('ref_axis',(0.0216293856601915,-1.13137331017225E-22,-0.999766057473429));
#21465=DIRECTION('center_axis',(0.999769839153505,1.40781112176933E-5,0.0214538695992536));
#21466=DIRECTION('ref_axis',(0.0214538696013796,1.23674150965502E-22,-0.999769839252579));
#21467=DIRECTION('center_axis',(0.999770358169119,3.64750266020402E-5,0.0214296429266803));
#21468=DIRECTION('ref_axis',(0.0214296429409356,4.42227884678903E-22,-0.99977035883418));
#21469=DIRECTION('center_axis',(0.999766032799768,2.3287275843937E-5,0.0216305135749479));
#21470=DIRECTION('ref_axis',(0.021630513580813,-4.12908816846881E-22,-0.999766033070853));
#21471=DIRECTION('center_axis',(0.999763745028459,3.66762269207557E-6,0.0217360095974351));
#21472=DIRECTION('ref_axis',(0.0217360095975813,-5.4425946294211E-23,-0.999763745035183));
#21473=DIRECTION('center_axis',(0.999763972772618,7.80388041093266E-6,0.0217255307187726));
#21474=DIRECTION('ref_axis',(0.0217255307194341,-4.1126736519674E-22,-0.999763972803061));
#21475=DIRECTION('center_axis',(-0.974671768615882,-0.0286863516212842,
0.221792778723403));
#21476=DIRECTION('ref_axis',(0.221884092473798,-2.88678970212481E-17,0.975073048292834));
#21477=DIRECTION('center_axis',(-0.975976237722848,0.0252188885886727,0.216412548293086));
#21478=DIRECTION('ref_axis',(0.216481399498132,-2.06557536366637E-17,0.976286742546128));
#21479=DIRECTION('center_axis',(0.999764709262297,-4.73662963717919E-6,
-0.0216916133848715));
#21480=DIRECTION('ref_axis',(0.0216916112630805,-0.000274958271209076,0.999764671509631));
#21481=DIRECTION('center_axis',(0.999764384264301,-4.08849168619633E-6,
-0.0217065874772601));
#21482=DIRECTION('ref_axis',(0.0217065858809087,-0.000238963614421796,0.999764355748786));
#21483=DIRECTION('center_axis',(0.999764063905754,-3.40534231195707E-6,
-0.0217213376902918));
#21484=DIRECTION('ref_axis',(0.0217213365462412,-0.000203702899778933,0.999764043184077));
#21485=DIRECTION('center_axis',(0.999763748332528,-2.89897229151112E-6,
-0.0217358577399271));
#21486=DIRECTION('ref_axis',(0.0217358569031682,-0.000174525088592317,0.99976373312182));
#21487=DIRECTION('center_axis',(0.999766403501999,-4.31175631876197E-6,
-0.0216133849751954));
#21488=DIRECTION('ref_axis',(0.0216133834966834,-0.000220804919340372,0.999766379160158));
#21489=DIRECTION('center_axis',(0.999763128353256,-8.40752198221754E-7,
-0.0217643558279152));
#21490=DIRECTION('ref_axis',(0.0217643558021162,-2.35325148120707E-5,0.999763128077216));
#21491=DIRECTION('center_axis',(0.999769418060103,-1.50448636207487E-5,
-0.0214734833088371));
#21492=DIRECTION('ref_axis',(0.0214734544646323,-0.00108205437596858,0.999768833236805));
#21493=DIRECTION('center_axis',(0.999763437260841,-2.16801141837553E-6,
-0.0217501611876457));
#21494=DIRECTION('ref_axis',(0.0217501607491883,-0.000124518145035359,0.999763429518512));
#21495=DIRECTION('center_axis',(0.999765038344753,-5.14904944543397E-6,
-0.0216764405980732));
#21496=DIRECTION('ref_axis',(0.0216764381689193,-0.000292188339262183,0.999764995713634));
#21497=DIRECTION('center_axis',(0.999765374632217,-5.15081959904467E-6,
-0.0216609247256913));
#21498=DIRECTION('ref_axis',(0.0216609223653019,-0.000286176218006351,0.999765333738601));
#21499=DIRECTION('center_axis',(0.99976571267043,-5.61582566448302E-6,-0.0216453167463528));
#21500=DIRECTION('ref_axis',(0.0216453140457445,-0.000303503805251101,0.999765666676597));
#21501=DIRECTION('center_axis',(0.999766057204937,-4.76013267136721E-6,
-0.0216293975467653));
#21502=DIRECTION('ref_axis',(0.0216293956773392,-0.00025039306212543,0.999766025901034));
#21503=DIRECTION('center_axis',(0.999769839441945,-1.4088563379705E-5,-0.0214538561508182));
#21504=DIRECTION('ref_axis',(0.0214538329403548,-0.000954360151552805,0.999769384532687));
#21505=DIRECTION('center_axis',(0.999770360412419,9.34322212250805E-6,-0.0214295672734342));
#21506=DIRECTION('ref_axis',(0.0214295545404625,0.000738176847933698,0.999770088213855));
#21507=DIRECTION('center_axis',(0.999766031866939,9.65877267560661E-6,-0.0216305670693989));
#21508=DIRECTION('ref_axis',(0.0216305539828126,0.000740752816224304,0.999765757775121));
#21509=DIRECTION('center_axis',(0.999763744304182,-3.6972435022485E-6,-0.021736042906044));
#21510=DIRECTION('ref_axis',(0.021736041333449,-0.000246635043159153,0.999763713923598));
#21511=DIRECTION('center_axis',(0.999763970269845,-7.60123828743992E-6,
-0.0217256459627287));
#21512=DIRECTION('ref_axis',(0.0217256434705418,-0.000243365665931261,0.999763940732483));
#21513=DIRECTION('center_axis',(-0.861920942122417,0.0166890382046472,-0.506767960248681));
#21514=DIRECTION('ref_axis',(-0.506838548513134,-4.00833851573235E-18,0.862041000034859));
#21515=DIRECTION('center_axis',(-0.871379853789596,0.0464998923150909,0.488400358747111));
#21516=DIRECTION('ref_axis',(0.48892923596368,1.37760753029074E-17,0.872323450458585));
#21517=DIRECTION('center_axis',(0.9997889250661,0.00124823490811798,0.0205072481036904));
#21518=DIRECTION('ref_axis',(0.0205072640797821,-9.63206510880043E-20,-0.999789703947766));
#21519=DIRECTION('center_axis',(0.999793850535689,-0.000926913239675538,
0.0202829303323548));
#21520=DIRECTION('ref_axis',(0.0202829390455843,-1.54023260780225E-20,-0.999794280031484));
#21521=DIRECTION('center_axis',(-0.888474164973873,-0.110685117325802,-0.44537901048046));
#21522=DIRECTION('ref_axis',(0.458638632717905,-0.248526491485849,-0.8531618765559));
#21523=DIRECTION('center_axis',(0.999791013008113,0.00102608806371862,0.0204175770231834));
#21524=DIRECTION('ref_axis',(0.0204175877715834,1.36199942924005E-20,-0.999791539326869));
#21525=DIRECTION('center_axis',(0.999794530784448,-0.000804757388187486,
0.0202545940233657));
#21526=DIRECTION('ref_axis',(0.0202546005821554,-4.98364828404734E-20,-0.999794854535298));
#21527=DIRECTION('center_axis',(0.999791115031614,0.000948396434230425,
0.020416337772641));
#21528=DIRECTION('ref_axis',(0.0204163469544439,-1.5274753026493E-20,-0.999791564665874));
#21529=DIRECTION('center_axis',(0.999793613160936,-0.000803410291055622,
0.0202998919825738));
#21530=DIRECTION('ref_axis',(0.0202998985340433,-3.79381199126813E-21,-0.999793935828532));
#21531=DIRECTION('center_axis',(0.999787734476799,0.00112360919993097,0.0205723963630029));
#21532=DIRECTION('ref_axis',(0.0205724093493161,-5.07154029360286E-20,-0.999788365592221));
#21533=DIRECTION('center_axis',(0.999793368904827,-0.00075256783557933,
0.020313865599363));
#21534=DIRECTION('ref_axis',(0.0203138713518291,-8.43310052312757E-21,-0.999793652025607));
#21535=DIRECTION('center_axis',(0.999796830831292,0.00103544519085822,0.0201301990293868));
#21536=DIRECTION('ref_axis',(0.0201302098206591,-8.26905179960667E-20,-0.99979736679618));
#21537=DIRECTION('center_axis',(0.999798400909155,-0.000959085530652312,
0.0200558643404188));
#21538=DIRECTION('ref_axis',(0.020055873564569,-8.57107583407826E-20,-0.99979886073928));
#21539=DIRECTION('center_axis',(0.999791828846322,0.000690509182037432,
0.0203917181521609));
#21540=DIRECTION('ref_axis',(0.0203917230135781,1.36073098268412E-20,-0.999792067198244));
#21541=DIRECTION('center_axis',(0.999798557733554,-0.000222129791565017,
0.0200697437019374));
#21542=DIRECTION('ref_axis',(0.0200697441970745,8.00806346724806E-22,-0.999798582399407));
#21543=DIRECTION('center_axis',(0.999807998093897,0.00102627949949861,0.0195681807499801));
#21544=DIRECTION('ref_axis',(0.0195681910550776,1.13196871364439E-20,-0.999808524618005));
#21545=DIRECTION('center_axis',(0.999793956365789,-0.00183064297990715,
0.0202161707730065));
#21546=DIRECTION('ref_axis',(0.0202162046478504,2.20102616963072E-20,-0.999795631651607));
#21547=DIRECTION('center_axis',(0.999782564221964,0.00141848170254525,0.0208041387087796));
#21548=DIRECTION('ref_axis',(0.0208041596387145,-5.80397643032026E-20,-0.999783570049902));
#21549=DIRECTION('center_axis',(0.999794149235583,-0.0006263178055023,0.0202797159818387));
#21550=DIRECTION('ref_axis',(0.0202797199594425,-3.1734126612677E-20,-0.999794345332262));
#21551=DIRECTION('center_axis',(0.999791678956523,0.0011207187498946,0.0203799577718084));
#21552=DIRECTION('ref_axis',(0.0203799705705411,-1.6022026816592E-21,-0.999792306831546));
#21553=DIRECTION('center_axis',(0.999794376483078,-0.000960029259732881,
0.0202554460981016));
#21554=DIRECTION('ref_axis',(0.0202554554323866,1.86296831220422E-20,-0.999794837216729));
#21555=DIRECTION('center_axis',(0.99979286009161,0.00110736634622207,0.0203226634478307));
#21556=DIRECTION('ref_axis',(0.0203226759082791,-1.33088630109754E-19,-0.999793473095282));
#21557=DIRECTION('center_axis',(0.999791633273466,-0.00123760086048944,
0.0203754357127787));
#21558=DIRECTION('ref_axis',(0.0203754513168747,2.79319123752651E-20,-0.999792398942717));
#21559=DIRECTION('center_axis',(0.999793659198503,0.00112258096642959,0.0202824761417586));
#21560=DIRECTION('ref_axis',(0.0202824889216375,8.64084697903419E-20,-0.999794289163098));
#21561=DIRECTION('center_axis',(0.999795640224913,-0.00101430853326898,
0.0201903186070843));
#21562=DIRECTION('ref_axis',(0.0201903289932123,-8.52295535382801E-20,-0.999796154531085));
#21563=DIRECTION('center_axis',(0.999797937496759,0.00087548785669098,0.0200827711793035));
#21564=DIRECTION('ref_axis',(0.020082778875819,-2.87508323961054E-20,-0.999798320659034));
#21565=DIRECTION('center_axis',(0.999788371198081,-0.00162444407414253,
0.0205079008808463));
#21566=DIRECTION('ref_axis',(0.0205079279392145,3.37598965323948E-21,-0.999789690330741));
#21567=DIRECTION('center_axis',(0.999809454916367,0.00101543101890164,0.0194941724544518));
#21568=DIRECTION('ref_axis',(0.0194941825046817,8.09901741121448E-20,-0.999809970368607));
#21569=DIRECTION('center_axis',(0.999813094544414,-0.000821842795898232,
0.0193158109314898));
#21570=DIRECTION('ref_axis',(0.0193158174546895,7.39417849148241E-20,-0.999813432194256));
#21571=DIRECTION('center_axis',(-0.894413399787221,-0.108947147830865,-0.433768589527394));
#21572=DIRECTION('ref_axis',(0.446107570363565,-0.286335917882665,-0.847938546001188));
#21573=DIRECTION('center_axis',(0.999275730732793,-0.0377336078180166,-0.00491821202049895));
#21574=DIRECTION('ref_axis',(0.0377340641918212,0.999287816597184,1.18406610643697E-20));
#21575=DIRECTION('center_axis',(0.9993238879154,0.0365809086693469,-0.00368838210782324));
#21576=DIRECTION('ref_axis',(-0.0365811574982001,0.999330685467074,5.68996066554659E-19));
#21577=DIRECTION('center_axis',(-0.9071068036828,-0.0997526098957014,-0.408909114023362));
#21578=DIRECTION('ref_axis',(0.420735592379569,-0.187704192648809,-0.887552081495544));
#21579=DIRECTION('center_axis',(-0.892779367153904,0.107912754414502,-0.437378370543114));
#21580=DIRECTION('ref_axis',(0.450437289746274,0.229260614961514,-0.862870684652979));
#21581=DIRECTION('center_axis',(-0.906179467397534,0.100126013659033,-0.410869266623671));
#21582=DIRECTION('ref_axis',(0.422740553915488,0.188359688277069,-0.88645984224182));
#21583=DIRECTION('center_axis',(-0.888442770560192,0.11072537147098,0.445431628369544));
#21584=DIRECTION('ref_axis',(0.458700410018584,0.248506250715052,0.853134559846412));
#21585=DIRECTION('center_axis',(0.999788900090079,-0.00125025659902504,
-0.0205083425733733));
#21586=DIRECTION('ref_axis',(0.0202248090182454,0.2357985529214,0.971591477700556));
#21587=DIRECTION('center_axis',(0.999793881909161,0.000924798772571727,
-0.020281480326686));
#21588=DIRECTION('ref_axis',(0.0199249195804614,-0.236470906870714,0.971434252939155));
#21589=DIRECTION('center_axis',(0.999791009341069,-0.00102657885440262,
-0.0204177319167002));
#21590=DIRECTION('ref_axis',(0.0200915076707316,0.233881095299282,0.972057593242872));
#21591=DIRECTION('center_axis',(0.999794553926456,0.000803250983560136,
-0.0202535114697604));
#21592=DIRECTION('ref_axis',(0.0198773395977057,-0.234440014181946,0.971927348684502));
#21593=DIRECTION('center_axis',(0.999791136401335,-0.000947056551401116,
-0.020415353467797));
#21594=DIRECTION('ref_axis',(0.0200780696682136,0.231986423030301,0.972511784323462));
#21595=DIRECTION('center_axis',(0.999793638354371,0.000801760735019295,
-0.0202987163597241));
#21596=DIRECTION('ref_axis',(0.0199289344184095,-0.232475550901422,0.972398043913102));
#21597=DIRECTION('center_axis',(0.999787777679922,-0.00112074158813577,
-0.0205704530853312));
#21598=DIRECTION('ref_axis',(0.0202762490552125,0.230120557335461,0.972950873793671));
#21599=DIRECTION('center_axis',(0.999793364511817,0.000753129469705107,
-0.0203140609958707));
#21600=DIRECTION('ref_axis',(0.019940463145563,-0.230537759819647,0.972859043863436));
#21601=DIRECTION('center_axis',(0.999797269820169,-0.00100281307594856,
-0.0201100379430304));
#21602=DIRECTION('ref_axis',(0.0197388213428965,0.245971495490712,0.969076056013178));
#21603=DIRECTION('center_axis',(0.999798569975224,0.000946215735264768,
-0.0200480460713516));
#21604=DIRECTION('ref_axis',(0.0196627093866498,-0.246479167651138,0.968948604299309));
#21605=DIRECTION('center_axis',(0.999791885662076,-0.000686562352684949,
-0.0203890656089599));
#21606=DIRECTION('ref_axis',(0.0200146371369503,0.226504667176284,0.973804420840056));
#21607=DIRECTION('center_axis',(0.99979855577085,0.000222511329138727,-0.0200698372497246));
#21608=DIRECTION('ref_axis',(0.0195979526674169,-0.226653390542104,0.973778291402624));
#21609=DIRECTION('center_axis',(0.999808251227011,-0.0010122534972086,-0.0195559740551144));
#21610=DIRECTION('ref_axis',(0.019561740686774,0.097217177687249,0.995070931473646));
#21611=DIRECTION('center_axis',(0.999793794637041,0.00183980383449,-0.0202233362014672));
#21612=DIRECTION('ref_axis',(0.0203061294301529,-0.0989747175626273,0.994882740020634));
#21613=DIRECTION('center_axis',(0.999782618994953,-0.0014149149279061,-0.0208017492374791));
#21614=DIRECTION('ref_axis',(0.0205754110187433,0.228287297878377,0.973376372267582));
#21615=DIRECTION('center_axis',(0.999794150030209,0.00062648588613381,-0.0202796716148505));
#21616=DIRECTION('ref_axis',(0.0198859134073932,-0.228587973036081,0.973320136969954));
#21617=DIRECTION('center_axis',(0.999791628136578,-0.0011246887331621,-0.0203822320481515));
#21618=DIRECTION('ref_axis',(0.0200651399814408,0.237752804753668,0.971118424286806));
#21619=DIRECTION('center_axis',(0.999794411622241,0.000957621136659537,
-0.0202538255817547));
#21620=DIRECTION('ref_axis',(0.0198979725293028,-0.238433414014752,0.970954982360404));
#21621=DIRECTION('center_axis',(0.999792754982158,-0.00111540024855146,
-0.0203273945077252));
#21622=DIRECTION('ref_axis',(0.0200019923075789,0.239729634175733,0.970633619241419));
#21623=DIRECTION('center_axis',(0.999791681155371,0.00123430342639552,-0.0203732861259386));
#21624=DIRECTION('ref_axis',(0.0200723578644585,-0.240436401635085,0.970457334053658));
#21625=DIRECTION('center_axis',(0.999793307262561,-0.00114897474535068,
-0.0202983400805286));
#21626=DIRECTION('ref_axis',(0.0199739827107701,0.241749830888139,0.970133011127972));
#21627=DIRECTION('center_axis',(0.999795700732705,0.00100994630042123,-0.0201875408326533));
#21628=DIRECTION('ref_axis',(0.0198300396982846,-0.242451180930935,0.969960924156617));
#21629=DIRECTION('center_axis',(0.999796612386705,-0.00097684807480299,
-0.0201439724956925));
#21630=DIRECTION('ref_axis',(0.0197741222240788,0.243832457525914,0.969615757270446));
#21631=DIRECTION('center_axis',(0.999788470786211,0.00161750735550819,-0.0205035936588081));
#21632=DIRECTION('ref_axis',(0.020276847625652,-0.24446333162905,0.969446506486661));
#21633=DIRECTION('center_axis',(0.999809561437771,-0.00100976586465744,
-0.0194890028095292));
#21634=DIRECTION('ref_axis',(0.0194928865433859,0.0993568624144647,0.994860915538127));
#21635=DIRECTION('center_axis',(0.999813090956489,0.000822563171989843,
-0.0193159659830663));
#21636=DIRECTION('ref_axis',(0.019299902172773,-0.101315362126067,0.994667135866761));
#21637=DIRECTION('center_axis',(-0.894513307027751,0.108908998607699,0.433572108849894));
#21638=DIRECTION('ref_axis',(0.445950796796345,0.285094269409663,0.848439240244389));
#21639=DIRECTION('center_axis',(0.999275539368059,0.0377381791903952,0.00492201707314082));
#21640=DIRECTION('ref_axis',(-0.0377386363260221,0.999287643938547,1.44659142945742E-19));
#21641=DIRECTION('center_axis',(0.999323945968658,-0.0365793722937842,0.00368789048421688));
#21642=DIRECTION('ref_axis',(0.0365796210458605,0.99933074170874,5.48310762901686E-20));
#21643=DIRECTION('center_axis',(-0.899913319397339,0.103764596224201,0.423543299016396));
#21644=DIRECTION('ref_axis',(0.435882629579717,0.185666942346874,0.880644150466142));
#21645=DIRECTION('center_axis',(-0.892850412212971,-0.107873925346478,0.437242904621071));
#21646=DIRECTION('ref_axis',(0.450296527273034,-0.22926177676768,0.862943842459735));
#21647=DIRECTION('center_axis',(-0.902455495465162,-0.102686894907543,0.418365247503871));
#21648=DIRECTION('ref_axis',(0.430605675709258,-0.18716164862259,0.882920873766074));
#21649=DIRECTION('center_axis',(-0.0158981576952788,0.585858710763356,0.81025725520022));
#21650=DIRECTION('ref_axis',(-0.128366775809462,-0.804849591107076,0.579429984176739));
#21651=DIRECTION('center_axis',(0.964785017122322,-0.0707010746474826,0.253359879973077));
#21652=DIRECTION('ref_axis',(0.253995491527146,0.,-0.967205402323562));
#21653=DIRECTION('center_axis',(-0.4517890859873,0.439366663897523,0.776430007430368));
#21654=DIRECTION('ref_axis',(0.864325114912213,0.,0.502933490366261));
#21655=DIRECTION('center_axis',(0.99979575798624,-0.00165747969236773,0.0201418736414786));
#21656=DIRECTION('ref_axis',(0.0201419013088053,-6.91947263585986E-21,-0.999797131327984));
#21657=DIRECTION('center_axis',(0.957670107909995,-0.0378387209059063,0.285370278087721));
#21658=DIRECTION('ref_axis',(0.285574789854396,0.,-0.958356426075193));
#21659=DIRECTION('center_axis',(-0.0157867627303391,0.591490281443045,0.806157568395238));
#21660=DIRECTION('ref_axis',(0.,-0.806258043227403,0.591564001382031));
#21661=DIRECTION('center_axis',(-0.574815246048694,-0.372435393183957,0.72861465179743));
#21662=DIRECTION('ref_axis',(0.785095927168427,0.,0.619374188309093));
#21663=DIRECTION('center_axis',(-0.0158858783442597,-0.585584495916129,
0.81045569713087));
#21664=DIRECTION('ref_axis',(-0.103891727389854,0.807137326320615,0.581150449918059));
#21665=DIRECTION('center_axis',(0.965326993626903,0.0677101640932514,0.252109359313991));
#21666=DIRECTION('ref_axis',(0.252689272754282,0.,-0.967547482780516));
#21667=DIRECTION('center_axis',(0.999814819167062,0.000554045269651598,
0.0192359145292012));
#21668=DIRECTION('ref_axis',(0.0192359174815893,-7.65610025019835E-21,-0.999814972621755));
#21669=DIRECTION('center_axis',(0.966303505500391,0.0721331810984261,0.24709176320201));
#21670=DIRECTION('ref_axis',(0.247737116134259,0.,-0.968827291775722));
#21671=DIRECTION('center_axis',(0.0157842736068064,-0.591588197507761,0.806085765459373));
#21672=DIRECTION('ref_axis',(0.,-0.806186199657785,-0.591661906397004));
#21673=DIRECTION('center_axis',(-0.0157863871158359,-0.591180316731151,
0.806384910009783));
#21674=DIRECTION('ref_axis',(0.0315820058328888,0.80578818841723,0.591361118365801));
#21675=DIRECTION('center_axis',(0.966378069659036,-0.0724684750264558,-0.246701736129714));
#21676=DIRECTION('ref_axis',(-0.247352098144654,0.,-0.968925662547668));
#21677=DIRECTION('center_axis',(0.999814852905107,-0.000552632782769883,
-0.01923420150011));
#21678=DIRECTION('ref_axis',(0.0192033195060585,0.092118786496819,0.995562836637799));
#21679=DIRECTION('center_axis',(0.965531741233883,-0.0685504202901476,-0.251096189831526));
#21680=DIRECTION('ref_axis',(-0.251688247883278,0.,-0.967808362165489));
#21681=DIRECTION('center_axis',(0.0158782835274792,-0.586533726279538,0.809769144910363));
#21682=DIRECTION('ref_axis',(-0.123819524012861,-0.804790948205936,-0.5805000044436));
#21683=DIRECTION('center_axis',(0.438823103950365,-0.445656359684007,0.780272191297733));
#21684=DIRECTION('ref_axis',(0.,-0.868345456619373,-0.495959845117014));
#21685=DIRECTION('center_axis',(0.0157906183176418,0.591381310212439,0.806237435439812));
#21686=DIRECTION('ref_axis',(0.0301303812059224,0.805690346002935,-0.591570136573895));
#21687=DIRECTION('center_axis',(0.965712986386173,0.0749508725835839,-0.248557427215642));
#21688=DIRECTION('ref_axis',(-0.249258534766396,0.,-0.968436979284718));
#21689=DIRECTION('center_axis',(0.999796052573138,0.00164189776482789,-0.0201285228196576));
#21690=DIRECTION('ref_axis',(0.020193557109576,-0.0946575785765395,0.995305060305276));
#21691=DIRECTION('center_axis',(0.526294582686482,0.401383271747728,0.749603549481958));
#21692=DIRECTION('ref_axis',(0.818424732890698,0.,-0.57461374556548));
#21693=DIRECTION('center_axis',(0.964696696273675,0.0703284210564187,-0.253799522045191));
#21694=DIRECTION('ref_axis',(-0.254429517253042,0.,-0.967091319757542));
#21695=DIRECTION('center_axis',(0.0158966842261725,0.585482599575022,0.810529099431654));
#21696=DIRECTION('ref_axis',(-0.114192359427942,0.806390651605264,-0.580253584264602));
#21697=DIRECTION('axis',(0.,0.,1.));
#21698=DIRECTION('refdir',(1.,0.,0.));
#21699=DIRECTION('center_axis',(0.999262230046436,0.0296611786871826,-0.0243969277063748));
#21700=DIRECTION('ref_axis',(-0.00376824454709722,-0.556456744658462,-0.830868035043556));
#21701=DIRECTION('center_axis',(0.999262200442761,-0.0296605976385099,-0.0243988465714553));
#21702=DIRECTION('ref_axis',(0.00376825013598259,0.707931452975492,-0.706271093970949));
#21703=DIRECTION('center_axis',(-1.33376816360845E-16,1.,0.));
#21704=DIRECTION('ref_axis',(-1.,-1.33376816360845E-16,0.));
#21705=DIRECTION('center_axis',(-1.33376816360845E-16,1.,0.));
#21706=DIRECTION('ref_axis',(-1.,-1.33376816360845E-16,0.));
#21707=DIRECTION('center_axis',(-1.33376816360845E-16,1.,0.));
#21708=DIRECTION('ref_axis',(-1.,-1.33376816360845E-16,0.));
#21709=DIRECTION('center_axis',(-1.33376816360845E-16,1.,0.));
#21710=DIRECTION('ref_axis',(-1.,-1.33376816360845E-16,0.));
#21711=DIRECTION('center_axis',(-1.33376816360845E-16,1.,0.));
#21712=DIRECTION('ref_axis',(-1.,-1.33376816360845E-16,0.));
#21713=DIRECTION('center_axis',(-1.33376816360845E-16,1.,0.));
#21714=DIRECTION('ref_axis',(-1.,-1.33376816360845E-16,0.));
#21715=DIRECTION('center_axis',(-1.33376816360845E-16,1.,0.));
#21716=DIRECTION('ref_axis',(-1.,-1.33376816360845E-16,0.));
#21717=DIRECTION('center_axis',(-1.33376816360845E-16,1.,0.));
#21718=DIRECTION('ref_axis',(-1.,-1.33376816360845E-16,0.));
#21719=DIRECTION('center_axis',(-1.33376816360845E-16,1.,0.));
#21720=DIRECTION('ref_axis',(-1.,-1.33376816360845E-16,0.));
#21721=DIRECTION('center_axis',(-1.33376816360845E-16,1.,0.));
#21722=DIRECTION('ref_axis',(-1.,-1.33376816360845E-16,0.));
#21723=DIRECTION('center_axis',(-1.33376816360845E-16,1.,0.));
#21724=DIRECTION('ref_axis',(-1.,-1.33376816360845E-16,0.));
#21725=DIRECTION('center_axis',(-1.33376816360845E-16,1.,0.));
#21726=DIRECTION('ref_axis',(-1.,-1.33376816360845E-16,0.));
#21727=DIRECTION('',(1.33376816360845E-16,-1.,0.));
#21728=DIRECTION('center_axis',(-1.33376816360845E-16,1.,0.));
#21729=DIRECTION('ref_axis',(-1.,-1.33376816360845E-16,0.));
#21730=DIRECTION('center_axis',(-1.33376816360845E-16,1.,0.));
#21731=DIRECTION('ref_axis',(-1.,-1.33376816360845E-16,0.));
#21732=DIRECTION('center_axis',(1.15648231731787E-16,-1.,0.));
#21733=DIRECTION('ref_axis',(1.,1.15648231731787E-16,0.));
#21734=DIRECTION('center_axis',(1.15648231731787E-16,-1.,0.));
#21735=DIRECTION('ref_axis',(1.,1.15648231731787E-16,0.));
#21736=DIRECTION('center_axis',(1.15648231731787E-16,-1.,0.));
#21737=DIRECTION('ref_axis',(1.,1.15648231731787E-16,0.));
#21738=DIRECTION('center_axis',(1.15648231731787E-16,-1.,0.));
#21739=DIRECTION('ref_axis',(1.,1.15648231731787E-16,0.));
#21740=DIRECTION('center_axis',(1.15648231731787E-16,-1.,0.));
#21741=DIRECTION('ref_axis',(1.,1.15648231731787E-16,0.));
#21742=DIRECTION('center_axis',(1.15648231731787E-16,-1.,0.));
#21743=DIRECTION('ref_axis',(1.,1.15648231731787E-16,0.));
#21744=DIRECTION('center_axis',(1.15648231731787E-16,-1.,0.));
#21745=DIRECTION('ref_axis',(1.,1.15648231731787E-16,0.));
#21746=DIRECTION('center_axis',(1.15648231731787E-16,-1.,0.));
#21747=DIRECTION('ref_axis',(1.,1.15648231731787E-16,0.));
#21748=DIRECTION('center_axis',(1.15648231731787E-16,-1.,0.));
#21749=DIRECTION('ref_axis',(1.,1.15648231731787E-16,0.));
#21750=DIRECTION('center_axis',(1.15648231731787E-16,-1.,0.));
#21751=DIRECTION('ref_axis',(1.,1.15648231731787E-16,0.));
#21752=DIRECTION('center_axis',(-9.13012355777267E-17,1.,0.));
#21753=DIRECTION('ref_axis',(-1.,-9.13012355777267E-17,0.));
#21754=DIRECTION('',(-9.13012355777267E-17,1.,0.));
#21755=DIRECTION('',(-9.13012355777267E-17,1.,0.));
#21756=DIRECTION('center_axis',(-1.33376816360844E-16,1.,4.20755807831181E-17));
#21757=DIRECTION('ref_axis',(1.,1.33376816360845E-16,-1.2312033195887E-14));
#21758=DIRECTION('',(-1.33376816360844E-16,1.,4.20755807831181E-17));
#21759=DIRECTION('',(-1.33376816360844E-16,1.,4.20755807831181E-17));
#21760=DIRECTION('center_axis',(-1.33376816360845E-16,1.,-4.20755807831181E-17));
#21761=DIRECTION('ref_axis',(-1.,-1.33376816360845E-16,0.));
#21762=DIRECTION('',(-1.33376816360845E-16,1.,-4.20755807831181E-17));
#21763=DIRECTION('',(-1.33376816360845E-16,1.,-4.20755807831181E-17));
#21764=DIRECTION('center_axis',(-1.75452397143963E-16,1.,0.));
#21765=DIRECTION('ref_axis',(-1.,-1.75452397143963E-16,0.));
#21766=DIRECTION('',(-1.75452397143963E-16,1.,0.));
#21767=DIRECTION('',(-1.75452397143963E-16,1.,0.));
#21768=DIRECTION('center_axis',(-1.75452397143963E-16,1.,0.));
#21769=DIRECTION('ref_axis',(-1.,-1.75452397143963E-16,0.));
#21770=DIRECTION('center_axis',(-1.33376816360845E-16,1.,-4.20755807831181E-17));
#21771=DIRECTION('ref_axis',(0.707106781186543,6.45597228077203E-17,-0.707106781186552));
#21772=DIRECTION('center_axis',(-9.13012355777267E-17,1.,0.));
#21773=DIRECTION('ref_axis',(0.707106781186543,6.45597228077206E-17,0.707106781186552));
#21774=DIRECTION('center_axis',(-1.33376816360844E-16,1.,4.20755807831181E-17));
#21775=DIRECTION('ref_axis',(-1.,-1.33376816360844E-16,0.));
#21776=DIRECTION('center_axis',(-1.15648231731787E-16,1.,0.));
#21777=DIRECTION('ref_axis',(-1.,-1.15648231731787E-16,0.));
#21778=DIRECTION('',(1.15648231731787E-16,-1.,0.));
#21779=DIRECTION('center_axis',(1.15648231731787E-16,-1.,0.));
#21780=DIRECTION('ref_axis',(1.,1.15648231731787E-16,0.));
#21781=DIRECTION('center_axis',(1.15648231731787E-16,-1.,0.));
#21782=DIRECTION('ref_axis',(1.,1.15648231731787E-16,0.));
#21783=DIRECTION('center_axis',(1.15648231731787E-16,-1.,0.));
#21784=DIRECTION('ref_axis',(1.,1.15648231731787E-16,0.));
#21785=DIRECTION('center_axis',(1.15648231731787E-16,-1.,0.));
#21786=DIRECTION('ref_axis',(1.,1.15648231731787E-16,0.));
#21787=DIRECTION('center_axis',(1.15648231731787E-16,-1.,0.));
#21788=DIRECTION('ref_axis',(1.,1.15648231731787E-16,0.));
#21789=DIRECTION('center_axis',(1.15648231731787E-16,-1.,0.));
#21790=DIRECTION('ref_axis',(1.,0.,0.));
#21791=DIRECTION('center_axis',(1.22464679914735E-16,1.41628236817384E-32,
-1.));
#21792=DIRECTION('ref_axis',(-1.,0.,-1.22464679914735E-16));
#21793=DIRECTION('center_axis',(1.15648231731787E-16,-1.,0.));
#21794=DIRECTION('ref_axis',(1.,1.15648231731787E-16,0.));
#21795=DIRECTION('center_axis',(1.15648231731787E-16,-1.,0.));
#21796=DIRECTION('ref_axis',(1.,1.15648231731787E-16,0.));
#21797=DIRECTION('',(1.15648231731787E-16,-1.,0.));
#21798=DIRECTION('center_axis',(1.15648231731787E-16,-1.,0.));
#21799=DIRECTION('ref_axis',(1.,1.15648231731787E-16,0.));
#21800=DIRECTION('center_axis',(1.15648231731787E-16,-1.,0.));
#21801=DIRECTION('ref_axis',(1.,1.15648231731787E-16,0.));
#21802=DIRECTION('center_axis',(1.15648231731787E-16,-1.,0.));
#21803=DIRECTION('ref_axis',(1.,1.15648231731787E-16,0.));
#21804=DIRECTION('center_axis',(1.,4.38931774757775E-24,-9.9579925010296E-17));
#21805=DIRECTION('ref_axis',(-9.9579925010296E-17,0.,-1.));
#21806=DIRECTION('',(-1.,-4.38931774757775E-24,9.9579925010296E-17));
#21807=DIRECTION('center_axis',(1.,-2.11863444194148E-23,-9.9579925010296E-17));
#21808=DIRECTION('ref_axis',(-9.9579925010296E-17,0.,-1.));
#21809=DIRECTION('center_axis',(-1.,1.98089019303025E-8,-1.56581200582727E-8));
#21810=DIRECTION('ref_axis',(2.43121132745886E-8,0.587909515445564,-0.80892669732712));
#21811=DIRECTION('',(1.,-2.11863444194148E-23,-9.9579925010296E-17));
#21812=DIRECTION('center_axis',(0.999472141255957,-0.0286348071154382,-0.0153455750851244));
#21813=DIRECTION('ref_axis',(0.00317408767800045,0.556162888203051,-0.831067245746729));
#21814=DIRECTION('center_axis',(-1.,1.98089019303025E-8,-1.56581200582727E-8));
#21815=DIRECTION('ref_axis',(2.43121132745886E-8,0.587909515445564,-0.80892669732712));
#21816=DIRECTION('center_axis',(-1.,0.,0.));
#21817=DIRECTION('ref_axis',(0.,0.,1.));
#21818=DIRECTION('center_axis',(1.,0.,0.));
#21819=DIRECTION('ref_axis',(0.,0.,-1.));
#21820=DIRECTION('center_axis',(1.,0.,0.));
#21821=DIRECTION('ref_axis',(0.,0.,-1.));
#21822=DIRECTION('center_axis',(1.,0.,0.));
#21823=DIRECTION('ref_axis',(0.,0.,-1.));
#21824=DIRECTION('',(1.,0.,0.));
#21825=DIRECTION('center_axis',(0.999999999993368,5.57549682629954E-7,-3.59912391188234E-6));
#21826=DIRECTION('ref_axis',(-3.59912391187535E-6,0.,-0.999999999993523));
#21827=DIRECTION('center_axis',(5.57549682626343E-7,-0.999999999999845,
-2.00669039482449E-12));
#21828=DIRECTION('ref_axis',(3.59912391189779E-6,0.,0.999999999993523));
#21829=DIRECTION('center_axis',(1.15648231731787E-16,-1.,0.));
#21830=DIRECTION('ref_axis',(1.,0.,0.));
#21831=DIRECTION('center_axis',(-1.22464679914735E-16,-1.41628236817384E-32,
1.));
#21832=DIRECTION('ref_axis',(-1.,0.,-1.22464679914735E-16));
#21833=DIRECTION('center_axis',(1.15648231731787E-16,-1.,0.));
#21834=DIRECTION('ref_axis',(1.,0.,0.));
#21835=DIRECTION('center_axis',(1.22464679914735E-16,1.41628236817384E-32,
-1.));
#21836=DIRECTION('ref_axis',(-1.,0.,-1.22464679914735E-16));
#21837=DIRECTION('center_axis',(-1.33376816360845E-16,1.,0.));
#21838=DIRECTION('ref_axis',(-1.,0.,0.));
#21839=DIRECTION('center_axis',(-1.22464679914735E-16,-1.63339491236773E-32,
-1.));
#21840=DIRECTION('ref_axis',(1.,0.,-1.22464679914735E-16));
#21841=DIRECTION('axis',(0.,0.,1.));
#21842=DIRECTION('refdir',(1.,0.,0.));
#21843=DIRECTION('center_axis',(0.,1.,0.));
#21844=DIRECTION('ref_axis',(0.,0.,1.));
#21845=DIRECTION('',(0.626301308135395,0.,0.779581087140967));
#21846=DIRECTION('',(-0.488115619572884,0.,0.872778976562211));
#21847=DIRECTION('',(0.571640760429912,0.,0.82050401645276));
#21848=DIRECTION('',(0.987834679513523,0.,-0.155507703829795));
#21849=DIRECTION('',(0.514314959619115,0.,0.857601377279671));
#21850=DIRECTION('',(-0.6024126729918,0.,0.798184797787376));
#21851=DIRECTION('',(0.454591185049047,0.,0.890700204600686));
#21852=DIRECTION('',(0.999808896940505,0.,-0.0195491585141347));
#21853=DIRECTION('',(0.952234407172013,0.,0.305368030084627));
#21854=DIRECTION('center_axis',(0.,1.,0.));
#21855=DIRECTION('ref_axis',(0.,0.,1.));
#21856=DIRECTION('center_axis',(0.,1.,0.));
#21857=DIRECTION('ref_axis',(0.,0.,1.));
#21858=DIRECTION('center_axis',(0.,1.,0.));
#21859=DIRECTION('ref_axis',(0.,0.,1.));
#21860=DIRECTION('',(-0.901654311614274,0.,-0.432457515077943));
#21861=DIRECTION('',(-0.955061656436705,0.,-0.296407207072259));
#21862=DIRECTION('',(-0.364725895711544,0.,0.931114934364932));
#21863=DIRECTION('',(0.678041750029829,0.,0.735023390931532));
#21864=DIRECTION('',(0.957458971062196,0.,-0.288569434854979));
#21865=DIRECTION('center_axis',(0.,1.,0.));
#21866=DIRECTION('ref_axis',(0.,0.,1.));
#21867=DIRECTION('center_axis',(0.,-1.,0.));
#21868=DIRECTION('ref_axis',(0.,0.,-1.));
#21869=DIRECTION('',(0.952234407172013,0.,0.305368030084627));
#21870=DIRECTION('',(0.999808896940505,0.,-0.0195491585141347));
#21871=DIRECTION('',(0.454591185049047,0.,0.890700204600686));
#21872=DIRECTION('',(-0.6024126729918,0.,0.798184797787376));
#21873=DIRECTION('',(0.514314959619115,0.,0.857601377279671));
#21874=DIRECTION('',(0.987834679513523,0.,-0.155507703829795));
#21875=DIRECTION('',(0.571640760429912,0.,0.82050401645276));
#21876=DIRECTION('',(-0.488115619572884,0.,0.872778976562211));
#21877=DIRECTION('',(0.626301308135395,0.,0.779581087140967));
#21878=DIRECTION('',(0.957458971062196,0.,-0.288569434854979));
#21879=DIRECTION('',(0.678041750029829,0.,0.735023390931532));
#21880=DIRECTION('',(-0.364725895711544,0.,0.931114934364932));
#21881=DIRECTION('',(-0.955061656436705,0.,-0.296407207072259));
#21882=DIRECTION('',(-0.901654311614274,0.,-0.432457515077943));
#21883=DIRECTION('center_axis',(0.,-1.,0.));
#21884=DIRECTION('ref_axis',(0.,0.,-1.));
#21885=DIRECTION('center_axis',(0.,-1.,0.));
#21886=DIRECTION('ref_axis',(0.,0.,-1.));
#21887=DIRECTION('center_axis',(0.,-1.,0.));
#21888=DIRECTION('ref_axis',(0.,0.,-1.));
#21889=DIRECTION('center_axis',(0.,-1.,0.));
#21890=DIRECTION('ref_axis',(0.,0.,-1.));
#21891=DIRECTION('center_axis',(-0.155507703829795,0.,-0.987834679513523));
#21892=DIRECTION('ref_axis',(-0.987834679513523,0.,0.155507703829795));
#21893=DIRECTION('',(0.,-1.,0.));
#21894=DIRECTION('',(0.987834679513523,0.,-0.155507703829795));
#21895=DIRECTION('',(0.,-1.,0.));
#21896=DIRECTION('',(0.987834679513523,0.,-0.155507703829795));
#21897=DIRECTION('center_axis',(0.82050401645276,0.,-0.571640760429912));
#21898=DIRECTION('ref_axis',(-0.571640760429912,0.,-0.82050401645276));
#21899=DIRECTION('',(0.,-1.,0.));
#21900=DIRECTION('',(0.571640760429912,0.,0.82050401645276));
#21901=DIRECTION('',(0.571640760429912,0.,0.82050401645276));
#21902=DIRECTION('center_axis',(0.872778976562211,0.,0.488115619572884));
#21903=DIRECTION('ref_axis',(0.488115619572884,0.,-0.872778976562211));
#21904=DIRECTION('',(0.,-1.,0.));
#21905=DIRECTION('',(-0.488115619572884,0.,0.872778976562211));
#21906=DIRECTION('',(-0.488115619572884,0.,0.872778976562211));
#21907=DIRECTION('center_axis',(0.779581087140967,0.,-0.626301308135395));
#21908=DIRECTION('ref_axis',(-0.626301308135395,0.,-0.779581087140967));
#21909=DIRECTION('',(0.,-1.,0.));
#21910=DIRECTION('',(0.626301308135395,0.,0.779581087140967));
#21911=DIRECTION('',(0.626301308135395,0.,0.779581087140967));
#21912=DIRECTION('center_axis',(-0.288569434854979,0.,-0.957458971062195));
#21913=DIRECTION('ref_axis',(-0.957458971062195,0.,0.288569434854979));
#21914=DIRECTION('',(0.,-1.,0.));
#21915=DIRECTION('',(0.957458971062196,0.,-0.288569434854979));
#21916=DIRECTION('',(0.957458971062196,0.,-0.288569434854979));
#21917=DIRECTION('center_axis',(0.735023390931532,0.,-0.678041750029829));
#21918=DIRECTION('ref_axis',(-0.678041750029829,0.,-0.735023390931532));
#21919=DIRECTION('',(0.,-1.,0.));
#21920=DIRECTION('',(0.678041750029829,0.,0.735023390931532));
#21921=DIRECTION('',(0.678041750029829,0.,0.735023390931532));
#21922=DIRECTION('center_axis',(0.931114934364932,0.,0.364725895711544));
#21923=DIRECTION('ref_axis',(0.364725895711544,0.,-0.931114934364932));
#21924=DIRECTION('',(0.,-1.,0.));
#21925=DIRECTION('',(-0.364725895711544,0.,0.931114934364932));
#21926=DIRECTION('',(-0.364725895711544,0.,0.931114934364932));
#21927=DIRECTION('center_axis',(-0.296407207072259,0.,0.955061656436705));
#21928=DIRECTION('ref_axis',(0.955061656436705,0.,0.296407207072259));
#21929=DIRECTION('',(0.,-1.,0.));
#21930=DIRECTION('',(-0.955061656436705,0.,-0.296407207072259));
#21931=DIRECTION('',(-0.955061656436705,0.,-0.296407207072259));
#21932=DIRECTION('center_axis',(-0.432457515077943,0.,0.901654311614274));
#21933=DIRECTION('ref_axis',(0.901654311614274,0.,0.432457515077943));
#21934=DIRECTION('',(0.,1.,0.));
#21935=DIRECTION('',(-0.901654311614274,0.,-0.432457515077943));
#21936=DIRECTION('',(-0.901654311614274,0.,-0.432457515077943));
#21937=DIRECTION('center_axis',(0.,-1.,0.));
#21938=DIRECTION('ref_axis',(-0.96822474174621,0.,0.250081685595898));
#21939=DIRECTION('',(0.,-1.,0.));
#21940=DIRECTION('center_axis',(0.,-1.,0.));
#21941=DIRECTION('ref_axis',(0.,0.,-1.));
#21942=DIRECTION('',(0.,-1.,0.));
#21943=DIRECTION('center_axis',(0.,1.,0.));
#21944=DIRECTION('ref_axis',(0.,0.,1.));
#21945=DIRECTION('center_axis',(0.305368030084627,0.,-0.952234407172013));
#21946=DIRECTION('ref_axis',(-0.952234407172013,0.,-0.305368030084627));
#21947=DIRECTION('',(0.,-1.,0.));
#21948=DIRECTION('',(0.952234407172013,0.,0.305368030084627));
#21949=DIRECTION('',(0.,1.,0.));
#21950=DIRECTION('',(0.952234407172013,0.,0.305368030084627));
#21951=DIRECTION('center_axis',(-0.0195491585141347,0.,-0.999808896940505));
#21952=DIRECTION('ref_axis',(-0.999808896940505,0.,0.0195491585141347));
#21953=DIRECTION('',(0.,-1.,0.));
#21954=DIRECTION('',(0.999808896940505,0.,-0.0195491585141347));
#21955=DIRECTION('',(0.999808896940505,0.,-0.0195491585141347));
#21956=DIRECTION('center_axis',(0.890700204600685,0.,-0.454591185049047));
#21957=DIRECTION('ref_axis',(-0.454591185049047,0.,-0.890700204600686));
#21958=DIRECTION('',(0.,-1.,0.));
#21959=DIRECTION('',(0.454591185049047,0.,0.890700204600686));
#21960=DIRECTION('',(0.454591185049047,0.,0.890700204600686));
#21961=DIRECTION('center_axis',(0.798184797787376,0.,0.6024126729918));
#21962=DIRECTION('ref_axis',(0.6024126729918,0.,-0.798184797787376));
#21963=DIRECTION('',(0.,-1.,0.));
#21964=DIRECTION('',(-0.6024126729918,0.,0.798184797787376));
#21965=DIRECTION('',(-0.6024126729918,0.,0.798184797787376));
#21966=DIRECTION('center_axis',(0.857601377279671,0.,-0.514314959619115));
#21967=DIRECTION('ref_axis',(-0.514314959619115,0.,-0.857601377279671));
#21968=DIRECTION('',(0.514314959619115,0.,0.857601377279671));
#21969=DIRECTION('',(0.514314959619115,0.,0.857601377279671));
#21970=DIRECTION('center_axis',(0.,-1.,0.));
#21971=DIRECTION('ref_axis',(0.,0.,-1.));
#21972=DIRECTION('center_axis',(0.,1.,0.));
#21973=DIRECTION('ref_axis',(0.,0.,1.));
#21974=DIRECTION('center_axis',(0.,1.,0.));
#21975=DIRECTION('ref_axis',(0.,0.,1.));
#21976=DIRECTION('',(0.,-1.,0.));
#21977=DIRECTION('center_axis',(0.,-1.,0.));
#21978=DIRECTION('ref_axis',(0.,0.,-1.));
#21979=DIRECTION('center_axis',(-0.488115619572884,0.,0.872778976562211));
#21980=DIRECTION('ref_axis',(0.872778976562211,0.,0.488115619572884));
#21981=DIRECTION('center_axis',(0.0492674350094236,0.,0.998785622567522));
#21982=DIRECTION('ref_axis',(-0.998785622567522,0.,0.0492674350094236));
#21983=DIRECTION('center_axis',(0.0833383631889745,0.,0.996521307961341));
#21984=DIRECTION('ref_axis',(-0.996521307961341,0.,0.0833383631889746));
#21985=DIRECTION('center_axis',(0.626301308135395,0.,0.779581087140967));
#21986=DIRECTION('ref_axis',(0.779581087140968,0.,-0.626301308135395));
#21987=DIRECTION('center_axis',(0.955149485630946,0.,0.29612406200601));
#21988=DIRECTION('ref_axis',(-0.29612406200601,0.,0.955149485630946));
#21989=DIRECTION('center_axis',(0.626301308135395,0.,0.779581087140967));
#21990=DIRECTION('ref_axis',(0.779581087140968,0.,-0.626301308135395));
#21991=DIRECTION('center_axis',(0.955149485630946,0.,0.29612406200601));
#21992=DIRECTION('ref_axis',(0.29612406200601,0.,-0.955149485630946));
#21993=DIRECTION('center_axis',(0.0833383631889745,0.,0.996521307961341));
#21994=DIRECTION('ref_axis',(0.996521307961341,0.,-0.0833383631889746));
#21995=DIRECTION('center_axis',(-0.488115619572884,0.,0.872778976562211));
#21996=DIRECTION('ref_axis',(0.872778976562211,0.,0.488115619572884));
#21997=DIRECTION('center_axis',(0.0492674350094236,0.,0.998785622567522));
#21998=DIRECTION('ref_axis',(0.998785622567522,0.,-0.0492674350094236));
#21999=DIRECTION('center_axis',(0.571640760429912,0.,0.82050401645276));
#22000=DIRECTION('ref_axis',(0.82050401645276,0.,-0.571640760429912));
#22001=DIRECTION('center_axis',(0.919859028046646,0.,0.392249115385974));
#22002=DIRECTION('ref_axis',(-0.392249115385974,0.,0.919859028046646));
#22003=DIRECTION('center_axis',(0.957458971062196,0.,-0.288569434854979));
#22004=DIRECTION('ref_axis',(-0.288569434854979,0.,-0.957458971062195));
#22005=DIRECTION('center_axis',(0.964702659073528,0.,0.263341564468019));
#22006=DIRECTION('ref_axis',(-0.263341564468019,0.,0.964702659073528));
#22007=DIRECTION('center_axis',(0.957458971062196,0.,-0.288569434854979));
#22008=DIRECTION('ref_axis',(-0.288569434854979,0.,-0.957458971062195));
#22009=DIRECTION('center_axis',(0.964702659073528,0.,0.263341564468019));
#22010=DIRECTION('ref_axis',(0.263341564468019,0.,-0.964702659073528));
#22011=DIRECTION('center_axis',(0.571640760429912,0.,0.82050401645276));
#22012=DIRECTION('ref_axis',(0.82050401645276,0.,-0.571640760429912));
#22013=DIRECTION('center_axis',(0.919859028046646,0.,0.392249115385974));
#22014=DIRECTION('ref_axis',(0.392249115385974,0.,-0.919859028046646));
#22015=DIRECTION('center_axis',(0.987834679513523,0.,-0.155507703829795));
#22016=DIRECTION('ref_axis',(-0.155507703829795,0.,-0.987834679513523));
#22017=DIRECTION('center_axis',(0.905930950538282,0.,0.423425451356913));
#22018=DIRECTION('ref_axis',(0.423425451356913,0.,-0.905930950538282));
#22019=DIRECTION('center_axis',(0.678041750029829,0.,0.735023390931532));
#22020=DIRECTION('ref_axis',(0.735023390931532,0.,-0.678041750029829));
#22021=DIRECTION('center_axis',(0.184809846851629,0.,0.982774297845989));
#22022=DIRECTION('ref_axis',(-0.982774297845989,0.,0.184809846851629));
#22023=DIRECTION('center_axis',(0.678041750029829,0.,0.735023390931532));
#22024=DIRECTION('ref_axis',(0.735023390931532,0.,-0.678041750029829));
#22025=DIRECTION('center_axis',(0.184809846851629,0.,0.982774297845989));
#22026=DIRECTION('ref_axis',(0.982774297845989,0.,-0.184809846851629));
#22027=DIRECTION('center_axis',(0.987834679513523,0.,-0.155507703829795));
#22028=DIRECTION('ref_axis',(-0.155507703829795,0.,-0.987834679513523));
#22029=DIRECTION('center_axis',(0.905930950538282,0.,0.423425451356913));
#22030=DIRECTION('ref_axis',(0.423425451356913,0.,-0.905930950538282));
#22031=DIRECTION('center_axis',(0.514314959619115,0.,0.857601377279671));
#22032=DIRECTION('ref_axis',(0.857601377279671,0.,-0.514314959619115));
#22033=DIRECTION('center_axis',(-0.0531308220811139,0.,0.998587560379652));
#22034=DIRECTION('ref_axis',(-0.998587560379652,0.,-0.0531308220811139));
#22035=DIRECTION('center_axis',(-0.364725895711544,0.,0.931114934364932));
#22036=DIRECTION('ref_axis',(0.931114934364932,0.,0.364725895711544));
#22037=DIRECTION('center_axis',(-0.90120055904943,0.,0.433402298527587));
#22038=DIRECTION('ref_axis',(-0.433402298527587,0.,-0.90120055904943));
#22039=DIRECTION('center_axis',(-0.364725895711544,0.,0.931114934364932));
#22040=DIRECTION('ref_axis',(0.931114934364932,0.,0.364725895711544));
#22041=DIRECTION('center_axis',(-0.90120055904943,0.,0.433402298527587));
#22042=DIRECTION('ref_axis',(0.433402298527587,0.,0.90120055904943));
#22043=DIRECTION('center_axis',(0.514314959619115,0.,0.857601377279671));
#22044=DIRECTION('ref_axis',(0.857601377279671,0.,-0.514314959619115));
#22045=DIRECTION('center_axis',(-0.0531308220811139,0.,0.998587560379652));
#22046=DIRECTION('ref_axis',(-0.998587560379652,0.,-0.0531308220811139));
#22047=DIRECTION('center_axis',(-0.6024126729918,0.,0.798184797787376));
#22048=DIRECTION('ref_axis',(0.798184797787376,0.,0.6024126729918));
#22049=DIRECTION('center_axis',(-0.087192735929436,0.,0.996191460915591));
#22050=DIRECTION('ref_axis',(-0.996191460915591,0.,-0.087192735929436));
#22051=DIRECTION('center_axis',(-0.955061656436705,0.,-0.296407207072259));
#22052=DIRECTION('ref_axis',(-0.296407207072259,0.,0.955061656436705));
#22053=DIRECTION('center_axis',(-0.930846909046263,0.,-0.365409403161739));
#22054=DIRECTION('ref_axis',(0.365409403161739,0.,-0.930846909046263));
#22055=DIRECTION('center_axis',(-0.955061656436705,0.,-0.296407207072259));
#22056=DIRECTION('ref_axis',(-0.296407207072259,0.,0.955061656436705));
#22057=DIRECTION('center_axis',(-0.930846909046263,0.,-0.365409403161739));
#22058=DIRECTION('ref_axis',(-0.365409403161739,0.,0.930846909046263));
#22059=DIRECTION('center_axis',(-0.6024126729918,0.,0.798184797787376));
#22060=DIRECTION('ref_axis',(0.798184797787376,0.,0.6024126729918));
#22061=DIRECTION('center_axis',(-0.087192735929436,0.,0.996191460915591));
#22062=DIRECTION('ref_axis',(0.996191460915591,0.,0.087192735929436));
#22063=DIRECTION('center_axis',(0.454591185049047,0.,0.890700204600686));
#22064=DIRECTION('ref_axis',(0.890700204600686,0.,-0.454591185049047));
#22065=DIRECTION('center_axis',(0.857880163767375,0.,0.513849807448113));
#22066=DIRECTION('ref_axis',(-0.513849807448113,0.,0.857880163767375));
#22067=DIRECTION('center_axis',(-0.901654311614274,0.,-0.432457515077943));
#22068=DIRECTION('ref_axis',(-0.432457515077943,0.,0.901654311614274));
#22069=DIRECTION('center_axis',(-0.901654311614274,0.,-0.432457515077943));
#22070=DIRECTION('ref_axis',(-0.432457515077943,0.,0.901654311614274));
#22071=DIRECTION('center_axis',(0.,-1.,0.));
#22072=DIRECTION('ref_axis',(0.,0.,-1.));
#22073=DIRECTION('center_axis',(0.,-1.,0.));
#22074=DIRECTION('ref_axis',(0.,0.,-1.));
#22075=DIRECTION('center_axis',(0.,1.,0.));
#22076=DIRECTION('ref_axis',(0.,0.,1.));
#22077=DIRECTION('center_axis',(-0.901654311614274,0.,-0.432457515077943));
#22078=DIRECTION('ref_axis',(-0.432457515077943,0.,0.901654311614274));
#22079=DIRECTION('center_axis',(-0.901654311614274,0.,-0.432457515077943));
#22080=DIRECTION('ref_axis',(-0.432457515077943,0.,0.901654311614274));
#22081=DIRECTION('center_axis',(0.454591185049047,0.,0.890700204600686));
#22082=DIRECTION('ref_axis',(0.890700204600686,0.,-0.454591185049047));
#22083=DIRECTION('center_axis',(0.857880163767375,0.,0.513849807448113));
#22084=DIRECTION('ref_axis',(0.513849807448113,0.,-0.857880163767375));
#22085=DIRECTION('center_axis',(0.999808896940505,0.,-0.0195491585141347));
#22086=DIRECTION('ref_axis',(-0.0195491585141347,0.,-0.999808896940505));
#22087=DIRECTION('center_axis',(0.989449877530115,0.,0.144875601312438));
#22088=DIRECTION('ref_axis',(-0.144875601312438,0.,0.989449877530115));
#22089=DIRECTION('center_axis',(0.,1.,0.));
#22090=DIRECTION('ref_axis',(-0.302115636055689,0.,-0.95327128481386));
#22091=DIRECTION('center_axis',(0.48796543950748,0.,-0.872862950208262));
#22092=DIRECTION('ref_axis',(-0.872862950208263,0.,-0.48796543950748));
#22093=DIRECTION('center_axis',(0.,-1.,0.));
#22094=DIRECTION('ref_axis',(0.,0.,-1.));
#22095=DIRECTION('center_axis',(0.487965439507477,3.78543962759162E-15,
-0.872862950208264));
#22096=DIRECTION('ref_axis',(-0.872862950208264,-3.40301281036919E-32,-0.487965439507477));
#22097=DIRECTION('center_axis',(0.999808896940505,0.,-0.0195491585141347));
#22098=DIRECTION('ref_axis',(-0.0195491585141347,0.,-0.999808896940505));
#22099=DIRECTION('center_axis',(0.989449877530115,0.,0.144875601312438));
#22100=DIRECTION('ref_axis',(0.144875601312438,0.,-0.989449877530115));
#22101=DIRECTION('center_axis',(0.952234407172013,0.,0.305368030084627));
#22102=DIRECTION('ref_axis',(0.305368030084627,0.,-0.952234407172013));
#22103=DIRECTION('center_axis',(-0.952234407172012,0.,-0.30536803008463));
#22104=DIRECTION('ref_axis',(-0.30536803008463,0.,0.952234407172012));
#22105=DIRECTION('center_axis',(0.,1.,0.));
#22106=DIRECTION('ref_axis',(-0.96822474174621,0.,0.250081685595898));
#22107=DIRECTION('center_axis',(0.849631715069657,0.,0.527376477241631));
#22108=DIRECTION('ref_axis',(0.527376477241631,0.,-0.849631715069657));
#22109=DIRECTION('center_axis',(0.,-1.,0.));
#22110=DIRECTION('ref_axis',(-0.96822474174621,0.,0.250081685595898));
#22111=DIRECTION('center_axis',(0.849631715069657,0.,0.527376477241631));
#22112=DIRECTION('ref_axis',(0.527376477241631,0.,-0.849631715069657));
#22113=DIRECTION('center_axis',(0.952234407172013,0.,0.305368030084627));
#22114=DIRECTION('ref_axis',(0.305368030084627,0.,-0.952234407172013));
#22115=DIRECTION('center_axis',(-0.952234407172012,1.3243227265015E-15,
-0.30536803008463));
#22116=DIRECTION('ref_axis',(-0.30536803008463,4.13937419839926E-32,0.952234407172012));
#22117=DIRECTION('center_axis',(0.,1.,0.));
#22118=DIRECTION('ref_axis',(0.,0.,1.));
#22119=DIRECTION('center_axis',(0.,1.,0.));
#22120=DIRECTION('ref_axis',(0.,0.,1.));
#22121=DIRECTION('center_axis',(0.,-1.,0.));
#22122=DIRECTION('ref_axis',(0.,0.,-1.));
#22123=DIRECTION('center_axis',(0.,-1.,0.));
#22124=DIRECTION('ref_axis',(0.,0.,-1.));
#22125=DIRECTION('center_axis',(0.,-1.,0.));
#22126=DIRECTION('ref_axis',(0.,0.,-1.));
#22127=DIRECTION('center_axis',(0.,-1.,0.));
#22128=DIRECTION('ref_axis',(0.,0.,-1.));
#22129=DIRECTION('center_axis',(-1.,0.,0.));
#22130=DIRECTION('ref_axis',(0.,0.,1.));
#22131=DIRECTION('center_axis',(0.,1.,0.));
#22132=DIRECTION('ref_axis',(0.,0.,1.));
#22133=DIRECTION('center_axis',(-1.,0.,0.));
#22134=DIRECTION('ref_axis',(0.,0.,-1.));
#22135=DIRECTION('axis',(0.,0.,1.));
#22136=DIRECTION('refdir',(1.,0.,0.));
#22137=DIRECTION('center_axis',(0.,1.,0.));
#22138=DIRECTION('ref_axis',(-0.96822474174621,0.,-0.250081685595898));
#22139=DIRECTION('',(0.,1.,0.));
#22140=DIRECTION('center_axis',(0.,-1.,0.));
#22141=DIRECTION('ref_axis',(0.,0.,-1.));
#22142=DIRECTION('',(0.,1.,0.));
#22143=DIRECTION('center_axis',(0.,1.,0.));
#22144=DIRECTION('ref_axis',(0.,0.,1.));
#22145=DIRECTION('center_axis',(0.432457515077943,0.,0.901654311614274));
#22146=DIRECTION('ref_axis',(0.901654311614274,0.,-0.432457515077943));
#22147=DIRECTION('',(0.,1.,0.));
#22148=DIRECTION('',(0.901654311614274,0.,-0.432457515077943));
#22149=DIRECTION('',(0.,-1.,0.));
#22150=DIRECTION('',(0.901654311614274,0.,-0.432457515077943));
#22151=DIRECTION('center_axis',(0.296407207072259,0.,0.955061656436705));
#22152=DIRECTION('ref_axis',(0.955061656436705,0.,-0.296407207072259));
#22153=DIRECTION('',(0.,1.,0.));
#22154=DIRECTION('',(0.955061656436705,0.,-0.296407207072259));
#22155=DIRECTION('',(0.,1.,0.));
#22156=DIRECTION('',(0.955061656436705,0.,-0.296407207072259));
#22157=DIRECTION('center_axis',(-0.931114934364932,0.,0.364725895711544));
#22158=DIRECTION('ref_axis',(0.364725895711544,0.,0.931114934364932));
#22159=DIRECTION('',(0.,1.,0.));
#22160=DIRECTION('',(0.364725895711544,0.,0.931114934364932));
#22161=DIRECTION('',(0.364725895711544,0.,0.931114934364932));
#22162=DIRECTION('center_axis',(-0.735023390931532,0.,-0.678041750029829));
#22163=DIRECTION('ref_axis',(-0.678041750029829,0.,0.735023390931532));
#22164=DIRECTION('',(0.,1.,0.));
#22165=DIRECTION('',(-0.678041750029829,0.,0.735023390931532));
#22166=DIRECTION('',(-0.678041750029829,0.,0.735023390931532));
#22167=DIRECTION('center_axis',(0.288569434854979,0.,-0.957458971062195));
#22168=DIRECTION('ref_axis',(-0.957458971062195,0.,-0.288569434854979));
#22169=DIRECTION('',(0.,1.,0.));
#22170=DIRECTION('',(-0.957458971062196,0.,-0.288569434854979));
#22171=DIRECTION('',(-0.957458971062196,0.,-0.288569434854979));
#22172=DIRECTION('center_axis',(-0.779581087140967,0.,-0.626301308135395));
#22173=DIRECTION('ref_axis',(-0.626301308135395,0.,0.779581087140967));
#22174=DIRECTION('',(0.,1.,0.));
#22175=DIRECTION('',(-0.626301308135395,0.,0.779581087140967));
#22176=DIRECTION('',(-0.626301308135395,0.,0.779581087140967));
#22177=DIRECTION('center_axis',(-0.872778976562211,0.,0.488115619572884));
#22178=DIRECTION('ref_axis',(0.488115619572884,0.,0.872778976562211));
#22179=DIRECTION('',(0.,1.,0.));
#22180=DIRECTION('',(0.488115619572884,0.,0.872778976562211));
#22181=DIRECTION('',(0.488115619572884,0.,0.872778976562211));
#22182=DIRECTION('center_axis',(-0.82050401645276,0.,-0.571640760429912));
#22183=DIRECTION('ref_axis',(-0.571640760429912,0.,0.82050401645276));
#22184=DIRECTION('',(0.,1.,0.));
#22185=DIRECTION('',(-0.571640760429912,0.,0.82050401645276));
#22186=DIRECTION('',(-0.571640760429912,0.,0.82050401645276));
#22187=DIRECTION('center_axis',(0.155507703829795,0.,-0.987834679513523));
#22188=DIRECTION('ref_axis',(-0.987834679513523,0.,-0.155507703829795));
#22189=DIRECTION('',(0.,1.,0.));
#22190=DIRECTION('',(-0.987834679513523,0.,-0.155507703829795));
#22191=DIRECTION('',(-0.987834679513523,0.,-0.155507703829795));
#22192=DIRECTION('center_axis',(-0.857601377279671,0.,-0.514314959619115));
#22193=DIRECTION('ref_axis',(-0.514314959619115,0.,0.857601377279671));
#22194=DIRECTION('',(0.,1.,0.));
#22195=DIRECTION('',(-0.514314959619115,0.,0.857601377279671));
#22196=DIRECTION('',(-0.514314959619115,0.,0.857601377279671));
#22197=DIRECTION('center_axis',(-0.798184797787376,0.,0.6024126729918));
#22198=DIRECTION('ref_axis',(0.6024126729918,0.,0.798184797787376));
#22199=DIRECTION('',(0.,1.,0.));
#22200=DIRECTION('',(0.6024126729918,0.,0.798184797787376));
#22201=DIRECTION('',(0.6024126729918,0.,0.798184797787376));
#22202=DIRECTION('center_axis',(-0.890700204600685,0.,-0.454591185049047));
#22203=DIRECTION('ref_axis',(-0.454591185049047,0.,0.890700204600686));
#22204=DIRECTION('',(0.,1.,0.));
#22205=DIRECTION('',(-0.454591185049047,0.,0.890700204600686));
#22206=DIRECTION('',(-0.454591185049047,0.,0.890700204600686));
#22207=DIRECTION('center_axis',(0.0195491585141347,0.,-0.999808896940505));
#22208=DIRECTION('ref_axis',(-0.999808896940505,0.,-0.0195491585141347));
#22209=DIRECTION('',(0.,1.,0.));
#22210=DIRECTION('',(-0.999808896940505,0.,-0.0195491585141347));
#22211=DIRECTION('',(-0.999808896940505,0.,-0.0195491585141347));
#22212=DIRECTION('center_axis',(-0.305368030084627,0.,-0.952234407172013));
#22213=DIRECTION('ref_axis',(-0.952234407172013,0.,0.305368030084627));
#22214=DIRECTION('',(0.,-1.,0.));
#22215=DIRECTION('',(-0.952234407172013,0.,0.305368030084627));
#22216=DIRECTION('',(0.,1.,0.));
#22217=DIRECTION('',(-0.952234407172013,0.,0.305368030084627));
#22218=DIRECTION('center_axis',(0.,1.,0.));
#22219=DIRECTION('ref_axis',(0.,0.,1.));
#22220=DIRECTION('',(0.364725895711544,0.,0.931114934364932));
#22221=DIRECTION('',(0.955061656436705,0.,-0.296407207072259));
#22222=DIRECTION('',(0.901654311614274,0.,-0.432457515077943));
#22223=DIRECTION('center_axis',(0.,1.,0.));
#22224=DIRECTION('ref_axis',(0.,0.,1.));
#22225=DIRECTION('center_axis',(0.,1.,0.));
#22226=DIRECTION('ref_axis',(0.,0.,1.));
#22227=DIRECTION('center_axis',(0.,1.,0.));
#22228=DIRECTION('ref_axis',(0.,0.,1.));
#22229=DIRECTION('',(-0.952234407172013,0.,0.305368030084627));
#22230=DIRECTION('center_axis',(0.,1.,0.));
#22231=DIRECTION('ref_axis',(0.,0.,1.));
#22232=DIRECTION('',(-0.999808896940505,0.,-0.0195491585141347));
#22233=DIRECTION('',(-0.454591185049047,0.,0.890700204600686));
#22234=DIRECTION('',(0.6024126729918,0.,0.798184797787376));
#22235=DIRECTION('',(-0.514314959619115,0.,0.857601377279671));
#22236=DIRECTION('',(-0.987834679513523,0.,-0.155507703829795));
#22237=DIRECTION('',(-0.571640760429912,0.,0.82050401645276));
#22238=DIRECTION('',(0.488115619572884,0.,0.872778976562211));
#22239=DIRECTION('',(-0.626301308135395,0.,0.779581087140967));
#22240=DIRECTION('',(-0.957458971062196,0.,-0.288569434854979));
#22241=DIRECTION('',(-0.678041750029829,0.,0.735023390931532));
#22242=DIRECTION('center_axis',(0.,1.,0.));
#22243=DIRECTION('ref_axis',(0.,0.,1.));
#22244=DIRECTION('center_axis',(0.,-1.,0.));
#22245=DIRECTION('ref_axis',(0.,0.,-1.));
#22246=DIRECTION('',(0.6024126729918,0.,0.798184797787376));
#22247=DIRECTION('',(-0.454591185049047,0.,0.890700204600686));
#22248=DIRECTION('',(-0.999808896940505,0.,-0.0195491585141347));
#22249=DIRECTION('center_axis',(0.,-1.,0.));
#22250=DIRECTION('ref_axis',(0.,0.,-1.));
#22251=DIRECTION('',(-0.952234407172013,0.,0.305368030084627));
#22252=DIRECTION('center_axis',(0.,-1.,0.));
#22253=DIRECTION('ref_axis',(0.,0.,-1.));
#22254=DIRECTION('center_axis',(0.,-1.,0.));
#22255=DIRECTION('ref_axis',(0.,0.,-1.));
#22256=DIRECTION('center_axis',(0.,-1.,0.));
#22257=DIRECTION('ref_axis',(0.,0.,-1.));
#22258=DIRECTION('',(0.901654311614274,0.,-0.432457515077943));
#22259=DIRECTION('',(0.955061656436705,0.,-0.296407207072259));
#22260=DIRECTION('',(0.364725895711544,0.,0.931114934364932));
#22261=DIRECTION('',(-0.678041750029829,0.,0.735023390931532));
#22262=DIRECTION('',(-0.957458971062196,0.,-0.288569434854979));
#22263=DIRECTION('',(-0.626301308135395,0.,0.779581087140967));
#22264=DIRECTION('',(0.488115619572884,0.,0.872778976562211));
#22265=DIRECTION('',(-0.571640760429912,0.,0.82050401645276));
#22266=DIRECTION('',(-0.987834679513523,0.,-0.155507703829795));
#22267=DIRECTION('',(-0.514314959619115,0.,0.857601377279671));
#22268=DIRECTION('center_axis',(0.,-1.,0.));
#22269=DIRECTION('ref_axis',(0.,0.,-1.));
#22270=DIRECTION('center_axis',(0.,-1.,0.));
#22271=DIRECTION('ref_axis',(0.,0.,-1.));
#22272=DIRECTION('center_axis',(0.,1.,0.));
#22273=DIRECTION('ref_axis',(0.,0.,1.));
#22274=DIRECTION('center_axis',(0.,1.,0.));
#22275=DIRECTION('ref_axis',(0.,0.,1.));
#22276=DIRECTION('',(0.,-1.,0.));
#22277=DIRECTION('center_axis',(0.,-1.,0.));
#22278=DIRECTION('ref_axis',(0.,0.,-1.));
#22279=DIRECTION('center_axis',(-0.488115619572884,0.,-0.872778976562211));
#22280=DIRECTION('ref_axis',(-0.872778976562211,0.,0.488115619572884));
#22281=DIRECTION('center_axis',(0.0492674350094236,0.,-0.998785622567522));
#22282=DIRECTION('ref_axis',(-0.998785622567522,0.,-0.0492674350094236));
#22283=DIRECTION('center_axis',(0.0833383631889745,0.,-0.996521307961341));
#22284=DIRECTION('ref_axis',(-0.996521307961341,0.,-0.0833383631889746));
#22285=DIRECTION('center_axis',(0.626301308135395,0.,-0.779581087140967));
#22286=DIRECTION('ref_axis',(-0.779581087140968,0.,-0.626301308135395));
#22287=DIRECTION('center_axis',(0.955149485630946,0.,-0.29612406200601));
#22288=DIRECTION('ref_axis',(-0.29612406200601,0.,-0.955149485630946));
#22289=DIRECTION('center_axis',(0.626301308135395,0.,-0.779581087140967));
#22290=DIRECTION('ref_axis',(-0.779581087140968,0.,-0.626301308135395));
#22291=DIRECTION('center_axis',(0.955149485630946,0.,-0.29612406200601));
#22292=DIRECTION('ref_axis',(0.29612406200601,0.,0.955149485630946));
#22293=DIRECTION('center_axis',(0.0833383631889745,0.,-0.996521307961341));
#22294=DIRECTION('ref_axis',(0.996521307961341,0.,0.0833383631889746));
#22295=DIRECTION('center_axis',(-0.488115619572884,0.,-0.872778976562211));
#22296=DIRECTION('ref_axis',(-0.872778976562211,0.,0.488115619572884));
#22297=DIRECTION('center_axis',(0.0492674350094236,0.,-0.998785622567522));
#22298=DIRECTION('ref_axis',(0.998785622567522,0.,0.0492674350094236));
#22299=DIRECTION('center_axis',(0.571640760429912,0.,-0.82050401645276));
#22300=DIRECTION('ref_axis',(-0.82050401645276,0.,-0.571640760429912));
#22301=DIRECTION('center_axis',(0.919859028046646,0.,-0.392249115385974));
#22302=DIRECTION('ref_axis',(-0.392249115385974,0.,-0.919859028046646));
#22303=DIRECTION('center_axis',(0.957458971062196,0.,0.288569434854979));
#22304=DIRECTION('ref_axis',(0.288569434854979,0.,-0.957458971062195));
#22305=DIRECTION('center_axis',(0.964702659073528,0.,-0.263341564468019));
#22306=DIRECTION('ref_axis',(-0.263341564468019,0.,-0.964702659073528));
#22307=DIRECTION('center_axis',(0.957458971062196,0.,0.288569434854979));
#22308=DIRECTION('ref_axis',(0.288569434854979,0.,-0.957458971062195));
#22309=DIRECTION('center_axis',(0.964702659073528,0.,-0.263341564468019));
#22310=DIRECTION('ref_axis',(0.263341564468019,0.,0.964702659073528));
#22311=DIRECTION('center_axis',(0.571640760429912,0.,-0.82050401645276));
#22312=DIRECTION('ref_axis',(-0.82050401645276,0.,-0.571640760429912));
#22313=DIRECTION('center_axis',(0.919859028046646,0.,-0.392249115385974));
#22314=DIRECTION('ref_axis',(0.392249115385974,0.,0.919859028046646));
#22315=DIRECTION('center_axis',(0.987834679513523,0.,0.155507703829795));
#22316=DIRECTION('ref_axis',(0.155507703829795,0.,-0.987834679513523));
#22317=DIRECTION('center_axis',(0.905930950538282,0.,-0.423425451356913));
#22318=DIRECTION('ref_axis',(-0.423425451356913,0.,-0.905930950538282));
#22319=DIRECTION('center_axis',(0.678041750029829,0.,-0.735023390931532));
#22320=DIRECTION('ref_axis',(-0.735023390931532,0.,-0.678041750029829));
#22321=DIRECTION('center_axis',(0.184809846851629,0.,-0.982774297845989));
#22322=DIRECTION('ref_axis',(-0.982774297845989,0.,-0.184809846851629));
#22323=DIRECTION('center_axis',(0.678041750029829,0.,-0.735023390931532));
#22324=DIRECTION('ref_axis',(-0.735023390931532,0.,-0.678041750029829));
#22325=DIRECTION('center_axis',(0.184809846851629,0.,-0.982774297845989));
#22326=DIRECTION('ref_axis',(0.982774297845989,0.,0.184809846851629));
#22327=DIRECTION('center_axis',(0.987834679513523,0.,0.155507703829795));
#22328=DIRECTION('ref_axis',(0.155507703829795,0.,-0.987834679513523));
#22329=DIRECTION('center_axis',(0.905930950538282,0.,-0.423425451356913));
#22330=DIRECTION('ref_axis',(0.423425451356913,0.,0.905930950538282));
#22331=DIRECTION('center_axis',(0.514314959619115,0.,-0.857601377279671));
#22332=DIRECTION('ref_axis',(-0.857601377279671,0.,-0.514314959619115));
#22333=DIRECTION('center_axis',(-0.0531308220811139,0.,-0.998587560379652));
#22334=DIRECTION('ref_axis',(-0.998587560379652,0.,0.0531308220811139));
#22335=DIRECTION('center_axis',(-0.364725895711544,0.,-0.931114934364932));
#22336=DIRECTION('ref_axis',(-0.931114934364932,0.,0.364725895711544));
#22337=DIRECTION('center_axis',(-0.90120055904943,0.,-0.433402298527587));
#22338=DIRECTION('ref_axis',(-0.433402298527587,0.,0.90120055904943));
#22339=DIRECTION('center_axis',(-0.364725895711544,0.,-0.931114934364932));
#22340=DIRECTION('ref_axis',(-0.931114934364932,0.,0.364725895711544));
#22341=DIRECTION('center_axis',(-0.90120055904943,0.,-0.433402298527587));
#22342=DIRECTION('ref_axis',(0.433402298527587,0.,-0.90120055904943));
#22343=DIRECTION('center_axis',(0.514314959619115,0.,-0.857601377279671));
#22344=DIRECTION('ref_axis',(-0.857601377279671,0.,-0.514314959619115));
#22345=DIRECTION('center_axis',(-0.0531308220811139,0.,-0.998587560379652));
#22346=DIRECTION('ref_axis',(0.998587560379652,0.,-0.0531308220811139));
#22347=DIRECTION('center_axis',(-0.6024126729918,0.,-0.798184797787376));
#22348=DIRECTION('ref_axis',(-0.798184797787376,0.,0.6024126729918));
#22349=DIRECTION('center_axis',(-0.087192735929436,0.,-0.996191460915591));
#22350=DIRECTION('ref_axis',(-0.996191460915591,0.,0.087192735929436));
#22351=DIRECTION('center_axis',(-0.955061656436705,0.,0.296407207072259));
#22352=DIRECTION('ref_axis',(0.296407207072259,0.,0.955061656436705));
#22353=DIRECTION('center_axis',(-0.955061656436705,2.56262108120603E-13,
0.29640720707226));
#22354=DIRECTION('ref_axis',(0.29640720707226,-1.35902423770987E-29,0.955061656436705));
#22355=DIRECTION('center_axis',(0.,1.,0.));
#22356=DIRECTION('ref_axis',(0.,0.,1.));
#22357=DIRECTION('center_axis',(0.,1.,0.));
#22358=DIRECTION('ref_axis',(0.,0.,1.));
#22359=DIRECTION('center_axis',(0.,-1.,0.));
#22360=DIRECTION('ref_axis',(0.,0.,-1.));
#22361=DIRECTION('center_axis',(-0.955061656436705,0.,0.296407207072259));
#22362=DIRECTION('ref_axis',(0.296407207072259,0.,0.955061656436705));
#22363=DIRECTION('center_axis',(-0.955061656436693,0.,0.296407207072297));
#22364=DIRECTION('ref_axis',(0.296407207072297,0.,0.955061656436693));
#22365=DIRECTION('center_axis',(-0.6024126729918,0.,-0.798184797787376));
#22366=DIRECTION('ref_axis',(-0.798184797787376,0.,0.6024126729918));
#22367=DIRECTION('center_axis',(-0.087192735929436,0.,-0.996191460915591));
#22368=DIRECTION('ref_axis',(0.996191460915591,0.,-0.087192735929436));
#22369=DIRECTION('center_axis',(0.454591185049047,0.,-0.890700204600686));
#22370=DIRECTION('ref_axis',(-0.890700204600686,0.,-0.454591185049047));
#22371=DIRECTION('center_axis',(0.857880163767375,0.,-0.513849807448113));
#22372=DIRECTION('ref_axis',(-0.513849807448113,0.,-0.857880163767375));
#22373=DIRECTION('center_axis',(-2.49773075486348E-13,-1.,1.04083408558608E-13));
#22374=DIRECTION('ref_axis',(1.,-2.49366499671666E-13,0.));
#22375=DIRECTION('center_axis',(0.901654311614385,0.,-0.432457515077713));
#22376=DIRECTION('ref_axis',(-0.432457515077713,0.,-0.901654311614385));
#22377=DIRECTION('center_axis',(3.92345661168194E-14,1.,-1.73472347597682E-14));
#22378=DIRECTION('ref_axis',(-1.,3.46944695195361E-14,0.));
#22379=DIRECTION('center_axis',(0.901654311614274,-3.98841325780622E-14,
-0.432457515077943));
#22380=DIRECTION('ref_axis',(-0.432457515077943,1.86255736537329E-29,-0.901654311614274));
#22381=DIRECTION('center_axis',(0.454591185049047,0.,-0.890700204600686));
#22382=DIRECTION('ref_axis',(-0.890700204600686,0.,-0.454591185049047));
#22383=DIRECTION('center_axis',(0.857880163767375,0.,-0.513849807448113));
#22384=DIRECTION('ref_axis',(0.513849807448113,0.,0.857880163767375));
#22385=DIRECTION('center_axis',(0.999808896940505,0.,0.0195491585141347));
#22386=DIRECTION('ref_axis',(0.0195491585141347,0.,-0.999808896940505));
#22387=DIRECTION('center_axis',(-0.999808896940505,0.,-0.0195491585141356));
#22388=DIRECTION('ref_axis',(-0.0195491585141356,0.,0.999808896940505));
#22389=DIRECTION('center_axis',(-0.901654311614274,0.,0.432457515077943));
#22390=DIRECTION('ref_axis',(0.432457515077943,0.,0.901654311614274));
#22391=DIRECTION('center_axis',(-0.901654311614274,3.18662470181932E-16,
0.432457515077943));
#22392=DIRECTION('ref_axis',(0.432457515077943,9.83362535564581E-33,0.901654311614274));
#22393=DIRECTION('center_axis',(0.,1.,0.));
#22394=DIRECTION('ref_axis',(0.,0.,1.));
#22395=DIRECTION('center_axis',(0.,1.,0.));
#22396=DIRECTION('ref_axis',(0.,0.,1.));
#22397=DIRECTION('center_axis',(0.,-1.,0.));
#22398=DIRECTION('ref_axis',(0.,0.,-1.));
#22399=DIRECTION('center_axis',(-0.901654311614274,0.,0.432457515077943));
#22400=DIRECTION('ref_axis',(0.432457515077943,0.,0.901654311614274));
#22401=DIRECTION('center_axis',(-0.901654311614275,0.,0.432457515077941));
#22402=DIRECTION('ref_axis',(0.432457515077941,0.,0.901654311614275));
#22403=DIRECTION('center_axis',(0.999808896940505,0.,0.0195491585141347));
#22404=DIRECTION('ref_axis',(0.0195491585141347,0.,-0.999808896940505));
#22405=DIRECTION('center_axis',(-0.999808896940505,0.,-0.0195491585141356));
#22406=DIRECTION('ref_axis',(-0.0195491585141356,0.,0.999808896940505));
#22407=DIRECTION('center_axis',(0.,-1.,0.));
#22408=DIRECTION('ref_axis',(0.,0.,-1.));
#22409=DIRECTION('center_axis',(0.,-1.,0.));
#22410=DIRECTION('ref_axis',(0.,0.,-1.));
#22411=DIRECTION('center_axis',(0.,1.,0.));
#22412=DIRECTION('ref_axis',(0.,0.,1.));
#22413=DIRECTION('center_axis',(0.,-1.,0.));
#22414=DIRECTION('ref_axis',(0.,0.,-1.));
#22415=DIRECTION('center_axis',(0.952234407172013,1.4810129988824E-15,-0.305368030084626));
#22416=DIRECTION('ref_axis',(-0.305368030084626,-8.45556637047479E-33,-0.952234407172013));
#22417=DIRECTION('center_axis',(0.,-1.,0.));
#22418=DIRECTION('ref_axis',(-0.302115636055689,0.,0.95327128481386));
#22419=DIRECTION('center_axis',(0.48796543950748,0.,0.872862950208262));
#22420=DIRECTION('ref_axis',(0.872862950208263,0.,-0.48796543950748));
#22421=DIRECTION('center_axis',(0.,1.,0.));
#22422=DIRECTION('ref_axis',(0.,0.,1.));
#22423=DIRECTION('center_axis',(0.487965439507477,-3.78543962759172E-15,
0.872862950208264));
#22424=DIRECTION('ref_axis',(0.872862950208264,-1.01742962109045E-31,-0.487965439507477));
#22425=DIRECTION('center_axis',(0.,1.,0.));
#22426=DIRECTION('ref_axis',(-0.144875601312395,0.,-0.989449877530121));
#22427=DIRECTION('center_axis',(0.952234407172013,0.,-0.305368030084625));
#22428=DIRECTION('ref_axis',(-0.305368030084625,0.,-0.952234407172013));
#22429=DIRECTION('center_axis',(0.952234407172013,0.,-0.305368030084627));
#22430=DIRECTION('ref_axis',(-0.305368030084627,0.,-0.952234407172013));
#22431=DIRECTION('center_axis',(-0.952234407172011,0.,0.305368030084631));
#22432=DIRECTION('ref_axis',(0.305368030084631,0.,0.952234407172011));
#22433=DIRECTION('center_axis',(0.,-1.,0.));
#22434=DIRECTION('ref_axis',(-0.96822474174621,0.,-0.250081685595898));
#22435=DIRECTION('center_axis',(0.849631715069657,0.,-0.527376477241631));
#22436=DIRECTION('ref_axis',(-0.527376477241631,0.,-0.849631715069657));
#22437=DIRECTION('center_axis',(0.,1.,0.));
#22438=DIRECTION('ref_axis',(-0.96822474174621,0.,-0.250081685595898));
#22439=DIRECTION('center_axis',(0.849631715069657,0.,-0.527376477241631));
#22440=DIRECTION('ref_axis',(-0.527376477241631,0.,-0.849631715069657));
#22441=DIRECTION('center_axis',(0.952234407172013,0.,-0.305368030084627));
#22442=DIRECTION('ref_axis',(-0.305368030084627,0.,-0.952234407172013));
#22443=DIRECTION('center_axis',(-0.952234407172012,0.,0.30536803008463));
#22444=DIRECTION('ref_axis',(0.30536803008463,0.,0.952234407172012));
#22445=DIRECTION('center_axis',(0.,-1.,0.));
#22446=DIRECTION('ref_axis',(0.,0.,-1.));
#22447=DIRECTION('center_axis',(0.,-1.,0.));
#22448=DIRECTION('ref_axis',(0.,0.,-1.));
#22449=DIRECTION('center_axis',(0.,1.,0.));
#22450=DIRECTION('ref_axis',(0.,0.,1.));
#22451=DIRECTION('center_axis',(0.,1.,0.));
#22452=DIRECTION('ref_axis',(0.,0.,1.));
#22453=DIRECTION('center_axis',(0.,1.,0.));
#22454=DIRECTION('ref_axis',(0.,0.,1.));
#22455=DIRECTION('center_axis',(0.,-1.,0.));
#22456=DIRECTION('ref_axis',(0.,0.,-1.));
#22457=DIRECTION('center_axis',(-1.,0.,0.));
#22458=DIRECTION('ref_axis',(0.,0.,1.));
#22459=DIRECTION('center_axis',(0.,1.,0.));
#22460=DIRECTION('ref_axis',(0.,0.,1.));
#22461=DIRECTION('center_axis',(-1.,0.,0.));
#22462=DIRECTION('ref_axis',(0.,0.,-1.));
#22463=DIRECTION('axis',(0.,0.,1.));
#22464=DIRECTION('refdir',(1.,0.,0.));
#22465=DIRECTION('center_axis',(0.,1.,0.));
#22466=DIRECTION('ref_axis',(0.,0.,1.));
#22467=DIRECTION('center_axis',(0.,1.,0.));
#22468=DIRECTION('ref_axis',(0.,0.,1.));
#22469=DIRECTION('',(0.,-1.,0.));
#22470=DIRECTION('center_axis',(0.,-1.,0.));
#22471=DIRECTION('ref_axis',(0.,0.,-1.));
#22472=DIRECTION('center_axis',(0.,-1.,0.));
#22473=DIRECTION('ref_axis',(0.,0.,-1.));
#22474=DIRECTION('center_axis',(0.,1.,0.));
#22475=DIRECTION('ref_axis',(1.22464679914735E-16,0.,-1.));
#22476=DIRECTION('center_axis',(0.,1.,0.));
#22477=DIRECTION('ref_axis',(0.,0.,1.));
#22478=DIRECTION('',(0.,1.,0.));
#22479=DIRECTION('center_axis',(0.,1.,0.));
#22480=DIRECTION('ref_axis',(0.,0.,1.));
#22481=DIRECTION('',(0.,1.,0.));
#22482=DIRECTION('center_axis',(0.998039845995171,0.,-0.0625816730835345));
#22483=DIRECTION('ref_axis',(-0.0625816730835345,0.,-0.998039845995171));
#22484=DIRECTION('',(-0.0625816730835345,0.,-0.998039845995171));
#22485=DIRECTION('',(0.,1.,0.));
#22486=DIRECTION('',(-0.0625816730835345,0.,-0.998039845995171));
#22487=DIRECTION('center_axis',(0.,1.,0.));
#22488=DIRECTION('ref_axis',(0.,0.,1.));
#22489=DIRECTION('center_axis',(0.,1.,0.));
#22490=DIRECTION('ref_axis',(0.,0.,1.));
#22491=DIRECTION('',(0.,1.,0.));
#22492=DIRECTION('center_axis',(0.,1.,0.));
#22493=DIRECTION('ref_axis',(0.,0.,1.));
#22494=DIRECTION('center_axis',(-0.998039845995171,0.,-0.0625816730835345));
#22495=DIRECTION('ref_axis',(-0.0625816730835345,0.,0.998039845995171));
#22496=DIRECTION('',(-0.0625816730835345,0.,0.998039845995171));
#22497=DIRECTION('',(-0.0625816730835345,0.,0.998039845995171));
#22498=DIRECTION('center_axis',(0.,1.,0.));
#22499=DIRECTION('ref_axis',(0.,0.,1.));
#22500=DIRECTION('center_axis',(0.,1.,0.));
#22501=DIRECTION('ref_axis',(0.,0.,1.));
#22502=DIRECTION('axis',(0.,0.,1.));
#22503=DIRECTION('refdir',(1.,0.,0.));
#22504=DIRECTION('center_axis',(1.33376816360845E-16,-1.,0.));
#22505=DIRECTION('ref_axis',(1.,1.33376816360845E-16,0.));
#22506=DIRECTION('center_axis',(1.33376816360845E-16,-1.,0.));
#22507=DIRECTION('ref_axis',(1.,1.33376816360845E-16,0.));
#22508=DIRECTION('center_axis',(1.33376816360845E-16,-1.,0.));
#22509=DIRECTION('ref_axis',(1.,1.33376816360845E-16,0.));
#22510=DIRECTION('center_axis',(-1.33376816360845E-16,1.,0.));
#22511=DIRECTION('ref_axis',(-1.,-1.33376816360845E-16,0.));
#22512=DIRECTION('center_axis',(1.33376816360845E-16,-1.,0.));
#22513=DIRECTION('ref_axis',(1.,1.33376816360845E-16,0.));
#22514=DIRECTION('center_axis',(1.33376816360845E-16,-1.,0.));
#22515=DIRECTION('ref_axis',(1.,1.33376816360845E-16,0.));
#22516=DIRECTION('',(1.33376816360845E-16,-1.,0.));
#22517=DIRECTION('center_axis',(-1.33376816360845E-16,1.,0.));
#22518=DIRECTION('ref_axis',(-1.,-1.33376816360845E-16,0.));
#22519=DIRECTION('center_axis',(-1.33376816360845E-16,1.,0.));
#22520=DIRECTION('ref_axis',(-1.,-1.33376816360845E-16,0.));
#22521=DIRECTION('center_axis',(-1.33376816360845E-16,1.,0.));
#22522=DIRECTION('ref_axis',(-1.,-1.33376816360845E-16,0.));
#22523=DIRECTION('center_axis',(-1.33376816360845E-16,1.,0.));
#22524=DIRECTION('ref_axis',(-1.,-1.33376816360845E-16,0.));
#22525=DIRECTION('center_axis',(-1.33376816360845E-16,1.,0.));
#22526=DIRECTION('ref_axis',(-1.,-1.33376816360845E-16,0.));
#22527=DIRECTION('',(-1.33376816360845E-16,1.,0.));
#22528=DIRECTION('center_axis',(-1.33376816360845E-16,1.,0.));
#22529=DIRECTION('ref_axis',(-1.,-1.32513598859339E-16,0.));
#22530=DIRECTION('center_axis',(-1.22464679914735E-16,-1.63339491236773E-32,
-1.));
#22531=DIRECTION('ref_axis',(1.,1.31067995962692E-16,-1.22464679914735E-16));
#22532=DIRECTION('center_axis',(1.33376816360845E-16,-1.,0.));
#22533=DIRECTION('ref_axis',(1.,1.92747052886312E-16,0.));
#22534=DIRECTION('center_axis',(1.22464679914735E-16,1.63339491236773E-32,
-1.));
#22535=DIRECTION('ref_axis',(-1.,-2.46716227694479E-16,-1.22464679914735E-16));
#22536=DIRECTION('axis',(0.,0.,1.));
#22537=DIRECTION('refdir',(1.,0.,0.));
#22538=DIRECTION('center_axis',(-1.,6.12323399573677E-17,0.));
#22539=DIRECTION('ref_axis',(0.,1.,0.));
#22540=DIRECTION('center_axis',(0.104528463267654,-0.241206989505463,-0.964827958021851));
#22541=DIRECTION('ref_axis',(1.25352732846412E-16,0.970142500145332,-0.242535625036333));
#22542=DIRECTION('center_axis',(0.104528463267654,0.994521895368273,0.));
#22543=DIRECTION('ref_axis',(-0.994521895368273,0.104528463267654,0.));
#22544=DIRECTION('center_axis',(0.104528463267654,-0.241206989505463,0.964827958021851));
#22545=DIRECTION('ref_axis',(-1.25352732846412E-16,-0.970142500145332,-0.242535625036333));
#22546=DIRECTION('center_axis',(0.104528463267654,0.497260947684128,0.861281226008779));
#22547=DIRECTION('ref_axis',(-4.48880618532109E-17,-0.866025403784444,0.499999999999991));
#22548=DIRECTION('center_axis',(0.104528463267654,0.861281226008788,0.497260947684113));
#22549=DIRECTION('ref_axis',(4.7859022490904E-17,-0.499999999999977,0.866025403784452));
#22550=DIRECTION('center_axis',(0.104528463267654,0.964827958021848,-0.241206989505473));
#22551=DIRECTION('ref_axis',(3.35494973080118E-17,0.242535625036343,0.970142500145329));
#22552=DIRECTION('center_axis',(0.104528463267654,1.0442123953466E-14,0.994521895368273));
#22553=DIRECTION('ref_axis',(0.994521895368273,2.35340993718907E-32,-0.104528463267654));
#22554=DIRECTION('center_axis',(0.104528463267654,-0.964827958021853,-0.241206989505453));
#22555=DIRECTION('ref_axis',(-1.87869149990428E-17,0.242535625036323,-0.970142500145334));
#22556=DIRECTION('center_axis',(0.104528463267654,-0.861281226008775,0.497260947684136));
#22557=DIRECTION('ref_axis',(-8.84532624015479E-17,-0.499999999999999,-0.866025403784439));
#22558=DIRECTION('center_axis',(0.104528463267654,-0.497260947684123,0.861281226008782));
#22559=DIRECTION('ref_axis',(-4.87589202125001E-17,-0.866025403784447,-0.499999999999986));
#22560=DIRECTION('center_axis',(0.104528463267654,0.241206989505469,0.964827958021849));
#22561=DIRECTION('ref_axis',(3.21756749545783E-17,-0.97014250014533,0.242535625036339));
#22562=DIRECTION('center_axis',(0.104528463267654,-0.994521895368273,6.81008083921694E-15));
#22563=DIRECTION('ref_axis',(0.994521895368273,0.104528463267654,-2.74588614067193E-32));
#22564=DIRECTION('center_axis',(0.,1.22464679914735E-16,1.));
#22565=DIRECTION('ref_axis',(0.,-1.,1.22464679914735E-16));
#22566=DIRECTION('center_axis',(-1.,0.,0.));
#22567=DIRECTION('ref_axis',(0.,0.,1.));
#22568=DIRECTION('center_axis',(-1.,0.,0.));
#22569=DIRECTION('ref_axis',(0.,0.,1.));
#22570=DIRECTION('center_axis',(0.104528463267654,-0.994521895368273,6.81008083921694E-15));
#22571=DIRECTION('ref_axis',(0.994521895368273,0.104528463267654,-2.74588614067193E-32));
#22572=DIRECTION('center_axis',(0.104528463267654,0.241206989505456,-0.964827958021853));
#22573=DIRECTION('ref_axis',(-2.00678541197572E-17,0.970142500145334,0.242535625036326));
#22574=DIRECTION('center_axis',(0.104528463267654,-0.497260947684145,-0.861281226008769));
#22575=DIRECTION('ref_axis',(-1.75746881493118E-17,0.866025403784434,-0.500000000000009));
#22576=DIRECTION('center_axis',(0.104528463267654,-0.861281226008775,-0.497260947684136));
#22577=DIRECTION('ref_axis',(8.84532624015479E-17,0.499999999999999,-0.866025403784439));
#22578=DIRECTION('center_axis',(0.104528463267654,-0.96482795802185,0.241206989505466));
#22579=DIRECTION('ref_axis',(3.16327731693601E-17,-0.242535625036336,-0.970142500145331));
#22580=DIRECTION('center_axis',(0.104528463267654,-3.63204311424904E-15,
-0.994521895368273));
#22581=DIRECTION('ref_axis',(-0.994521895368273,-6.31025267670437E-32,-0.104528463267654));
#22582=DIRECTION('center_axis',(0.104528463267654,0.964827958021852,0.241206989505459));
#22583=DIRECTION('ref_axis',(-2.43308567694987E-17,-0.242535625036329,0.970142500145333));
#22584=DIRECTION('center_axis',(0.104528463267654,0.861281226008778,-0.49726094768413));
#22585=DIRECTION('ref_axis',(5.38148870333637E-17,0.499999999999993,0.866025403784443));
#22586=DIRECTION('center_axis',(0.104528463267654,0.497260947684129,-0.861281226008779));
#22587=DIRECTION('ref_axis',(2.61266480593264E-18,0.866025403784443,0.499999999999992));
#22588=DIRECTION('center_axis',(-1.,0.,0.));
#22589=DIRECTION('ref_axis',(0.,0.,1.));
#22590=DIRECTION('center_axis',(-1.,0.,0.));
#22591=DIRECTION('ref_axis',(0.,0.,1.));
#22592=DIRECTION('center_axis',(-1.,0.,0.));
#22593=DIRECTION('ref_axis',(0.,0.,1.));
#22594=DIRECTION('center_axis',(-1.,0.,0.));
#22595=DIRECTION('ref_axis',(0.,0.,1.));
#22596=DIRECTION('',(1.,0.,0.));
#22597=DIRECTION('center_axis',(-1.,0.,0.));
#22598=DIRECTION('ref_axis',(0.,0.,1.));
#22599=DIRECTION('center_axis',(-1.,0.,0.));
#22600=DIRECTION('ref_axis',(0.,0.,1.));
#22601=DIRECTION('center_axis',(-1.,0.,0.));
#22602=DIRECTION('ref_axis',(0.,0.,1.));
#22603=DIRECTION('center_axis',(-1.,0.,0.));
#22604=DIRECTION('ref_axis',(0.,0.,1.));
#22605=DIRECTION('',(1.,0.,0.));
#22606=DIRECTION('center_axis',(-1.,0.,0.));
#22607=DIRECTION('ref_axis',(0.,0.,1.));
#22608=DIRECTION('center_axis',(-1.,0.,0.));
#22609=DIRECTION('ref_axis',(0.,0.,1.));
#22610=DIRECTION('',(0.866025403784438,6.12323399573678E-17,0.500000000000001));
#22611=DIRECTION('center_axis',(0.104528463267654,-0.241206989505463,-0.964827958021851));
#22612=DIRECTION('ref_axis',(1.25352732846412E-16,0.970142500145332,-0.242535625036333));
#22613=DIRECTION('',(-0.993634572314886,0.0156427600493605,-0.111560032084303));
#22614=DIRECTION('',(0.,-0.970142500145332,0.242535625036332));
#22615=DIRECTION('',(-0.985727427293419,0.103604127426078,-0.132693722013437));
#22616=DIRECTION('center_axis',(0.104528463267654,0.994521895368273,0.));
#22617=DIRECTION('ref_axis',(-0.994521895368273,0.104528463267654,0.));
#22618=DIRECTION('',(0.,0.,-1.));
#22619=DIRECTION('',(-0.985727427293419,0.103604127426078,0.132693722013437));
#22620=DIRECTION('center_axis',(0.104528463267654,-0.241206989505463,0.964827958021851));
#22621=DIRECTION('ref_axis',(-1.25352732846412E-16,-0.970142500145332,-0.242535625036333));
#22622=DIRECTION('',(0.,0.970142500145332,0.242535625036332));
#22623=DIRECTION('',(-0.993634572314886,0.0156427600493605,0.111560032084303));
#22624=DIRECTION('center_axis',(0.104528463267654,0.497260947684128,0.861281226008779));
#22625=DIRECTION('ref_axis',(-4.48880618532109E-17,-0.866025403784444,0.499999999999991));
#22626=DIRECTION('',(0.,0.866025403784443,-0.499999999999992));
#22627=DIRECTION('',(-0.994132040497618,0.0764901498757915,0.0764901498757902));
#22628=DIRECTION('center_axis',(0.104528463267654,0.861281226008788,0.497260947684113));
#22629=DIRECTION('ref_axis',(4.7859022490904E-17,-0.499999999999977,0.866025403784452));
#22630=DIRECTION('',(0.,0.499999999999977,-0.866025403784452));
#22631=DIRECTION('',(-0.993634572314886,0.111560032084303,0.0156427600493589));
#22632=DIRECTION('center_axis',(0.104528463267654,0.964827958021848,-0.241206989505473));
#22633=DIRECTION('ref_axis',(3.35494973080118E-17,0.242535625036343,0.970142500145329));
#22634=DIRECTION('',(0.,-0.242535625036343,-0.970142500145329));
#22635=DIRECTION('',(-0.985727427293419,0.132693722013438,0.103604127426076));
#22636=DIRECTION('center_axis',(0.104528463267654,1.0442123953466E-14,0.994521895368273));
#22637=DIRECTION('ref_axis',(0.994521895368273,2.35340993718907E-32,-0.104528463267654));
#22638=DIRECTION('',(0.,1.,-1.04996420914386E-14));
#22639=DIRECTION('',(-0.985727427293419,-0.132693722013436,0.103604127426079));
#22640=DIRECTION('center_axis',(0.104528463267654,-0.964827958021853,-0.241206989505453));
#22641=DIRECTION('ref_axis',(-1.87869149990428E-17,0.242535625036323,-0.970142500145334));
#22642=DIRECTION('',(0.,-0.242535625036323,0.970142500145334));
#22643=DIRECTION('',(-0.993634572314887,-0.111560032084302,0.0156427600493615));
#22644=DIRECTION('center_axis',(0.104528463267654,-0.861281226008775,0.497260947684136));
#22645=DIRECTION('ref_axis',(-8.84532624015479E-17,-0.499999999999999,-0.866025403784439));
#22646=DIRECTION('',(0.,0.5,0.866025403784439));
#22647=DIRECTION('',(-0.994132040497618,-0.07649014987579,0.0764901498757912));
#22648=DIRECTION('center_axis',(0.104528463267654,-0.497260947684123,0.861281226008782));
#22649=DIRECTION('ref_axis',(-4.87589202125001E-17,-0.866025403784447,-0.499999999999986));
#22650=DIRECTION('',(0.,0.866025403784447,0.499999999999986));
#22651=DIRECTION('',(-0.993634572314886,-0.0156427600493598,0.111560032084303));
#22652=DIRECTION('center_axis',(0.104528463267654,0.241206989505469,0.964827958021849));
#22653=DIRECTION('ref_axis',(3.21756749545783E-17,-0.97014250014533,0.242535625036339));
#22654=DIRECTION('',(0.,0.97014250014533,-0.242535625036339));
#22655=DIRECTION('',(-0.985727427293419,-0.103604127426077,0.132693722013437));
#22656=DIRECTION('center_axis',(0.104528463267654,-0.994521895368273,6.81008083921694E-15));
#22657=DIRECTION('ref_axis',(0.994521895368273,0.104528463267654,-2.74588614067193E-32));
#22658=DIRECTION('',(0.,6.8475926683295E-15,1.));
#22659=DIRECTION('',(-0.985727427293419,-0.103604127426079,-0.132693722013436));
#22660=DIRECTION('center_axis',(0.104528463267654,0.241206989505456,-0.964827958021853));
#22661=DIRECTION('ref_axis',(-2.00678541197572E-17,0.970142500145334,0.242535625036326));
#22662=DIRECTION('',(0.,-0.970142500145334,-0.242535625036326));
#22663=DIRECTION('',(-0.993634572314886,-0.015642760049362,-0.111560032084303));
#22664=DIRECTION('center_axis',(0.104528463267654,-0.497260947684145,-0.861281226008769));
#22665=DIRECTION('ref_axis',(-1.75746881493119E-17,0.866025403784434,-0.500000000000009));
#22666=DIRECTION('',(0.,-0.866025403784434,0.500000000000009));
#22667=DIRECTION('',(-0.994132040497618,-0.0764901498757908,-0.07649014987579));
#22668=DIRECTION('center_axis',(0.104528463267654,-0.861281226008775,-0.497260947684136));
#22669=DIRECTION('ref_axis',(8.84532624015479E-17,0.499999999999999,-0.866025403784439));
#22670=DIRECTION('',(0.,-0.5,0.866025403784439));
#22671=DIRECTION('',(-0.993634572314886,-0.111560032084303,-0.0156427600493608));
#22672=DIRECTION('center_axis',(0.104528463267654,-0.96482795802185,0.241206989505466));
#22673=DIRECTION('ref_axis',(3.16327731693601E-17,-0.242535625036336,-0.970142500145331));
#22674=DIRECTION('',(0.,0.242535625036336,0.970142500145331));
#22675=DIRECTION('',(-0.985727427293419,-0.132693722013437,-0.103604127426077));
#22676=DIRECTION('center_axis',(0.104528463267654,-3.63204311424904E-15,
-0.994521895368273));
#22677=DIRECTION('ref_axis',(-0.994521895368273,-6.31025267670437E-32,-0.104528463267654));
#22678=DIRECTION('',(0.,-1.,3.65204942310906E-15));
#22679=DIRECTION('',(-0.985727427293419,0.132693722013436,-0.103604127426078));
#22680=DIRECTION('center_axis',(0.104528463267654,0.964827958021852,0.241206989505459));
#22681=DIRECTION('ref_axis',(-2.43308567694987E-17,-0.242535625036329,0.970142500145333));
#22682=DIRECTION('',(0.,0.242535625036329,-0.970142500145333));
#22683=DIRECTION('',(-0.993634572314886,0.111560032084303,-0.0156427600493608));
#22684=DIRECTION('center_axis',(0.104528463267654,0.861281226008778,-0.49726094768413));
#22685=DIRECTION('ref_axis',(5.38148870333637E-17,0.499999999999993,0.866025403784443));
#22686=DIRECTION('',(0.,-0.499999999999993,-0.866025403784443));
#22687=DIRECTION('',(-0.994132040497618,0.0764901498757906,-0.0764901498757907));
#22688=DIRECTION('center_axis',(0.104528463267654,0.497260947684129,-0.861281226008779));
#22689=DIRECTION('ref_axis',(2.61266480593264E-18,0.866025403784443,0.499999999999992));
#22690=DIRECTION('',(0.,-0.866025403784443,-0.499999999999992));
#22691=DIRECTION('center_axis',(-1.,0.,0.));
#22692=DIRECTION('ref_axis',(0.,0.,1.));
#22693=DIRECTION('center_axis',(-1.,0.,0.));
#22694=DIRECTION('ref_axis',(0.,0.,1.));
#22695=DIRECTION('center_axis',(0.,1.,-1.22464679914735E-16));
#22696=DIRECTION('ref_axis',(0.,-1.22464679914735E-16,-1.));
#22697=DIRECTION('axis',(0.,0.,1.));
#22698=DIRECTION('refdir',(1.,0.,0.));
#22699=DIRECTION('center_axis',(0.,-1.,0.));
#22700=DIRECTION('ref_axis',(-1.,0.,-6.12323399573676E-17));
#22701=DIRECTION('',(0.,-1.,0.));
#22702=DIRECTION('center_axis',(0.,1.,0.));
#22703=DIRECTION('ref_axis',(0.,0.,1.));
#22704=DIRECTION('',(0.,-1.,0.));
#22705=DIRECTION('center_axis',(0.,1.,0.));
#22706=DIRECTION('ref_axis',(0.,0.,1.));
#22707=DIRECTION('center_axis',(0.,-1.,0.));
#22708=DIRECTION('ref_axis',(1.,0.,1.83697019872103E-16));
#22709=DIRECTION('center_axis',(0.,1.,0.));
#22710=DIRECTION('ref_axis',(0.,0.,1.));
#22711=DIRECTION('center_axis',(0.,1.,0.));
#22712=DIRECTION('ref_axis',(0.,0.,1.));
#22713=DIRECTION('center_axis',(0.,1.,0.));
#22714=DIRECTION('ref_axis',(0.,0.,1.));
#22715=DIRECTION('center_axis',(0.,1.,0.));
#22716=DIRECTION('ref_axis',(0.,0.,1.));
#22717=DIRECTION('center_axis',(0.,1.,0.));
#22718=DIRECTION('ref_axis',(0.,0.,1.));
#22719=DIRECTION('center_axis',(0.,1.,0.));
#22720=DIRECTION('ref_axis',(0.,0.,1.));
#22721=DIRECTION('center_axis',(0.,1.,0.));
#22722=DIRECTION('ref_axis',(0.,0.,1.));
#22723=DIRECTION('center_axis',(0.,1.,0.));
#22724=DIRECTION('ref_axis',(0.,0.,1.));
#22725=DIRECTION('center_axis',(0.,1.,0.));
#22726=DIRECTION('ref_axis',(0.,0.,1.));
#22727=DIRECTION('center_axis',(0.,1.,0.));
#22728=DIRECTION('ref_axis',(0.,0.,1.));
#22729=DIRECTION('center_axis',(0.,1.,0.));
#22730=DIRECTION('ref_axis',(0.,0.,1.));
#22731=DIRECTION('center_axis',(0.,1.,0.));
#22732=DIRECTION('ref_axis',(0.,0.,1.));
#22733=DIRECTION('center_axis',(0.,1.,0.));
#22734=DIRECTION('ref_axis',(0.,0.,1.));
#22735=DIRECTION('center_axis',(0.,1.,0.));
#22736=DIRECTION('ref_axis',(0.,0.,1.));
#22737=DIRECTION('center_axis',(0.,1.,0.));
#22738=DIRECTION('ref_axis',(0.,0.,1.));
#22739=DIRECTION('center_axis',(0.,1.,0.));
#22740=DIRECTION('ref_axis',(0.,0.,1.));
#22741=DIRECTION('center_axis',(0.,-1.,0.));
#22742=DIRECTION('ref_axis',(0.,0.,-1.));
#22743=DIRECTION('center_axis',(0.,1.,0.));
#22744=DIRECTION('ref_axis',(0.,0.,1.));
#22745=DIRECTION('center_axis',(0.,1.,0.));
#22746=DIRECTION('ref_axis',(0.,0.,1.));
#22747=DIRECTION('',(0.,-1.,0.));
#22748=DIRECTION('center_axis',(0.,1.,0.));
#22749=DIRECTION('ref_axis',(0.,0.,1.));
#22750=DIRECTION('center_axis',(0.,1.,0.));
#22751=DIRECTION('ref_axis',(0.,0.,1.));
#22752=DIRECTION('center_axis',(0.,-1.,0.));
#22753=DIRECTION('ref_axis',(0.,0.,-1.));
#22754=DIRECTION('center_axis',(0.,1.,0.));
#22755=DIRECTION('ref_axis',(0.,0.,1.));
#22756=DIRECTION('center_axis',(0.,1.,0.));
#22757=DIRECTION('ref_axis',(0.,0.,1.));
#22758=DIRECTION('',(0.,-1.,0.));
#22759=DIRECTION('center_axis',(0.,1.,0.));
#22760=DIRECTION('ref_axis',(0.,0.,1.));
#22761=DIRECTION('center_axis',(0.,1.,0.));
#22762=DIRECTION('ref_axis',(0.,0.,1.));
#22763=DIRECTION('center_axis',(0.,-1.,0.));
#22764=DIRECTION('ref_axis',(0.,0.,-1.));
#22765=DIRECTION('center_axis',(0.,1.,0.));
#22766=DIRECTION('ref_axis',(0.,0.,1.));
#22767=DIRECTION('center_axis',(0.,1.,0.));
#22768=DIRECTION('ref_axis',(0.,0.,1.));
#22769=DIRECTION('',(0.,-1.,0.));
#22770=DIRECTION('center_axis',(0.,1.,0.));
#22771=DIRECTION('ref_axis',(0.,0.,1.));
#22772=DIRECTION('center_axis',(0.,1.,0.));
#22773=DIRECTION('ref_axis',(0.,0.,1.));
#22774=DIRECTION('center_axis',(0.,-1.,0.));
#22775=DIRECTION('ref_axis',(0.,0.,-1.));
#22776=DIRECTION('center_axis',(0.,1.,0.));
#22777=DIRECTION('ref_axis',(0.,0.,1.));
#22778=DIRECTION('center_axis',(0.,1.,0.));
#22779=DIRECTION('ref_axis',(0.,0.,1.));
#22780=DIRECTION('',(0.,-1.,0.));
#22781=DIRECTION('center_axis',(0.,1.,0.));
#22782=DIRECTION('ref_axis',(0.,0.,1.));
#22783=DIRECTION('center_axis',(0.,1.,0.));
#22784=DIRECTION('ref_axis',(0.,0.,1.));
#22785=DIRECTION('center_axis',(0.,1.,0.));
#22786=DIRECTION('ref_axis',(-1.,0.,-1.83697019872103E-16));
#22787=DIRECTION('center_axis',(0.,1.,0.));
#22788=DIRECTION('ref_axis',(1.,0.,-1.60812264967664E-16));
#22789=DIRECTION('center_axis',(0.,1.,0.));
#22790=DIRECTION('ref_axis',(0.,0.,1.));
#22791=DIRECTION('center_axis',(-1.,0.,2.41352831440251E-16));
#22792=DIRECTION('ref_axis',(-2.41352831440251E-16,0.,-1.));
#22793=DIRECTION('center_axis',(0.,1.,0.));
#22794=DIRECTION('ref_axis',(0.,0.,1.));
#22795=DIRECTION('center_axis',(-1.,0.,0.));
#22796=DIRECTION('ref_axis',(0.,0.,-1.));
#22797=DIRECTION('center_axis',(0.,1.,0.));
#22798=DIRECTION('ref_axis',(0.,0.,1.));
#22799=DIRECTION('center_axis',(-1.,0.,1.22464679914735E-16));
#22800=DIRECTION('ref_axis',(-1.22464679914735E-16,0.,-1.));
#22801=DIRECTION('center_axis',(0.,1.,0.));
#22802=DIRECTION('ref_axis',(0.,0.,1.));
#22803=DIRECTION('center_axis',(-1.,0.,1.22464679914735E-16));
#22804=DIRECTION('ref_axis',(-1.22464679914735E-16,0.,-1.));
#22805=DIRECTION('center_axis',(0.,1.,0.));
#22806=DIRECTION('ref_axis',(-1.,0.,-1.83697019872103E-16));
#22807=DIRECTION('center_axis',(0.,1.,0.));
#22808=DIRECTION('ref_axis',(1.,0.,6.12323399573676E-17));
#22809=DIRECTION('center_axis',(0.,1.,0.));
#22810=DIRECTION('ref_axis',(0.,0.,1.));
#22811=DIRECTION('center_axis',(-1.,0.,2.41352831440251E-16));
#22812=DIRECTION('ref_axis',(-2.41352831440251E-16,0.,-1.));
#22813=DIRECTION('center_axis',(0.,1.,0.));
#22814=DIRECTION('ref_axis',(0.,0.,1.));
#22815=DIRECTION('center_axis',(-1.,0.,0.));
#22816=DIRECTION('ref_axis',(0.,0.,-1.));
#22817=DIRECTION('center_axis',(0.,1.,0.));
#22818=DIRECTION('ref_axis',(0.,0.,1.));
#22819=DIRECTION('center_axis',(-1.,0.,1.22464679914735E-16));
#22820=DIRECTION('ref_axis',(-1.22464679914735E-16,0.,-1.));
#22821=DIRECTION('center_axis',(0.,1.,0.));
#22822=DIRECTION('ref_axis',(0.,0.,1.));
#22823=DIRECTION('center_axis',(-1.,0.,1.22464679914735E-16));
#22824=DIRECTION('ref_axis',(-1.22464679914735E-16,0.,-1.));
#22825=DIRECTION('axis',(0.,0.,1.));
#22826=DIRECTION('refdir',(1.,0.,0.));
#22827=DIRECTION('center_axis',(1.24100495794237E-20,1.,9.9579925010296E-17));
#22828=DIRECTION('ref_axis',(-0.242093751695761,9.66207115918887E-17,-0.970252861572627));
#22829=DIRECTION('',(0.,-1.,0.));
#22830=DIRECTION('center_axis',(4.78776181462468E-8,-0.999999999999989,
1.38777575295897E-7));
#22831=DIRECTION('ref_axis',(0.228625617239181,-1.2415592080664E-7,-0.973514420613268));
#22832=DIRECTION('',(0.,1.,0.));
#22833=DIRECTION('center_axis',(4.78638686561428E-8,0.999999999999989,1.38744664442357E-7));
#22834=DIRECTION('ref_axis',(-0.657176856530054,1.36031932324909E-7,-0.753736412309541));
#22835=DIRECTION('center_axis',(-0.988756381047007,0.,0.149535343443703));
#22836=DIRECTION('ref_axis',(0.149535343443703,0.,0.988756381047007));
#22837=DIRECTION('',(-0.149535343443703,0.,-0.988756381047007));
#22838=DIRECTION('',(0.,-1.,0.));
#22839=DIRECTION('',(-0.149535343443703,0.,-0.988756381047007));
#22840=DIRECTION('',(0.,-1.,0.));
#22841=DIRECTION('center_axis',(-0.754320837054538,0.,0.656505959443889));
#22842=DIRECTION('ref_axis',(0.656505959443889,0.,0.754320837054538));
#22843=DIRECTION('',(0.,-1.,0.));
#22844=DIRECTION('',(-0.656505959443889,0.,-0.754320837054538));
#22845=DIRECTION('',(0.,-1.,0.));
#22846=DIRECTION('',(-0.656505959443889,0.,-0.754320837054538));
#22847=DIRECTION('center_axis',(0.,-1.,0.));
#22848=DIRECTION('ref_axis',(0.,0.,-1.));
#22849=DIRECTION('center_axis',(0.,-1.,0.));
#22850=DIRECTION('ref_axis',(0.,0.,-1.));
#22851=DIRECTION('',(0.,-1.,0.));
#22852=DIRECTION('center_axis',(0.,-1.,0.));
#22853=DIRECTION('ref_axis',(0.,0.,-1.));
#22854=DIRECTION('center_axis',(0.754320837054538,0.,0.656505959443889));
#22855=DIRECTION('ref_axis',(0.656505959443889,0.,-0.754320837054538));
#22856=DIRECTION('',(-0.656505959443889,0.,0.754320837054538));
#22857=DIRECTION('',(0.,-1.,0.));
#22858=DIRECTION('',(-0.656505959443889,0.,0.754320837054538));
#22859=DIRECTION('center_axis',(0.988756381047007,0.,0.149535343443703));
#22860=DIRECTION('ref_axis',(0.149535343443703,0.,-0.988756381047007));
#22861=DIRECTION('',(-0.149535343443703,0.,0.988756381047007));
#22862=DIRECTION('',(0.,-1.,0.));
#22863=DIRECTION('',(-0.149535343443703,0.,0.988756381047007));
#22864=DIRECTION('',(0.,-1.,0.));
#22865=DIRECTION('center_axis',(-1.24149291915094E-20,1.,9.9579925010296E-17));
#22866=DIRECTION('ref_axis',(0.242093751716637,9.66207127726939E-17,-0.970252861567418));
#22867=DIRECTION('',(0.,-1.,0.));
#22868=DIRECTION('center_axis',(-4.78638689058599E-8,-0.999999999999989,
1.38744669549957E-7));
#22869=DIRECTION('ref_axis',(0.657176856532881,-1.36031936363378E-7,-0.753736412307076));
#22870=DIRECTION('',(0.,1.,0.));
#22871=DIRECTION('center_axis',(-4.78776226059778E-8,0.999999999999989,
1.38777586767972E-7));
#22872=DIRECTION('ref_axis',(-0.228625617218267,1.24155931198126E-7,-0.97351442061818));
#22873=DIRECTION('center_axis',(0.,-1.,0.));
#22874=DIRECTION('ref_axis',(-4.27550288255207E-14,0.,1.));
#22875=DIRECTION('center_axis',(0.,-1.,0.));
#22876=DIRECTION('ref_axis',(0.,0.,-1.));
#22877=DIRECTION('center_axis',(0.,-1.,0.));
#22878=DIRECTION('ref_axis',(0.,0.,-1.));
#22879=DIRECTION('center_axis',(0.,-1.,0.));
#22880=DIRECTION('ref_axis',(0.,0.,-1.));
#22881=DIRECTION('center_axis',(0.,-1.,0.));
#22882=DIRECTION('ref_axis',(0.,0.,-1.));
#22883=DIRECTION('center_axis',(0.,-1.,0.));
#22884=DIRECTION('ref_axis',(-0.319023595909223,0.,-0.947746772747419));
#22885=DIRECTION('center_axis',(0.,-1.,0.));
#22886=DIRECTION('ref_axis',(-0.319023595909223,0.,-0.947746772747419));
#22887=DIRECTION('',(-0.149535343443703,0.,-0.988756381047007));
#22888=DIRECTION('',(-0.656505959443889,0.,-0.754320837054538));
#22889=DIRECTION('center_axis',(0.,-1.,0.));
#22890=DIRECTION('ref_axis',(0.,0.,-1.));
#22891=DIRECTION('',(-0.656505959443889,0.,0.754320837054538));
#22892=DIRECTION('',(-0.149535343443703,0.,0.988756381047007));
#22893=DIRECTION('center_axis',(0.,-1.,0.));
#22894=DIRECTION('ref_axis',(0.,0.,-1.));
#22895=DIRECTION('center_axis',(0.,-1.,0.));
#22896=DIRECTION('ref_axis',(0.,0.,-1.));
#22897=DIRECTION('',(-0.656505959443889,0.,-0.754320837054538));
#22898=DIRECTION('',(-0.149535343443703,0.,-0.988756381047007));
#22899=DIRECTION('center_axis',(0.,-1.,0.));
#22900=DIRECTION('ref_axis',(0.,0.,-1.));
#22901=DIRECTION('center_axis',(0.,1.,0.));
#22902=DIRECTION('ref_axis',(-0.319023595909249,0.,0.94774677274741));
#22903=DIRECTION('center_axis',(0.,1.,0.));
#22904=DIRECTION('ref_axis',(-0.319023595909249,0.,0.94774677274741));
#22905=DIRECTION('',(-0.149535343443703,0.,0.988756381047007));
#22906=DIRECTION('',(-0.656505959443889,0.,0.754320837054538));
#22907=DIRECTION('center_axis',(0.,-1.,0.));
#22908=DIRECTION('ref_axis',(0.,0.,-1.));
#22909=DIRECTION('center_axis',(0.,-1.,0.));
#22910=DIRECTION('ref_axis',(0.,0.,-1.));
#22911=DIRECTION('center_axis',(0.,1.,0.));
#22912=DIRECTION('ref_axis',(0.,0.,1.));
#22913=DIRECTION('center_axis',(0.,-1.,0.));
#22914=DIRECTION('ref_axis',(0.,0.,-1.));
#22915=DIRECTION('center_axis',(0.,-1.,0.));
#22916=DIRECTION('ref_axis',(0.,0.,-1.));
#22917=DIRECTION('',(0.,1.,0.));
#22918=DIRECTION('center_axis',(0.,-1.,0.));
#22919=DIRECTION('ref_axis',(0.,0.,-1.));
#22920=DIRECTION('center_axis',(0.,-1.,0.));
#22921=DIRECTION('ref_axis',(0.,0.,-1.));
#22922=DIRECTION('center_axis',(-0.149535343443703,0.,0.988756381047007));
#22923=DIRECTION('ref_axis',(0.988756381047007,0.,0.149535343443703));
#22924=DIRECTION('center_axis',(-0.149535343443704,0.,0.988756381047007));
#22925=DIRECTION('ref_axis',(0.988756381047007,0.,0.149535343443704));
#22926=DIRECTION('center_axis',(0.149535343443704,5.36005908195038E-16,
-0.988756381047007));
#22927=DIRECTION('ref_axis',(-0.988756381047007,1.21230624919584E-32,-0.149535343443704));
#22928=DIRECTION('center_axis',(0.577350269189623,0.577350269189631,0.577350269189624));
#22929=DIRECTION('ref_axis',(-0.707106781186548,0.,0.707106781186547));
#22930=DIRECTION('center_axis',(0.,1.,0.));
#22931=DIRECTION('ref_axis',(0.,0.,1.));
#22932=DIRECTION('center_axis',(0.,1.,0.));
#22933=DIRECTION('ref_axis',(0.,0.,1.));
#22934=DIRECTION('center_axis',(0.,1.,0.));
#22935=DIRECTION('ref_axis',(0.,0.,1.));
#22936=DIRECTION('center_axis',(-0.65650595944389,0.,0.754320837054537));
#22937=DIRECTION('ref_axis',(0.754320837054537,0.,0.656505959443889));
#22938=DIRECTION('center_axis',(0.,-1.,0.));
#22939=DIRECTION('ref_axis',(-0.693236209136321,0.,0.720710453887206));
#22940=DIRECTION('center_axis',(0.,-1.,0.));
#22941=DIRECTION('ref_axis',(0.,0.,-1.));
#22942=DIRECTION('center_axis',(0.,-1.,0.));
#22943=DIRECTION('ref_axis',(0.242097618474639,0.,-0.970251896740691));
#22944=DIRECTION('center_axis',(-0.656505959443889,0.,0.754320837054538));
#22945=DIRECTION('ref_axis',(0.754320837054538,0.,0.656505959443889));
#22946=DIRECTION('center_axis',(0.656505959443889,0.,-0.754320837054538));
#22947=DIRECTION('ref_axis',(-0.754320837054538,0.,-0.656505959443889));
#22948=DIRECTION('center_axis',(0.,-1.,0.));
#22949=DIRECTION('ref_axis',(0.,0.,-1.));
#22950=DIRECTION('center_axis',(0.,-1.,0.));
#22951=DIRECTION('ref_axis',(0.,0.,-1.));
#22952=DIRECTION('center_axis',(0.149535343443703,0.,-0.988756381047007));
#22953=DIRECTION('ref_axis',(-0.988756381047007,0.,-0.149535343443703));
#22954=DIRECTION('center_axis',(-0.149535343443704,-5.36005908195038E-15,
0.988756381047007));
#22955=DIRECTION('ref_axis',(0.988756381047007,-3.32168718654534E-32,0.149535343443704));
#22956=DIRECTION('center_axis',(0.149535343443707,0.,-0.988756381047006));
#22957=DIRECTION('ref_axis',(-0.988756381047006,0.,-0.149535343443707));
#22958=DIRECTION('center_axis',(0.577350269189625,0.577350269189626,0.577350269189626));
#22959=DIRECTION('ref_axis',(-0.707106781186548,0.,0.707106781186547));
#22960=DIRECTION('center_axis',(0.,-1.,0.));
#22961=DIRECTION('ref_axis',(-7.27572790734007E-5,0.,0.999999997353189));
#22962=DIRECTION('center_axis',(-0.759157852463309,0.000273278785289962,
0.650906506621344));
#22963=DIRECTION('ref_axis',(0.011467416751576,0.999850324991952,0.012954766170509));
#22964=DIRECTION('center_axis',(0.,-1.,0.));
#22965=DIRECTION('ref_axis',(0.,0.,-1.));
#22966=DIRECTION('center_axis',(0.656505959443889,0.,0.754320837054538));
#22967=DIRECTION('ref_axis',(0.754320837054538,0.,-0.656505959443889));
#22968=DIRECTION('center_axis',(0.,-1.,4.33680868994202E-15));
#22969=DIRECTION('ref_axis',(0.,-4.33680868994202E-15,-1.));
#22970=DIRECTION('center_axis',(-0.656505959443889,2.86242701599967E-15,
0.754320837054538));
#22971=DIRECTION('ref_axis',(0.754320837054538,8.45944254531623E-32,0.656505959443889));
#22972=DIRECTION('center_axis',(1.43818211772392E-17,-1.,-2.7292332891214E-17));
#22973=DIRECTION('ref_axis',(0.242098473658204,2.63898515742187E-17,-0.970251683354565));
#22974=DIRECTION('center_axis',(8.39371644022886E-16,-1.,-2.61255151017137E-16));
#22975=DIRECTION('ref_axis',(-0.24209847365972,0.,-0.970251683354187));
#22976=DIRECTION('center_axis',(-0.149535343443703,0.,-0.988756381047007));
#22977=DIRECTION('ref_axis',(-0.988756381047007,0.,0.149535343443703));
#22978=DIRECTION('center_axis',(-0.149535343443694,0.,-0.988756381047008));
#22979=DIRECTION('ref_axis',(-0.988756381047008,0.,0.149535343443694));
#22980=DIRECTION('center_axis',(0.149535343443704,6.00856525885051E-15,
0.988756381047007));
#22981=DIRECTION('ref_axis',(0.988756381047007,-1.58953417427367E-31,-0.149535343443704));
#22982=DIRECTION('center_axis',(0.149535343443704,6.00856525885051E-15,
0.988756381047007));
#22983=DIRECTION('ref_axis',(0.988756381047007,-1.58953417427367E-31,-0.149535343443704));
#22984=DIRECTION('center_axis',(-0.656505959443889,0.,-0.754320837054538));
#22985=DIRECTION('ref_axis',(-0.754320837054538,0.,0.656505959443889));
#22986=DIRECTION('center_axis',(0.656505959443889,1.06165855076284E-14,
0.754320837054538));
#22987=DIRECTION('ref_axis',(0.754320837054538,-1.58155227462586E-31,-0.656505959443889));
#22988=DIRECTION('center_axis',(0.656505959443889,0.,-0.754320837054538));
#22989=DIRECTION('ref_axis',(-0.754320837054538,0.,-0.656505959443889));
#22990=DIRECTION('center_axis',(0.656505959443889,0.,-0.754320837054538));
#22991=DIRECTION('ref_axis',(-0.754320837054538,0.,-0.656505959443889));
#22992=DIRECTION('center_axis',(0.,-1.,0.));
#22993=DIRECTION('ref_axis',(-7.273230047561E-5,0.,0.999999997355006));
#22994=DIRECTION('center_axis',(-0.759157804384072,-0.000273319894445015,
0.650906562679307));
#22995=DIRECTION('ref_axis',(0.650906589214572,-1.08983609746617E-5,0.759157830756081));
#22996=DIRECTION('center_axis',(0.577350269189623,0.577350269189631,0.577350269189624));
#22997=DIRECTION('ref_axis',(-0.707106781186548,0.,0.707106781186547));
#22998=DIRECTION('center_axis',(-0.408248290463864,0.816496580927726,-0.408248290463862));
#22999=DIRECTION('ref_axis',(0.707106781186546,0.,-0.707106781186549));
#23000=DIRECTION('center_axis',(0.,1.,0.));
#23001=DIRECTION('ref_axis',(0.,0.,1.));
#23002=DIRECTION('center_axis',(-4.33680868994204E-15,1.,-8.67361737988409E-15));
#23003=DIRECTION('ref_axis',(0.,1.73472347597681E-14,1.));
#23004=DIRECTION('center_axis',(0.,1.,0.));
#23005=DIRECTION('ref_axis',(0.,0.,1.));
#23006=DIRECTION('center_axis',(0.,-1.,0.));
#23007=DIRECTION('ref_axis',(0.,0.,-1.));
#23008=DIRECTION('center_axis',(0.656505959443889,0.,0.754320837054538));
#23009=DIRECTION('ref_axis',(0.754320837054538,0.,-0.656505959443889));
#23010=DIRECTION('center_axis',(0.,-1.,0.));
#23011=DIRECTION('ref_axis',(-0.242097618470637,0.,-0.970251896741689));
#23012=DIRECTION('center_axis',(0.,-1.,0.));
#23013=DIRECTION('ref_axis',(0.693236209130818,0.,0.720710453892499));
#23014=DIRECTION('center_axis',(0.,-1.,0.));
#23015=DIRECTION('ref_axis',(0.,0.,-1.));
#23016=DIRECTION('center_axis',(0.,-1.,0.));
#23017=DIRECTION('ref_axis',(0.,0.,-1.));
#23018=DIRECTION('center_axis',(0.,-1.,0.));
#23019=DIRECTION('ref_axis',(0.,0.,-1.));
#23020=DIRECTION('center_axis',(0.656505959443889,0.,0.754320837054538));
#23021=DIRECTION('ref_axis',(0.754320837054538,0.,-0.656505959443889));
#23022=DIRECTION('center_axis',(0.656505959443887,0.,0.75432083705454));
#23023=DIRECTION('ref_axis',(0.75432083705454,0.,-0.656505959443887));
#23024=DIRECTION('center_axis',(0.577350269189625,0.577350269189626,0.577350269189626));
#23025=DIRECTION('ref_axis',(-0.707106781186548,0.,0.707106781186547));
#23026=DIRECTION('center_axis',(0.1495353434437,0.,0.988756381047007));
#23027=DIRECTION('ref_axis',(0.988756381047007,0.,-0.1495353434437));
#23028=DIRECTION('center_axis',(0.,-1.,-3.25260651745651E-15));
#23029=DIRECTION('ref_axis',(0.,3.25260651745651E-15,-1.));
#23030=DIRECTION('center_axis',(-0.149535343443704,2.68002954097519E-15,
-0.988756381047007));
#23031=DIRECTION('ref_axis',(-0.988756381047007,-1.66084359327267E-32,0.149535343443704));
#23032=DIRECTION('center_axis',(0.149535343443703,0.,0.988756381047007));
#23033=DIRECTION('ref_axis',(0.988756381047007,0.,-0.149535343443703));
#23034=DIRECTION('center_axis',(0.,-1.,0.));
#23035=DIRECTION('ref_axis',(0.,0.,-1.));
#23036=DIRECTION('center_axis',(-1.,0.,-1.22464679914735E-16));
#23037=DIRECTION('ref_axis',(-1.22464679914735E-16,0.,1.));
#23038=DIRECTION('center_axis',(0.,-1.,0.));
#23039=DIRECTION('ref_axis',(0.,0.,-1.));
#23040=DIRECTION('center_axis',(-1.,0.,-1.22464679914735E-16));
#23041=DIRECTION('ref_axis',(-1.22464679914735E-16,0.,1.));
#23042=DIRECTION('axis',(0.,0.,1.));
#23043=DIRECTION('refdir',(1.,0.,0.));
#23044=DIRECTION('center_axis',(0.,-1.,0.));
#23045=DIRECTION('ref_axis',(0.999832864782553,0.,-0.0182823002030212));
#23046=DIRECTION('',(0.,-1.,0.));
#23047=DIRECTION('center_axis',(0.,1.,0.));
#23048=DIRECTION('ref_axis',(0.,0.,1.));
#23049=DIRECTION('',(0.,-1.,0.));
#23050=DIRECTION('center_axis',(0.,1.,0.));
#23051=DIRECTION('ref_axis',(0.,0.,1.));
#23052=DIRECTION('center_axis',(0.,1.,0.));
#23053=DIRECTION('ref_axis',(0.,0.,1.));
#23054=DIRECTION('center_axis',(0.,1.,0.));
#23055=DIRECTION('ref_axis',(0.,0.,1.));
#23056=DIRECTION('center_axis',(0.,1.,0.));
#23057=DIRECTION('ref_axis',(0.,0.,1.));
#23058=DIRECTION('',(0.,1.,0.));
#23059=DIRECTION('center_axis',(0.,1.,0.));
#23060=DIRECTION('ref_axis',(0.,0.,1.));
#23061=DIRECTION('center_axis',(0.,1.,0.));
#23062=DIRECTION('ref_axis',(0.,0.,1.));
#23063=DIRECTION('center_axis',(0.,1.,0.));
#23064=DIRECTION('ref_axis',(0.,0.,1.));
#23065=DIRECTION('',(0.,1.,0.));
#23066=DIRECTION('center_axis',(0.,1.,0.));
#23067=DIRECTION('ref_axis',(0.,0.,1.));
#23068=DIRECTION('',(0.,1.,0.));
#23069=DIRECTION('center_axis',(0.,1.,0.));
#23070=DIRECTION('ref_axis',(0.,0.,1.));
#23071=DIRECTION('',(0.,-1.,0.));
#23072=DIRECTION('center_axis',(0.,1.,0.));
#23073=DIRECTION('ref_axis',(0.,0.,1.));
#23074=DIRECTION('',(0.,-1.,0.));
#23075=DIRECTION('center_axis',(0.,1.,0.));
#23076=DIRECTION('ref_axis',(0.,0.,1.));
#23077=DIRECTION('center_axis',(0.,1.,0.));
#23078=DIRECTION('ref_axis',(0.,0.,1.));
#23079=DIRECTION('center_axis',(0.,1.,0.));
#23080=DIRECTION('ref_axis',(0.,0.,1.));
#23081=DIRECTION('center_axis',(0.,1.,0.));
#23082=DIRECTION('ref_axis',(0.,0.,1.));
#23083=DIRECTION('center_axis',(0.,1.,0.));
#23084=DIRECTION('ref_axis',(0.,0.,1.));
#23085=DIRECTION('center_axis',(0.,1.,0.));
#23086=DIRECTION('ref_axis',(0.,0.,1.));
#23087=DIRECTION('center_axis',(0.,1.,0.));
#23088=DIRECTION('ref_axis',(0.,0.,1.));
#23089=DIRECTION('center_axis',(0.,1.,0.));
#23090=DIRECTION('ref_axis',(0.,0.,1.));
#23091=DIRECTION('center_axis',(0.,1.,0.));
#23092=DIRECTION('ref_axis',(0.,0.,1.));
#23093=DIRECTION('center_axis',(0.,1.,0.));
#23094=DIRECTION('ref_axis',(0.,0.,1.));
#23095=DIRECTION('center_axis',(0.,1.,0.));
#23096=DIRECTION('ref_axis',(0.,0.,1.));
#23097=DIRECTION('center_axis',(0.,1.,0.));
#23098=DIRECTION('ref_axis',(0.,0.,1.));
#23099=DIRECTION('center_axis',(0.,1.,0.));
#23100=DIRECTION('ref_axis',(0.,0.,1.));
#23101=DIRECTION('center_axis',(0.,1.,0.));
#23102=DIRECTION('ref_axis',(0.,0.,1.));
#23103=DIRECTION('center_axis',(0.,1.,0.));
#23104=DIRECTION('ref_axis',(0.,0.,1.));
#23105=DIRECTION('center_axis',(0.,1.,0.));
#23106=DIRECTION('ref_axis',(0.,0.,1.));
#23107=DIRECTION('center_axis',(0.,-1.,0.));
#23108=DIRECTION('ref_axis',(0.240266771391976,0.,0.970706896320859));
#23109=DIRECTION('',(0.,-1.,0.));
#23110=DIRECTION('center_axis',(0.,1.,0.));
#23111=DIRECTION('ref_axis',(0.,0.,1.));
#23112=DIRECTION('',(0.,-1.,0.));
#23113=DIRECTION('center_axis',(0.,-1.,0.));
#23114=DIRECTION('ref_axis',(0.,0.,-1.));
#23115=DIRECTION('center_axis',(0.,1.,0.));
#23116=DIRECTION('ref_axis',(0.,0.,1.));
#23117=DIRECTION('',(0.,-1.,0.));
#23118=DIRECTION('center_axis',(0.,1.,0.));
#23119=DIRECTION('ref_axis',(0.,0.,1.));
#23120=DIRECTION('',(0.,-1.,0.));
#23121=DIRECTION('center_axis',(1.,0.,0.));
#23122=DIRECTION('ref_axis',(0.,0.,-1.));
#23123=DIRECTION('center_axis',(-1.,0.,0.));
#23124=DIRECTION('ref_axis',(0.,-1.55431223447522E-15,-1.));
#23125=DIRECTION('center_axis',(-1.,0.,0.));
#23126=DIRECTION('ref_axis',(0.,-0.493494070811408,-0.869749160433044));
#23127=DIRECTION('center_axis',(1.,0.,0.));
#23128=DIRECTION('ref_axis',(0.,0.,-1.));
#23129=DIRECTION('',(-1.,0.,0.));
#23130=DIRECTION('center_axis',(-1.,0.,0.));
#23131=DIRECTION('ref_axis',(0.,0.,1.));
#23132=DIRECTION('center_axis',(-1.,0.,0.));
#23133=DIRECTION('ref_axis',(0.,0.,1.));
#23134=DIRECTION('center_axis',(1.,0.,0.));
#23135=DIRECTION('ref_axis',(0.,0.,-1.));
#23136=DIRECTION('center_axis',(0.,-1.,0.));
#23137=DIRECTION('ref_axis',(0.,0.,-1.));
#23138=DIRECTION('',(0.,-1.,0.));
#23139=DIRECTION('center_axis',(0.,1.,0.));
#23140=DIRECTION('ref_axis',(0.,0.,1.));
#23141=DIRECTION('',(0.,-1.,0.));
#23142=DIRECTION('center_axis',(0.,1.,0.));
#23143=DIRECTION('ref_axis',(0.,0.,1.));
#23144=DIRECTION('center_axis',(-2.77555756156289E-16,0.,-1.));
#23145=DIRECTION('ref_axis',(-1.,0.,2.77555756156289E-16));
#23146=DIRECTION('',(0.,-1.,0.));
#23147=DIRECTION('',(1.,0.,-2.77555756156289E-16));
#23148=DIRECTION('',(1.,0.,-2.77555756156289E-16));
#23149=DIRECTION('center_axis',(0.,-1.,0.));
#23150=DIRECTION('ref_axis',(0.,0.,-1.));
#23151=DIRECTION('',(0.,-1.,0.));
#23152=DIRECTION('center_axis',(0.,1.,0.));
#23153=DIRECTION('ref_axis',(0.,0.,1.));
#23154=DIRECTION('',(0.,-1.,0.));
#23155=DIRECTION('center_axis',(0.,1.,0.));
#23156=DIRECTION('ref_axis',(0.,0.,1.));
#23157=DIRECTION('center_axis',(-2.77555756156289E-16,0.,-1.));
#23158=DIRECTION('ref_axis',(-1.,0.,2.77555756156289E-16));
#23159=DIRECTION('',(1.,0.,-2.77555756156289E-16));
#23160=DIRECTION('',(0.,-1.,0.));
#23161=DIRECTION('',(1.,0.,-2.77555756156289E-16));
#23162=DIRECTION('center_axis',(0.,-1.,0.));
#23163=DIRECTION('ref_axis',(0.,0.,-1.));
#23164=DIRECTION('center_axis',(0.,1.,0.));
#23165=DIRECTION('ref_axis',(0.,0.,1.));
#23166=DIRECTION('center_axis',(0.,1.,0.));
#23167=DIRECTION('ref_axis',(0.,0.,1.));
#23168=DIRECTION('center_axis',(0.,1.,0.));
#23169=DIRECTION('ref_axis',(0.,0.,1.));
#23170=DIRECTION('',(-0.885876528532327,0.,-0.463921088328083));
#23171=DIRECTION('center_axis',(0.,1.,0.));
#23172=DIRECTION('ref_axis',(0.,0.,1.));
#23173=DIRECTION('',(0.885876528532327,0.,-0.463921088328083));
#23174=DIRECTION('',(0.860841979634012,0.,0.508872367200063));
#23175=DIRECTION('center_axis',(0.,1.,0.));
#23176=DIRECTION('ref_axis',(0.,0.,1.));
#23177=DIRECTION('',(1.,0.,-2.77555756156289E-16));
#23178=DIRECTION('center_axis',(0.,1.,0.));
#23179=DIRECTION('ref_axis',(0.,0.,1.));
#23180=DIRECTION('',(1.,0.,-2.77555756156289E-16));
#23181=DIRECTION('center_axis',(0.,1.,0.));
#23182=DIRECTION('ref_axis',(0.,0.,1.));
#23183=DIRECTION('',(-0.860841979634012,0.,0.508872367200063));
#23184=DIRECTION('center_axis',(0.,1.,0.));
#23185=DIRECTION('ref_axis',(0.,0.,1.));
#23186=DIRECTION('center_axis',(0.,1.,0.));
#23187=DIRECTION('ref_axis',(0.,0.,1.));
#23188=DIRECTION('center_axis',(0.,1.,0.));
#23189=DIRECTION('ref_axis',(0.,0.,1.));
#23190=DIRECTION('center_axis',(0.,1.,0.));
#23191=DIRECTION('ref_axis',(0.,0.,1.));
#23192=DIRECTION('',(-0.860841979634012,0.,0.508872367200063));
#23193=DIRECTION('center_axis',(0.,1.,0.));
#23194=DIRECTION('ref_axis',(0.,0.,1.));
#23195=DIRECTION('',(1.,0.,-2.77555756156289E-16));
#23196=DIRECTION('center_axis',(0.,1.,0.));
#23197=DIRECTION('ref_axis',(0.,0.,1.));
#23198=DIRECTION('',(1.,0.,-2.77555756156289E-16));
#23199=DIRECTION('center_axis',(0.,1.,0.));
#23200=DIRECTION('ref_axis',(0.,0.,1.));
#23201=DIRECTION('',(0.860841979634012,0.,0.508872367200063));
#23202=DIRECTION('center_axis',(0.,1.,0.));
#23203=DIRECTION('ref_axis',(0.,0.,1.));
#23204=DIRECTION('center_axis',(0.,1.,0.));
#23205=DIRECTION('ref_axis',(0.,0.,1.));
#23206=DIRECTION('center_axis',(0.,-1.,0.));
#23207=DIRECTION('ref_axis',(-1.,0.,1.83697019872103E-16));
#23208=DIRECTION('',(0.,-1.,0.));
#23209=DIRECTION('center_axis',(0.,1.,0.));
#23210=DIRECTION('ref_axis',(0.,0.,1.));
#23211=DIRECTION('',(0.,-1.,0.));
#23212=DIRECTION('center_axis',(0.,1.,0.));
#23213=DIRECTION('ref_axis',(0.,0.,1.));
#23214=DIRECTION('center_axis',(0.,-1.,0.));
#23215=DIRECTION('ref_axis',(1.,0.,-5.0532154980743E-16));
#23216=DIRECTION('center_axis',(0.,1.,0.));
#23217=DIRECTION('ref_axis',(0.,0.,1.));
#23218=DIRECTION('center_axis',(0.,1.,0.));
#23219=DIRECTION('ref_axis',(0.,0.,1.));
#23220=DIRECTION('center_axis',(0.,1.,0.));
#23221=DIRECTION('ref_axis',(0.,0.,1.));
#23222=DIRECTION('center_axis',(0.,1.,0.));
#23223=DIRECTION('ref_axis',(0.,0.,1.));
#23224=DIRECTION('center_axis',(0.,1.,0.));
#23225=DIRECTION('ref_axis',(0.,0.,1.));
#23226=DIRECTION('center_axis',(0.,1.,0.));
#23227=DIRECTION('ref_axis',(0.,0.,1.));
#23228=DIRECTION('center_axis',(0.,1.,0.));
#23229=DIRECTION('ref_axis',(0.,0.,1.));
#23230=DIRECTION('center_axis',(0.,1.,0.));
#23231=DIRECTION('ref_axis',(0.,0.,1.));
#23232=DIRECTION('center_axis',(0.,1.,0.));
#23233=DIRECTION('ref_axis',(0.,0.,1.));
#23234=DIRECTION('center_axis',(0.,-1.,0.));
#23235=DIRECTION('ref_axis',(0.,0.,1.));
#23236=DIRECTION('center_axis',(0.,-1.,0.));
#23237=DIRECTION('ref_axis',(0.,0.,-1.));
#23238=DIRECTION('center_axis',(0.,1.,0.));
#23239=DIRECTION('ref_axis',(0.,0.,1.));
#23240=DIRECTION('center_axis',(0.,1.,0.));
#23241=DIRECTION('ref_axis',(0.,0.,1.));
#23242=DIRECTION('center_axis',(0.,1.,0.));
#23243=DIRECTION('ref_axis',(0.,0.,1.));
#23244=DIRECTION('center_axis',(0.,1.,0.));
#23245=DIRECTION('ref_axis',(0.,0.,1.));
#23246=DIRECTION('center_axis',(0.,1.,0.));
#23247=DIRECTION('ref_axis',(0.,0.,1.));
#23248=DIRECTION('center_axis',(0.,1.,0.));
#23249=DIRECTION('ref_axis',(0.,0.,1.));
#23250=DIRECTION('center_axis',(0.,-1.,0.));
#23251=DIRECTION('ref_axis',(0.,0.,-1.));
#23252=DIRECTION('center_axis',(0.,1.,0.));
#23253=DIRECTION('ref_axis',(0.,0.,1.));
#23254=DIRECTION('center_axis',(0.,1.,0.));
#23255=DIRECTION('ref_axis',(0.,0.,1.));
#23256=DIRECTION('',(0.,-1.,0.));
#23257=DIRECTION('center_axis',(0.,1.,0.));
#23258=DIRECTION('ref_axis',(0.,0.,1.));
#23259=DIRECTION('center_axis',(0.,1.,0.));
#23260=DIRECTION('ref_axis',(0.,0.,1.));
#23261=DIRECTION('center_axis',(0.508872367200063,0.,-0.860841979634012));
#23262=DIRECTION('ref_axis',(-0.860841979634012,0.,-0.508872367200063));
#23263=DIRECTION('',(0.860841979634012,0.,0.508872367200063));
#23264=DIRECTION('',(-0.00269325522461897,-0.999995099755979,-0.00159588230306779));
#23265=DIRECTION('',(0.860841979634012,0.,0.508872367200063));
#23266=DIRECTION('',(0.860841979634012,0.,0.508872367200063));
#23267=DIRECTION('',(0.,1.,0.));
#23268=DIRECTION('center_axis',(0.508872367200063,0.,-0.860841979634012));
#23269=DIRECTION('ref_axis',(-0.860841979634012,0.,-0.508872367200063));
#23270=DIRECTION('center_axis',(0.508872367200063,0.,0.860841979634012));
#23271=DIRECTION('ref_axis',(0.860841979634012,0.,-0.508872367200063));
#23272=DIRECTION('',(-0.860841979634012,0.,0.508872367200063));
#23273=DIRECTION('',(-0.0188132396443243,0.999761206246989,0.0111172162725081));
#23274=DIRECTION('',(-0.860841979634012,0.,0.508872367200063));
#23275=DIRECTION('center_axis',(0.508872367200063,0.,0.860841979634012));
#23276=DIRECTION('ref_axis',(0.860841979634012,0.,-0.508872367200063));
#23277=DIRECTION('',(0.,1.,0.));
#23278=DIRECTION('',(-0.860841979634012,0.,0.508872367200063));
#23279=DIRECTION('',(-0.0248338283987128,0.999591512051479,0.0141453173064702));
#23280=DIRECTION('',(0.003001304709461,-0.999994675620979,0.0012809760867381));
#23281=DIRECTION('center_axis',(-1.,0.,0.));
#23282=DIRECTION('ref_axis',(0.,0.,1.));
#23283=DIRECTION('center_axis',(-1.,0.,0.));
#23284=DIRECTION('ref_axis',(0.,0.,1.));
#23285=DIRECTION('center_axis',(0.,0.,-1.));
#23286=DIRECTION('ref_axis',(1.,0.,0.));
#23287=DIRECTION('center_axis',(0.,0.,-1.));
#23288=DIRECTION('ref_axis',(1.,0.,0.));
#23289=DIRECTION('center_axis',(0.,0.,-1.));
#23290=DIRECTION('ref_axis',(1.,0.,0.));
#23291=DIRECTION('center_axis',(0.,0.,-1.));
#23292=DIRECTION('ref_axis',(1.,0.,0.));
#23293=DIRECTION('center_axis',(0.,0.,-1.));
#23294=DIRECTION('ref_axis',(1.,0.,0.));
#23295=DIRECTION('center_axis',(0.,1.,0.));
#23296=DIRECTION('ref_axis',(0.,0.,1.));
#23297=DIRECTION('center_axis',(0.,1.,0.));
#23298=DIRECTION('ref_axis',(0.,0.,1.));
#23299=DIRECTION('',(0.,1.,0.));
#23300=DIRECTION('center_axis',(0.,1.,0.));
#23301=DIRECTION('ref_axis',(0.,0.,1.));
#23302=DIRECTION('',(0.,1.,0.));
#23303=DIRECTION('center_axis',(0.,-1.,0.));
#23304=DIRECTION('ref_axis',(-0.988127879018848,0.,-0.153633637936853));
#23305=DIRECTION('',(0.,-1.,0.));
#23306=DIRECTION('center_axis',(0.,1.,0.));
#23307=DIRECTION('ref_axis',(0.,0.,1.));
#23308=DIRECTION('center_axis',(0.,-1.,0.));
#23309=DIRECTION('ref_axis',(-0.988127879018849,0.,0.153633637936853));
#23310=DIRECTION('center_axis',(0.,1.,0.));
#23311=DIRECTION('ref_axis',(0.,0.,1.));
#23312=DIRECTION('',(0.,-1.,0.));
#23313=DIRECTION('center_axis',(0.,1.,0.));
#23314=DIRECTION('ref_axis',(0.,0.,1.));
#23315=DIRECTION('',(0.860841979634012,0.,0.508872367200063));
#23316=DIRECTION('',(-0.885876528532327,0.,0.463921088328083));
#23317=DIRECTION('center_axis',(0.,1.,0.));
#23318=DIRECTION('ref_axis',(0.,0.,1.));
#23319=DIRECTION('',(0.885876528532327,0.,0.463921088328083));
#23320=DIRECTION('',(-0.860841979634012,0.,0.508872367200063));
#23321=DIRECTION('center_axis',(0.,1.,0.));
#23322=DIRECTION('ref_axis',(0.,0.,1.));
#23323=DIRECTION('center_axis',(0.,1.,0.));
#23324=DIRECTION('ref_axis',(0.,0.,1.));
#23325=DIRECTION('center_axis',(0.,1.,0.));
#23326=DIRECTION('ref_axis',(0.,0.,1.));
#23327=DIRECTION('center_axis',(0.,1.,0.));
#23328=DIRECTION('ref_axis',(0.,0.,1.));
#23329=DIRECTION('',(0.,1.,0.));
#23330=DIRECTION('center_axis',(0.,1.,0.));
#23331=DIRECTION('ref_axis',(0.,0.,1.));
#23332=DIRECTION('',(0.,1.,0.));
#23333=DIRECTION('center_axis',(0.,1.,0.));
#23334=DIRECTION('ref_axis',(0.,0.,1.));
#23335=DIRECTION('center_axis',(0.463921088328083,0.,0.885876528532327));
#23336=DIRECTION('ref_axis',(0.885876528532327,0.,-0.463921088328083));
#23337=DIRECTION('',(0.,1.,0.));
#23338=DIRECTION('',(0.885876528532327,0.,-0.463921088328083));
#23339=DIRECTION('',(-0.885876528532327,0.,0.463921088328083));
#23340=DIRECTION('center_axis',(0.463921088328083,0.,-0.885876528532327));
#23341=DIRECTION('ref_axis',(-0.885876528532327,0.,-0.463921088328083));
#23342=DIRECTION('',(-0.885876528532327,0.,-0.463921088328083));
#23343=DIRECTION('',(0.,1.,0.));
#23344=DIRECTION('',(0.885876528532327,0.,0.463921088328083));
#23345=DIRECTION('center_axis',(-0.509699705555825,-0.478496577218806,-0.715015549303784));
#23346=DIRECTION('ref_axis',(-0.814285578254856,1.53671303241302E-16,0.580464466652485));
#23347=DIRECTION('center_axis',(0.510097528065447,0.478091211432643,-0.715003010771556));
#23348=DIRECTION('ref_axis',(-0.814066621565784,2.26446044253015E-17,-0.580771500378996));
#23349=DIRECTION('center_axis',(-0.377407413767257,0.379597766708892,-0.844671048126507));
#23350=DIRECTION('ref_axis',(2.42466011867008E-16,0.912125144520788,0.409911845075172));
#23351=DIRECTION('center_axis',(-0.376533159226498,0.380305963034329,0.844742655773606));
#23352=DIRECTION('ref_axis',(-3.15051401839995E-16,-0.911852106514195,0.410518861741607));
#23353=DIRECTION('center_axis',(0.993761383166,0.0477842249653497,-0.100771926509617));
#23354=DIRECTION('ref_axis',(-0.100887171794749,0.,-0.99489787343589));
#23355=DIRECTION('center_axis',(0.997000202168049,-0.0364823216717374,-0.06826153442686));
#23356=DIRECTION('ref_axis',(-0.0683070065019442,0.,-0.997664348798103));
#23357=DIRECTION('center_axis',(0.997510682482232,-0.0331317236572203,0.0622473069404123));
#23358=DIRECTION('ref_axis',(0.0622814998737367,0.,-0.998058622914244));
#23359=DIRECTION('center_axis',(0.993950716469454,0.0467448536050328,0.0993825532540959));
#23360=DIRECTION('ref_axis',(0.0994913110012255,0.,-0.99503843093383));
#23361=DIRECTION('center_axis',(0.,1.,0.));
#23362=DIRECTION('ref_axis',(0.240266771391976,0.,-0.97070689632086));
#23363=DIRECTION('center_axis',(-0.87052398911462,0.,-0.492125984251968));
#23364=DIRECTION('ref_axis',(-0.492125984251968,0.,0.87052398911462));
#23365=DIRECTION('center_axis',(-0.99957228042324,0.,0.0292447637959857));
#23366=DIRECTION('ref_axis',(0.0292447637959857,0.,0.99957228042324));
#23367=DIRECTION('center_axis',(0.,1.,0.));
#23368=DIRECTION('ref_axis',(0.,0.,1.));
#23369=DIRECTION('center_axis',(0.,1.,0.));
#23370=DIRECTION('ref_axis',(0.,0.,1.));
#23371=DIRECTION('center_axis',(0.943400802255207,0.,-0.331654830063173));
#23372=DIRECTION('ref_axis',(-0.331654830063173,0.,-0.943400802255207));
#23373=DIRECTION('center_axis',(0.,-1.,0.));
#23374=DIRECTION('ref_axis',(0.,0.,-1.));
#23375=DIRECTION('center_axis',(0.,-1.,0.));
#23376=DIRECTION('ref_axis',(0.,0.,-1.));
#23377=DIRECTION('center_axis',(0.,1.,0.));
#23378=DIRECTION('ref_axis',(0.,0.,1.));
#23379=DIRECTION('center_axis',(0.,1.,0.));
#23380=DIRECTION('ref_axis',(0.,0.,1.));
#23381=DIRECTION('center_axis',(-0.943400802255207,0.,0.331654830063173));
#23382=DIRECTION('ref_axis',(0.331654830063173,0.,0.943400802255207));
#23383=DIRECTION('center_axis',(0.341538277837768,0.,-0.939867865591548));
#23384=DIRECTION('ref_axis',(-0.939867865591548,0.,-0.341538277837768));
#23385=DIRECTION('center_axis',(0.,-1.,0.));
#23386=DIRECTION('ref_axis',(0.41535894332624,0.,0.909657599428988));
#23387=DIRECTION('center_axis',(0.,1.,0.));
#23388=DIRECTION('ref_axis',(0.,0.,1.));
#23389=DIRECTION('center_axis',(0.,1.,0.));
#23390=DIRECTION('ref_axis',(0.,0.,1.));
#23391=DIRECTION('center_axis',(-0.933920684244367,0.,-0.357480286925774));
#23392=DIRECTION('ref_axis',(-0.357480286925774,0.,0.933920684244367));
#23393=DIRECTION('center_axis',(0.,1.,0.));
#23394=DIRECTION('ref_axis',(-0.998212936683536,0.,-0.0597572843896898));
#23395=DIRECTION('center_axis',(0.,1.,0.));
#23396=DIRECTION('ref_axis',(0.,0.,1.));
#23397=DIRECTION('center_axis',(0.,1.,0.));
#23398=DIRECTION('ref_axis',(-0.998212936683537,0.,0.0597572843896886));
#23399=DIRECTION('center_axis',(-0.933920684244367,0.,0.357480286925774));
#23400=DIRECTION('ref_axis',(0.357480286925774,0.,0.933920684244367));
#23401=DIRECTION('center_axis',(0.,1.,0.));
#23402=DIRECTION('ref_axis',(0.41535894332623,0.,-0.909657599428993));
#23403=DIRECTION('center_axis',(0.341538277837768,0.,0.939867865591548));
#23404=DIRECTION('ref_axis',(0.939867865591548,0.,-0.341538277837768));
#23405=DIRECTION('center_axis',(0.,1.,0.));
#23406=DIRECTION('ref_axis',(0.,0.,1.));
#23407=DIRECTION('center_axis',(0.,1.,0.));
#23408=DIRECTION('ref_axis',(0.,0.,1.));
#23409=DIRECTION('center_axis',(0.664990346018686,-0.709768435883733,0.232414730869427));
#23410=DIRECTION('ref_axis',(0.667995465406688,0.704421904797486,0.239941322488609));
#23411=DIRECTION('center_axis',(0.,1.,0.));
#23412=DIRECTION('ref_axis',(0.415358943326241,0.,-0.909657599428988));
#23413=DIRECTION('center_axis',(0.,-1.,0.));
#23414=DIRECTION('ref_axis',(0.,0.,-1.));
#23415=DIRECTION('center_axis',(0.,1.,0.));
#23416=DIRECTION('ref_axis',(0.,0.,1.));
#23417=DIRECTION('center_axis',(0.,1.,0.));
#23418=DIRECTION('ref_axis',(0.,0.,1.));
#23419=DIRECTION('center_axis',(0.943400802255207,0.,0.331654830063173));
#23420=DIRECTION('ref_axis',(0.331654830063173,0.,-0.943400802255207));
#23421=DIRECTION('center_axis',(0.,1.,0.));
#23422=DIRECTION('ref_axis',(0.,0.,1.));
#23423=DIRECTION('center_axis',(-0.99957228042324,0.,-0.0292447637959857));
#23424=DIRECTION('ref_axis',(-0.0292447637959857,0.,0.99957228042324));
#23425=DIRECTION('center_axis',(0.,1.,0.));
#23426=DIRECTION('ref_axis',(0.,0.,1.));
#23427=DIRECTION('center_axis',(0.87052398911462,0.,-0.492125984251969));
#23428=DIRECTION('ref_axis',(-0.492125984251969,0.,-0.87052398911462));
#23429=DIRECTION('center_axis',(-0.859125449034146,0.00660004002305416,
-0.511722485624358));
#23430=DIRECTION('ref_axis',(0.00325484628249352,0.999967079615338,0.00743274251192558));
#23431=DIRECTION('center_axis',(0.,1.,0.));
#23432=DIRECTION('ref_axis',(0.,0.,1.));
#23433=DIRECTION('center_axis',(-0.860841979634013,0.,-0.508872367200061));
#23434=DIRECTION('ref_axis',(-0.508872367200061,0.,0.860841979634013));
#23435=DIRECTION('center_axis',(1.,0.,-2.77555756156291E-16));
#23436=DIRECTION('ref_axis',(-2.77555756156291E-16,0.,-1.));
#23437=DIRECTION('center_axis',(-0.860841979634012,0.,-0.508872367200063));
#23438=DIRECTION('ref_axis',(-0.508872367200063,0.,0.860841979634012));
#23439=DIRECTION('center_axis',(0.860841979634011,0.,0.508872367200065));
#23440=DIRECTION('ref_axis',(0.508872367200065,0.,-0.860841979634011));
#23441=DIRECTION('center_axis',(0.863246210589165,-0.00473021077503891,
0.504760938474315));
#23442=DIRECTION('ref_axis',(0.504766585555321,-4.22748313639192E-18,-0.863255868272451));
#23443=DIRECTION('center_axis',(0.864784496230593,-0.00574209397403801,
0.502110349859464));
#23444=DIRECTION('ref_axis',(-0.283224646410217,0.820121494130974,0.497176562732181));
#23445=DIRECTION('center_axis',(-1.,0.,2.77555756156289E-16));
#23446=DIRECTION('ref_axis',(2.77555756156289E-16,0.,1.));
#23447=DIRECTION('center_axis',(1.,0.,-8.67361737988409E-15));
#23448=DIRECTION('ref_axis',(-8.67361737988409E-15,0.,-1.));
#23449=DIRECTION('center_axis',(-0.860841979634012,0.,-0.508872367200063));
#23450=DIRECTION('ref_axis',(-0.508872367200063,0.,0.860841979634012));
#23451=DIRECTION('center_axis',(-0.860841979634013,-1.05194637034855E-14,
-0.508872367200061));
#23452=DIRECTION('ref_axis',(-0.508872367200061,-3.69238341666438E-31,0.860841979634013));
#23453=DIRECTION('center_axis',(0.,1.,0.));
#23454=DIRECTION('ref_axis',(0.,0.,1.));
#23455=DIRECTION('center_axis',(0.,-1.,0.));
#23456=DIRECTION('ref_axis',(0.,0.,-1.));
#23457=DIRECTION('center_axis',(-9.03800051153415E-15,1.,4.73307385236553E-15));
#23458=DIRECTION('ref_axis',(-1.,-9.03800051153415E-15,0.));
#23459=DIRECTION('center_axis',(-0.195513569438188,0.,0.980700996311077));
#23460=DIRECTION('ref_axis',(-0.980700996311077,0.,-0.195513569438188));
#23461=DIRECTION('center_axis',(-0.000553346312781574,0.999999846903545,
8.62668738358512E-7));
#23462=DIRECTION('ref_axis',(-0.999999846903917,-0.00055334631278159,0.));
#23463=DIRECTION('center_axis',(-0.863024574373895,-0.00477577234771503,
0.505139362973467));
#23464=DIRECTION('ref_axis',(-0.333722054577103,0.756073495912651,-0.563011952863578));
#23465=DIRECTION('center_axis',(0.,1.,0.));
#23466=DIRECTION('ref_axis',(0.,0.,1.));
#23467=DIRECTION('center_axis',(-1.,0.,0.));
#23468=DIRECTION('ref_axis',(0.,0.,1.));
#23469=DIRECTION('center_axis',(-1.7347234759768E-14,1.,8.67361737988401E-15));
#23470=DIRECTION('ref_axis',(-1.,-1.73472347597682E-14,0.));
#23471=DIRECTION('center_axis',(-0.885876528532336,0.,0.463921088328067));
#23472=DIRECTION('ref_axis',(0.463921088328067,0.,0.885876528532336));
#23473=DIRECTION('center_axis',(-0.885876528532327,0.,0.463921088328083));
#23474=DIRECTION('ref_axis',(0.463921088328083,0.,0.885876528532327));
#23475=DIRECTION('center_axis',(-0.885876528532327,0.,0.463921088328084));
#23476=DIRECTION('ref_axis',(0.463921088328084,0.,0.885876528532327));
#23477=DIRECTION('center_axis',(0.863167213322135,-0.00464466166563832,
-0.504896810213445));
#23478=DIRECTION('ref_axis',(-0.504902256341213,0.,-0.863176523974993));
#23479=DIRECTION('center_axis',(-0.859070797571545,0.00649965078107082,
0.511815512953167));
#23480=DIRECTION('ref_axis',(-0.360863243714502,0.701451263689212,-0.614608691774413));
#23481=DIRECTION('center_axis',(1.,0.,-2.77555756156289E-16));
#23482=DIRECTION('ref_axis',(-2.77555756156289E-16,0.,-1.));
#23483=DIRECTION('center_axis',(-1.,0.,3.4302489988858E-15));
#23484=DIRECTION('ref_axis',(3.4302489988858E-15,0.,1.));
#23485=DIRECTION('center_axis',(-0.885876528532327,0.,0.463921088328083));
#23486=DIRECTION('ref_axis',(0.463921088328083,0.,0.885876528532327));
#23487=DIRECTION('center_axis',(0.885876528532327,9.09984937312614E-17,
-0.463921088328084));
#23488=DIRECTION('ref_axis',(-0.463921088328084,-3.29612034119983E-33,-0.885876528532327));
#23489=DIRECTION('center_axis',(0.,1.,0.));
#23490=DIRECTION('ref_axis',(0.,0.,1.));
#23491=DIRECTION('center_axis',(0.885876528532327,0.,0.463921088328083));
#23492=DIRECTION('ref_axis',(0.463921088328083,0.,-0.885876528532327));
#23493=DIRECTION('center_axis',(0.,1.,0.));
#23494=DIRECTION('ref_axis',(0.,0.,1.));
#23495=DIRECTION('center_axis',(-0.860841979634015,0.,0.508872367200058));
#23496=DIRECTION('ref_axis',(0.508872367200058,0.,0.860841979634015));
#23497=DIRECTION('center_axis',(0.,1.,0.));
#23498=DIRECTION('ref_axis',(0.,0.,1.));
#23499=DIRECTION('center_axis',(-0.885876528532327,0.,-0.463921088328084));
#23500=DIRECTION('ref_axis',(-0.463921088328084,0.,0.885876528532327));
#23501=DIRECTION('center_axis',(0.885876528532327,0.,0.463921088328083));
#23502=DIRECTION('ref_axis',(0.463921088328083,0.,-0.885876528532327));
#23503=DIRECTION('center_axis',(-0.195513569438188,0.,-0.980700996311077));
#23504=DIRECTION('ref_axis',(0.980700996311077,0.,-0.195513569438188));
#23505=DIRECTION('center_axis',(0.860841979634012,0.,-0.508872367200063));
#23506=DIRECTION('ref_axis',(-0.508872367200063,0.,-0.860841979634012));
#23507=DIRECTION('center_axis',(0.860841979634013,0.,-0.508872367200061));
#23508=DIRECTION('ref_axis',(-0.508872367200061,0.,-0.860841979634013));
#23509=DIRECTION('center_axis',(0.860841979634012,0.,-0.508872367200063));
#23510=DIRECTION('ref_axis',(-0.508872367200063,0.,-0.860841979634012));
#23511=DIRECTION('center_axis',(-0.860841979634021,0.,0.508872367200048));
#23512=DIRECTION('ref_axis',(0.508872367200048,0.,0.860841979634021));
#23513=DIRECTION('center_axis',(0.885876528532327,0.,0.463921088328083));
#23514=DIRECTION('ref_axis',(0.463921088328083,0.,-0.885876528532327));
#23515=DIRECTION('center_axis',(-0.885876528532327,-1.93913821232359E-14,
-0.463921088328084));
#23516=DIRECTION('ref_axis',(-0.463921088328084,-1.07766259570539E-30,0.885876528532327));
#23517=DIRECTION('center_axis',(0.,-1.,0.));
#23518=DIRECTION('ref_axis',(0.,0.,-1.));
#23519=DIRECTION('center_axis',(-1.7347234759768E-14,1.,0.));
#23520=DIRECTION('ref_axis',(-1.,-1.73472347597682E-14,0.));
#23521=DIRECTION('center_axis',(8.7825899001661E-15,1.,-5.19168142165297E-15));
#23522=DIRECTION('ref_axis',(-1.,8.7825899001661E-15,0.));
#23523=DIRECTION('center_axis',(0.,1.,0.));
#23524=DIRECTION('ref_axis',(0.,0.,1.));
#23525=DIRECTION('center_axis',(0.,1.,0.));
#23526=DIRECTION('ref_axis',(0.,0.,1.));
#23527=DIRECTION('center_axis',(0.,1.,0.));
#23528=DIRECTION('ref_axis',(0.,0.,1.));
#23529=DIRECTION('center_axis',(1.,0.,-1.77635683940025E-16));
#23530=DIRECTION('ref_axis',(-1.77635683940025E-16,0.,-1.));
#23531=DIRECTION('center_axis',(0.,1.,0.));
#23532=DIRECTION('ref_axis',(0.,0.,1.));
#23533=DIRECTION('center_axis',(-1.,0.,2.36217664813863E-16));
#23534=DIRECTION('ref_axis',(-2.36217664813863E-16,0.,-1.));
#23535=DIRECTION('center_axis',(-0.857824537815853,0.,-0.513942664429622));
#23536=DIRECTION('ref_axis',(-0.513942664429622,0.,0.857824537815853));
#23537=DIRECTION('center_axis',(0.860841979634012,0.,0.508872367200063));
#23538=DIRECTION('ref_axis',(0.508872367200063,0.,-0.860841979634012));
#23539=DIRECTION('center_axis',(0.860841979634013,0.,0.508872367200061));
#23540=DIRECTION('ref_axis',(0.508872367200061,0.,-0.860841979634013));
#23541=DIRECTION('center_axis',(-0.86396885760878,-3.77362398313829E-13,
-0.503545244324857));
#23542=DIRECTION('ref_axis',(-0.40193736700939,-0.602372654072851,0.689632901351718));
#23543=DIRECTION('center_axis',(0.,1.,0.));
#23544=DIRECTION('ref_axis',(0.,0.,1.));
#23545=DIRECTION('center_axis',(1.,0.,0.));
#23546=DIRECTION('ref_axis',(0.,0.,-1.));
#23547=DIRECTION('center_axis',(0.000484671251441277,0.999999882395689,
-1.73892337407491E-5));
#23548=DIRECTION('ref_axis',(-0.999999882546882,0.000484671251514543,0.));
#23549=DIRECTION('center_axis',(-0.863965003980117,8.6132890394033E-13,
0.503551856215065));
#23550=DIRECTION('ref_axis',(-6.88338275267738E-13,-1.,5.35682609381748E-13));
#23551=DIRECTION('center_axis',(1.,0.,-2.77555756156289E-16));
#23552=DIRECTION('ref_axis',(-2.77555756156289E-16,0.,-1.));
#23553=DIRECTION('center_axis',(1.,0.,0.));
#23554=DIRECTION('ref_axis',(0.,0.,-1.));
#23555=DIRECTION('center_axis',(0.857823788622072,0.,-0.513943914911028));
#23556=DIRECTION('ref_axis',(-0.513943914911028,0.,-0.857823788622072));
#23557=DIRECTION('center_axis',(0.,1.,0.));
#23558=DIRECTION('ref_axis',(0.,0.,1.));
#23559=DIRECTION('center_axis',(-1.,0.,0.));
#23560=DIRECTION('ref_axis',(0.,0.,1.));
#23561=DIRECTION('center_axis',(-1.,0.,2.77555756156289E-16));
#23562=DIRECTION('ref_axis',(2.77555756156289E-16,0.,1.));
#23563=DIRECTION('center_axis',(-1.,-3.15269324272952E-15,2.7755575615626E-16));
#23564=DIRECTION('ref_axis',(3.15269324272952E-15,-1.,-5.15124444202338E-47));
#23565=DIRECTION('center_axis',(-0.860841979634012,0.,0.508872367200063));
#23566=DIRECTION('ref_axis',(0.508872367200063,0.,0.860841979634012));
#23567=DIRECTION('center_axis',(0.860841979634013,0.,-0.508872367200061));
#23568=DIRECTION('ref_axis',(-0.508872367200061,0.,-0.860841979634013));
#23569=DIRECTION('center_axis',(0.,1.,0.));
#23570=DIRECTION('ref_axis',(0.,0.,1.));
#23571=DIRECTION('center_axis',(0.,1.,0.));
#23572=DIRECTION('ref_axis',(-1.,0.,-1.83697019872103E-16));
#23573=DIRECTION('center_axis',(0.,1.,0.));
#23574=DIRECTION('ref_axis',(1.,0.,6.12323399573677E-17));
#23575=DIRECTION('center_axis',(0.,1.,0.));
#23576=DIRECTION('ref_axis',(0.,0.,1.));
#23577=DIRECTION('center_axis',(-1.,0.,2.36217664813863E-16));
#23578=DIRECTION('ref_axis',(-2.36217664813863E-16,0.,-1.));
#23579=DIRECTION('center_axis',(0.,1.,0.));
#23580=DIRECTION('ref_axis',(0.,0.,1.));
#23581=DIRECTION('center_axis',(-1.,0.,0.));
#23582=DIRECTION('ref_axis',(0.,0.,-1.));
#23583=DIRECTION('center_axis',(1.,0.,0.));
#23584=DIRECTION('ref_axis',(0.,-1.,0.));
#23585=DIRECTION('center_axis',(-0.99957228042324,4.08129586043321E-15,
0.029244763795984));
#23586=DIRECTION('ref_axis',(0.029244763795984,-9.77391875425212E-33,0.99957228042324));
#23587=DIRECTION('center_axis',(0.,1.,0.));
#23588=DIRECTION('ref_axis',(1.,0.,7.04481399828022E-16));
#23589=DIRECTION('center_axis',(-0.87052398911462,0.,0.492125984251969));
#23590=DIRECTION('ref_axis',(0.492125984251969,0.,0.87052398911462));
#23591=DIRECTION('center_axis',(-0.87052398911462,-4.26851249010043E-15,
-0.492125984251969));
#23592=DIRECTION('ref_axis',(-0.492125984251969,3.56763598725556E-30,0.87052398911462));
#23593=DIRECTION('center_axis',(0.492125984251969,0.,0.87052398911462));
#23594=DIRECTION('ref_axis',(0.870523989114618,0.,-0.492125984251973));
#23595=DIRECTION('center_axis',(0.,1.,0.));
#23596=DIRECTION('ref_axis',(0.,0.,1.));
#23597=DIRECTION('center_axis',(0.492125984251969,0.,-0.87052398911462));
#23598=DIRECTION('ref_axis',(-0.870523989114623,0.,-0.492125984251964));
#23599=DIRECTION('center_axis',(0.,1.,0.));
#23600=DIRECTION('ref_axis',(0.,0.,1.));
#23601=DIRECTION('center_axis',(0.,-1.,0.));
#23602=DIRECTION('ref_axis',(-2.20819958125884E-14,0.,1.));
#23603=DIRECTION('center_axis',(0.,1.,0.));
#23604=DIRECTION('ref_axis',(0.,0.,1.));
#23605=DIRECTION('center_axis',(0.,1.,0.));
#23606=DIRECTION('ref_axis',(0.240266771500873,0.,-0.970706896293906));
#23607=DIRECTION('center_axis',(0.,-1.,0.));
#23608=DIRECTION('ref_axis',(0.,0.,-1.));
#23609=DIRECTION('center_axis',(0.851950674417188,3.69474708821441E-15,
-0.523622047244097));
#23610=DIRECTION('ref_axis',(-0.523622047244097,7.84320521258019E-32,-0.851950674417188));
#23611=DIRECTION('center_axis',(0.,1.,0.));
#23612=DIRECTION('ref_axis',(0.,0.,1.));
#23613=DIRECTION('center_axis',(0.875811224577025,6.4333293152058E-5,0.48265380425945));
#23614=DIRECTION('ref_axis',(0.482653805258247,0.,-0.875811226389417));
#23615=DIRECTION('center_axis',(-0.224058013086413,0.885784476176752,0.406428183737356));
#23616=DIRECTION('ref_axis',(0.890655349196501,0.0168104402479641,0.454368196561257));
#23617=DIRECTION('center_axis',(-0.822444407952205,-0.295329920203461,-0.486174283627554));
#23618=DIRECTION('ref_axis',(-0.508872367200061,2.60023830660238E-16,0.860841979634013));
#23619=DIRECTION('center_axis',(-0.00270036335398834,-0.999995105202431,
-0.00158038252836222));
#23620=DIRECTION('ref_axis',(0.509072475055034,-1.44080963018857E-5,-0.860723657705392));
#23621=DIRECTION('center_axis',(0.00227714854045241,0.999996496446841,0.00134969943612062));
#23622=DIRECTION('ref_axis',(-0.999997407289178,0.00227715061458298,-6.8912051966359E-21));
#23623=DIRECTION('center_axis',(0.0027029442948384,0.999995097323232,0.00158095592591226));
#23624=DIRECTION('ref_axis',(0.444580341019544,0.000214448963012711,-0.895738954378221));
#23625=DIRECTION('center_axis',(0.000103527088607853,0.999999992623769,
6.35185350686548E-5));
#23626=DIRECTION('ref_axis',(-0.999999994641071,0.000103527088816698,-3.76084161841949E-23));
#23627=DIRECTION('center_axis',(-0.00214831185033822,0.999997022148358,
-0.00115777830791125));
#23628=DIRECTION('ref_axis',(0.438135237678527,-9.94865870677395E-5,-0.898909063035188));
#23629=DIRECTION('center_axis',(0.819672096105927,-0.305553637946519,0.484535477754687));
#23630=DIRECTION('ref_axis',(0.508872367200059,1.84629072854334E-16,-0.860841979634014));
#23631=DIRECTION('center_axis',(-0.282731426109906,-0.801305881909544,0.527230333257702));
#23632=DIRECTION('ref_axis',(0.407870460957109,-0.59792211370622,-0.690022342406187));
#23633=DIRECTION('center_axis',(0.881188233597026,-0.00024684095531491,
0.472765519089217));
#23634=DIRECTION('ref_axis',(0.472765533492127,-2.08912278962891E-20,-0.881188260442628));
#23635=DIRECTION('center_axis',(0.881643835712412,-0.000205864534824282,
-0.471915357421328));
#23636=DIRECTION('ref_axis',(-0.471915367421263,4.31856925775005E-20,-0.881643854394536));
#23637=DIRECTION('center_axis',(-0.285649301116541,-0.795890144086274,-0.533819590609002));
#23638=DIRECTION('ref_axis',(0.345501431459368,-0.605095435813926,0.717278380000877));
#23639=DIRECTION('center_axis',(-0.81846149474772,0.309901812552962,0.483819850969052));
#23640=DIRECTION('ref_axis',(0.508872367200115,1.08402883170529E-16,0.860841979633981));
#23641=DIRECTION('center_axis',(-0.0235631216677967,0.999626094909593,0.0138726231501557));
#23642=DIRECTION('ref_axis',(0.509367231127245,6.42305444620244E-5,0.860549254678778));
#23643=DIRECTION('center_axis',(-0.0224243417675557,0.999660615912144,0.0132590305243092));
#23644=DIRECTION('ref_axis',(-0.999748498612813,-0.0224263131483262,1.07790531220658E-18));
#23645=DIRECTION('center_axis',(0.0214414384172488,-0.999689035276165,-0.012731750359262));
#23646=DIRECTION('ref_axis',(0.435401828077164,-0.00212657061748541,0.900233706214376));
#23647=DIRECTION('center_axis',(-0.0204053358968825,0.999719111022908,0.0120549293860458));
#23648=DIRECTION('ref_axis',(-0.999791759192672,-0.0204068187236985,-4.51782575218622E-19));
#23649=DIRECTION('center_axis',(0.0187793084075624,-0.999761209584918,-0.0111741391183278));
#23650=DIRECTION('ref_axis',(0.442592142534916,-0.00170892344078755,0.896721403194452));
#23651=DIRECTION('center_axis',(-0.0192244218537273,0.999750649496634,0.0113604769023756));
#23652=DIRECTION('ref_axis',(-0.999815169869054,-0.0192256625299481,-2.76063375332087E-19));
#23653=DIRECTION('center_axis',(0.0188072437744052,-0.999761138089071,-0.0111334787221499));
#23654=DIRECTION('ref_axis',(0.446265374922732,-0.00157069574366981,0.894899294926504));
#23655=DIRECTION('center_axis',(0.821930410018369,0.297254628825937,-0.4858704423286));
#23656=DIRECTION('ref_axis',(-0.508872367200098,1.3431595397086E-16,-0.860841979633991));
#23657=DIRECTION('center_axis',(-0.224582549367916,0.885152773348463,-0.407513492234224));
#23658=DIRECTION('ref_axis',(0.423300985656642,0.465295843830645,0.777377677358981));
#23659=DIRECTION('center_axis',(0.875783254496798,9.66947566949944E-5,-0.482704549173841));
#23660=DIRECTION('ref_axis',(-0.482704551430455,-1.00776139250218E-19,-0.87578325859103));
#23661=DIRECTION('center_axis',(0.,-1.,0.));
#23662=DIRECTION('ref_axis',(0.,0.,-1.));
#23663=DIRECTION('',(0.,-1.,0.));
#23664=DIRECTION('center_axis',(0.,-1.,0.));
#23665=DIRECTION('ref_axis',(0.,0.,-1.));
#23666=DIRECTION('',(0.,-1.,0.));
#23667=DIRECTION('center_axis',(0.,-1.,0.));
#23668=DIRECTION('ref_axis',(0.,0.,-1.));
#23669=DIRECTION('',(0.,-1.,0.));
#23670=DIRECTION('center_axis',(0.,-1.,0.));
#23671=DIRECTION('ref_axis',(0.,0.,-1.));
#23672=DIRECTION('',(0.,-1.,0.));
#23673=DIRECTION('center_axis',(-1.,0.,0.));
#23674=DIRECTION('ref_axis',(0.,0.,1.));
#23675=DIRECTION('center_axis',(0.,-1.,2.22044604925031E-16));
#23676=DIRECTION('ref_axis',(0.,-2.22044604925031E-16,-1.));
#23677=DIRECTION('axis',(0.,0.,1.));
#23678=DIRECTION('refdir',(1.,0.,0.));
#23679=DIRECTION('center_axis',(-6.12323399573677E-17,0.,1.));
#23680=DIRECTION('ref_axis',(-1.,0.,0.));
#23681=DIRECTION('center_axis',(0.,0.,1.));
#23682=DIRECTION('ref_axis',(1.,0.,0.));
#23683=DIRECTION('center_axis',(-1.22464679914735E-16,1.,0.));
#23684=DIRECTION('ref_axis',(1.,1.22464679914735E-16,0.));
#23685=DIRECTION('center_axis',(0.,0.,1.));
#23686=DIRECTION('ref_axis',(1.,0.,0.));
#23687=DIRECTION('center_axis',(0.,0.,1.));
#23688=DIRECTION('ref_axis',(1.,0.,0.));
#23689=DIRECTION('center_axis',(0.,0.,1.));
#23690=DIRECTION('ref_axis',(1.,0.,0.));
#23691=DIRECTION('center_axis',(0.,0.,1.));
#23692=DIRECTION('ref_axis',(1.,0.,0.));
#23693=DIRECTION('',(0.,0.,-1.));
#23694=DIRECTION('center_axis',(0.,0.,1.));
#23695=DIRECTION('ref_axis',(1.,0.,0.));
#23696=DIRECTION('',(0.,1.,0.));
#23697=DIRECTION('',(4.16333634234434E-16,0.,1.));
#23698=DIRECTION('',(0.,1.,0.));
#23699=DIRECTION('',(1.,0.,0.));
#23700=DIRECTION('',(0.,1.,0.));
#23701=DIRECTION('',(1.,0.,0.));
#23702=DIRECTION('',(0.,1.,0.));
#23703=DIRECTION('',(1.,0.,0.));
#23704=DIRECTION('',(0.,1.,0.));
#23705=DIRECTION('',(1.,0.,0.));
#23706=DIRECTION('',(0.,1.,0.));
#23707=DIRECTION('',(1.,0.,0.));
#23708=DIRECTION('',(0.,1.,0.));
#23709=DIRECTION('',(1.,0.,0.));
#23710=DIRECTION('',(7.06766209131827E-16,-6.2450045135165E-16,-1.));
#23711=DIRECTION('',(1.,5.55111512312576E-17,7.06766209131827E-16));
#23712=DIRECTION('',(0.996194698091746,-0.0871557427476585,0.));
#23713=DIRECTION('',(-0.0871557427476585,-0.996194698091746,0.));
#23714=DIRECTION('',(0.,1.,0.));
#23715=DIRECTION('',(1.,0.,0.));
#23716=DIRECTION('',(-0.999507148419871,-0.0294609393212734,0.0108403557084823));
#23717=DIRECTION('',(-0.0142758199078133,0.119025494507007,-0.992788563906395));
#23718=DIRECTION('',(0.,1.,0.));
#23719=DIRECTION('',(1.,0.,0.));
#23720=DIRECTION('',(1.,-3.46944695195361E-17,0.));
#23721=DIRECTION('',(-3.46944695195361E-17,-1.,0.));
#23722=DIRECTION('',(0.,1.,0.));
#23723=DIRECTION('',(1.,0.,0.));
#23724=DIRECTION('',(-5.08974708834442E-17,6.24500451351651E-16,-1.));
#23725=DIRECTION('',(1.,-3.40418406424152E-17,-5.08974708834442E-17));
#23726=CARTESIAN_POINT('',(0.,0.,0.));
#23727=CARTESIAN_POINT('',(0.,0.,0.));
#23728=CARTESIAN_POINT('Origin',(0.012,0.,0.));
#23729=CARTESIAN_POINT('',(0.012,-0.000521792360520078,0.0108614735985732));
#23730=CARTESIAN_POINT('',(0.012,-0.000157005585611549,0.011998972841293));
#23731=CARTESIAN_POINT('Origin',(0.012,0.00400379034671789,0.010037397655502));
#23732=CARTESIAN_POINT('',(0.012,-0.000962038105848782,0.0108313599646072));
#23733=CARTESIAN_POINT('Origin',(0.012,0.,0.));
#23734=CARTESIAN_POINT('',(0.012,-0.00147831669728126,0.0119085926852227));
#23735=CARTESIAN_POINT('Origin',(0.012,-0.00533325763176565,0.00939872607688738));
#23736=CARTESIAN_POINT('',(0.012,-0.0017894031515103,0.0118658348362585));
#23737=CARTESIAN_POINT('Origin',(0.012,0.,0.));
#23738=CARTESIAN_POINT('',(0.012,-0.00199590282248143,0.0106892585300951));
#23739=CARTESIAN_POINT('Origin',(0.012,0.00259974002297311,0.0104890915072804));
#23740=CARTESIAN_POINT('',(0.012,-0.0024279476225516,0.0105994785882205));
#23741=CARTESIAN_POINT('Origin',(0.012,0.,0.));
#23742=CARTESIAN_POINT('',(0.012,-0.00308610073718624,0.0115963779793493));
#23743=CARTESIAN_POINT('Origin',(0.012,-0.00656337641804451,0.008584974014533));
#23744=CARTESIAN_POINT('',(0.012,-0.00338846752237721,0.0115116587792461));
#23745=CARTESIAN_POINT('Origin',(0.012,0.,0.));
#23746=CARTESIAN_POINT('',(0.012,-0.00343283339125312,0.0103179228000551));
#23747=CARTESIAN_POINT('Origin',(0.012,0.00114726146149736,0.0107453934304013));
#23748=CARTESIAN_POINT('',(0.012,-0.0038486290688996,0.0101701489807191));
#23749=CARTESIAN_POINT('Origin',(0.012,0.,0.));
#23750=CARTESIAN_POINT('',(0.012,-0.00463639655948427,0.0110681446929105));
#23751=CARTESIAN_POINT('Origin',(0.012,-0.00767123192004028,0.00761130012968249));
#23752=CARTESIAN_POINT('',(0.012,-0.00492441115452898,0.0109430423000713));
#23753=CARTESIAN_POINT('Origin',(0.012,0.,0.));
#23754=CARTESIAN_POINT('',(0.012,-0.00480581676911598,0.0097543836905098));
#23755=CARTESIAN_POINT('Origin',(0.012,-0.000326588410304044,0.0108015290049791));
#23756=CARTESIAN_POINT('',(0.012,-0.00519761783757985,0.00955136874036762));
#23757=CARTESIAN_POINT('Origin',(0.012,0.,0.));
#23758=CARTESIAN_POINT('',(0.012,-0.00610032508627829,0.0103337328125767));
#23759=CARTESIAN_POINT('Origin',(0.012,-0.0086361868858939,0.00649584212454889));
#23760=CARTESIAN_POINT('',(0.012,-0.0063686223242156,0.0101705776478774));
#23761=CARTESIAN_POINT('Origin',(0.012,0.,0.));
#23762=CARTESIAN_POINT('',(0.012,-0.00608927687352473,0.00900913886881298));
#23763=CARTESIAN_POINT('Origin',(0.012,-0.00179435455795048,0.0106564525314718));
#23764=CARTESIAN_POINT('',(0.012,-0.0064497848202166,0.0087546645722668));
#23765=CARTESIAN_POINT('Origin',(0.012,0.,0.));
#23766=CARTESIAN_POINT('',(0.012,-0.00745061609897327,0.0094068230421179));
#23767=CARTESIAN_POINT('Origin',(0.012,-0.00944026603035641,0.00525937887124024));
#23768=CARTESIAN_POINT('',(0.012,-0.00769419810989828,0.00920865437757535));
#23769=CARTESIAN_POINT('Origin',(0.012,0.,0.));
#23770=CARTESIAN_POINT('',(0.012,-0.00725930527113401,0.00809607083593554));
#23771=CARTESIAN_POINT('Origin',(0.012,-0.00322869527523151,0.0103128665100857));
#23772=CARTESIAN_POINT('',(0.012,-0.00758180451511425,0.00779487756764615));
#23773=CARTESIAN_POINT('Origin',(0.012,0.,0.));
#23774=CARTESIAN_POINT('',(0.012,-0.00866211623085141,0.00830468195677719));
#23775=CARTESIAN_POINT('Origin',(0.012,-0.0100684908803427,0.00392494334068737));
#23776=CARTESIAN_POINT('',(0.012,-0.00887644554277545,0.00807519129966231));
#23777=CARTESIAN_POINT('Origin',(0.012,0.,0.));
#23778=CARTESIAN_POINT('',(0.012,-0.00829410654667511,0.00703218832173891));
#23779=CARTESIAN_POINT('Origin',(0.012,-0.00460289150846104,0.00977717129830948));
#23780=CARTESIAN_POINT('',(0.012,-0.00857258953722036,0.006689886742415));
#23781=CARTESIAN_POINT('Origin',(0.012,0.,0.));
#23782=CARTESIAN_POINT('',(0.012,-0.0097122575267021,0.0070478403596434));
#23783=CARTESIAN_POINT('Origin',(0.012,-0.0105091587955445,0.00251739354197548));
#23784=CARTESIAN_POINT('',(0.012,-0.00989334159007065,0.00679130268668526));
#23785=CARTESIAN_POINT('Origin',(0.012,0.,0.));
#23786=CARTESIAN_POINT('',(0.012,-0.0091744043103039,0.00583730944451955));
#23787=CARTESIAN_POINT('Origin',(0.012,-0.00589134458189312,0.00905934588436428));
#23788=CARTESIAN_POINT('',(0.012,-0.00940368343621036,0.00546027598492447));
#23789=CARTESIAN_POINT('Origin',(0.012,0.,0.));
#23790=CARTESIAN_POINT('',(0.012,-0.0105814778411273,0.00565971083163554));
#23791=CARTESIAN_POINT('Origin',(0.012,-0.0107540609664773,0.00106294946466809));
#23792=CARTESIAN_POINT('',(0.012,-0.010725943402464,0.0053809049542934));
#23793=CARTESIAN_POINT('Origin',(0.012,0.,0.));
#23794=CARTESIAN_POINT('',(0.012,-0.00988380028027131,0.00453369253696241));
#23795=CARTESIAN_POINT('Origin',(0.012,-0.00707005305261656,0.00817276199753406));
#23796=CARTESIAN_POINT('',(0.012,-0.0100596045052361,0.00412895061707371));
#23797=CARTESIAN_POINT('Origin',(0.012,0.,0.));
#23798=CARTESIAN_POINT('',(0.012,-0.0112535852442972,0.00416615159941843));
#23799=CARTESIAN_POINT('Origin',(0.012,-0.0107986353290695,-0.000411295349988447));
#23800=CARTESIAN_POINT('',(0.012,-0.0113587411835337,0.00387027114366622));
#23801=CARTESIAN_POINT('Origin',(0.012,0.,0.));
#23802=CARTESIAN_POINT('',(0.012,-0.0104090797518856,0.00314562151551737));
#23803=CARTESIAN_POINT('Origin',(0.012,-0.00811705981202384,0.00713393501814931));
#23804=CARTESIAN_POINT('',(0.012,-0.010528134175832,0.00272071071150145));
#23805=CARTESIAN_POINT('Origin',(0.012,0.,0.));
#23806=CARTESIAN_POINT('',(0.012,-0.0117160596469668,0.0025949848455657));
#23807=CARTESIAN_POINT('Origin',(0.012,-0.0106420515472837,-0.00187787851047538));
#23808=CARTESIAN_POINT('',(0.012,-0.0117799471079178,0.00228754150446676));
#23809=CARTESIAN_POINT('Origin',(0.012,0.,0.));
#23810=CARTESIAN_POINT('',(0.012,-0.0107404577624574,0.00169895351698271));
#23811=CARTESIAN_POINT('Origin',(0.012,-0.00901286110520009,0.00596221632729986));
#23812=CARTESIAN_POINT('',(0.012,-0.0108005446267269,0.00126178911315627));
#23813=CARTESIAN_POINT('Origin',(0.012,0.,0.));
#23814=CARTESIAN_POINT('',(0.012,-0.0119602860260496,0.000975478433939967));
#23815=CARTESIAN_POINT('Origin',(0.012,-0.0102872264807069,-0.00330948034739476));
#23816=CARTESIAN_POINT('',(0.012,-0.0119817149061973,0.000662199295233823));
#23817=CARTESIAN_POINT('Origin',(0.012,0.,0.));
#23818=CARTESIAN_POINT('',(0.012,-0.0108717613666412,0.000220637228970165));
#23819=CARTESIAN_POINT('Origin',(0.012,-0.00974076984897455,0.00467943282721932));
#23820=CARTESIAN_POINT('',(0.012,-0.0108717613666412,-0.000220637228970318));
#23821=CARTESIAN_POINT('Origin',(0.012,0.,0.));
#23822=CARTESIAN_POINT('',(0.012,-0.0119817149061973,-0.000662199295233991));
#23823=CARTESIAN_POINT('Origin',(0.012,-0.00974076984897448,-0.00467943282721946));
#23824=CARTESIAN_POINT('',(0.012,-0.0119602860260496,-0.000975478433940136));
#23825=CARTESIAN_POINT('Origin',(0.012,0.,0.));
#23826=CARTESIAN_POINT('',(0.012,-0.0108005446267269,-0.00126178911315643));
#23827=CARTESIAN_POINT('Origin',(0.012,-0.0102872264807069,0.00330948034739461));
#23828=CARTESIAN_POINT('',(0.012,-0.0107404577624574,-0.00169895351698286));
#23829=CARTESIAN_POINT('Origin',(0.012,0.,0.));
#23830=CARTESIAN_POINT('',(0.012,-0.0117799471079178,-0.00228754150446692));
#23831=CARTESIAN_POINT('Origin',(0.012,-0.0090128611052,-0.00596221632729998));
#23832=CARTESIAN_POINT('',(0.012,-0.0117160596469668,-0.00259498484556586));
#23833=CARTESIAN_POINT('Origin',(0.012,0.,0.));
#23834=CARTESIAN_POINT('',(0.012,-0.0105281341758319,-0.00272071071150159));
#23835=CARTESIAN_POINT('Origin',(0.012,-0.0106420515472838,0.00187787851047525));
#23836=CARTESIAN_POINT('',(0.012,-0.0104090797518855,-0.00314562151551751));
#23837=CARTESIAN_POINT('Origin',(0.012,0.,0.));
#23838=CARTESIAN_POINT('',(0.012,-0.0113587411835336,-0.00387027114366637));
#23839=CARTESIAN_POINT('Origin',(0.012,-0.00811705981202375,-0.00713393501814942));
#23840=CARTESIAN_POINT('',(0.012,-0.0112535852442971,-0.00416615159941858));
#23841=CARTESIAN_POINT('Origin',(0.012,0.,0.));
#23842=CARTESIAN_POINT('',(0.012,-0.010059604505236,-0.00412895061707385));
#23843=CARTESIAN_POINT('Origin',(0.012,-0.0107986353290695,0.0004112953499883));
#23844=CARTESIAN_POINT('',(0.012,-0.00988380028027125,-0.00453369253696255));
#23845=CARTESIAN_POINT('Origin',(0.012,0.,0.));
#23846=CARTESIAN_POINT('',(0.012,-0.0107259434024639,-0.00538090495429355));
#23847=CARTESIAN_POINT('Origin',(0.012,-0.00707005305261645,-0.00817276199753415));
#23848=CARTESIAN_POINT('',(0.012,-0.0105814778411272,-0.00565971083163568));
#23849=CARTESIAN_POINT('Origin',(0.012,0.,0.));
#23850=CARTESIAN_POINT('',(0.012,-0.00940368343621029,-0.0054602759849246));
#23851=CARTESIAN_POINT('Origin',(0.012,-0.0107540609664773,-0.00106294946466824));
#23852=CARTESIAN_POINT('',(0.012,-0.00917440431030382,-0.00583730944451968));
#23853=CARTESIAN_POINT('Origin',(0.012,0.,0.));
#23854=CARTESIAN_POINT('',(0.012,-0.00989334159007055,-0.00679130268668539));
#23855=CARTESIAN_POINT('Origin',(0.012,-0.00589134458189299,-0.00905934588436437));
#23856=CARTESIAN_POINT('',(0.012,-0.009712257526702,-0.00704784035964354));
#23857=CARTESIAN_POINT('Origin',(0.012,0.,0.));
#23858=CARTESIAN_POINT('',(0.012,-0.00857258953722027,-0.00668988674241512));
#23859=CARTESIAN_POINT('Origin',(0.012,-0.0105091587955444,-0.00251739354197563));
#23860=CARTESIAN_POINT('',(0.012,-0.00829410654667501,-0.00703218832173902));
#23861=CARTESIAN_POINT('Origin',(0.012,0.,0.));
#23862=CARTESIAN_POINT('',(0.012,-0.00887644554277533,-0.00807519129966243));
#23863=CARTESIAN_POINT('Origin',(0.012,-0.0046028915084609,-0.00977717129830955));
#23864=CARTESIAN_POINT('',(0.012,-0.00866211623085129,-0.00830468195677731));
#23865=CARTESIAN_POINT('Origin',(0.012,0.,0.));
#23866=CARTESIAN_POINT('',(0.012,-0.00758180451511414,-0.00779487756764626));
#23867=CARTESIAN_POINT('Origin',(0.012,-0.0100684908803426,-0.00392494334068751));
#23868=CARTESIAN_POINT('',(0.012,-0.0072593052711339,-0.00809607083593564));
#23869=CARTESIAN_POINT('Origin',(0.012,0.,0.));
#23870=CARTESIAN_POINT('',(0.012,-0.00769419810989815,-0.00920865437757546));
#23871=CARTESIAN_POINT('Origin',(0.012,-0.00322869527523136,-0.0103128665100857));
#23872=CARTESIAN_POINT('',(0.012,-0.00745061609897314,-0.009406823042118));
#23873=CARTESIAN_POINT('Origin',(0.012,0.,0.));
#23874=CARTESIAN_POINT('',(0.012,-0.00644978482021648,-0.00875466457226689));
#23875=CARTESIAN_POINT('Origin',(0.012,-0.00944026603035634,-0.00525937887124037));
#23876=CARTESIAN_POINT('',(0.012,-0.0060892768735246,-0.00900913886881307));
#23877=CARTESIAN_POINT('Origin',(0.012,0.,0.));
#23878=CARTESIAN_POINT('',(0.012,-0.00636862232421547,-0.0101705776478774));
#23879=CARTESIAN_POINT('Origin',(0.012,-0.00179435455795034,-0.0106564525314718));
#23880=CARTESIAN_POINT('',(0.012,-0.00610032508627815,-0.0103337328125767));
#23881=CARTESIAN_POINT('Origin',(0.012,0.,0.));
#23882=CARTESIAN_POINT('',(0.012,-0.00519761783757972,-0.00955136874036769));
#23883=CARTESIAN_POINT('Origin',(0.012,-0.00863618688589381,-0.00649584212454901));
#23884=CARTESIAN_POINT('',(0.012,-0.00480581676911584,-0.00975438369050987));
#23885=CARTESIAN_POINT('Origin',(0.012,0.,0.));
#23886=CARTESIAN_POINT('',(0.012,-0.00492441115452883,-0.0109430423000714));
#23887=CARTESIAN_POINT('Origin',(0.012,-0.000326588410303897,-0.0108015290049791));
#23888=CARTESIAN_POINT('',(0.012,-0.00463639655948412,-0.0110681446929105));
#23889=CARTESIAN_POINT('Origin',(0.012,0.,0.));
#23890=CARTESIAN_POINT('',(0.012,-0.00384862906889946,-0.0101701489807191));
#23891=CARTESIAN_POINT('Origin',(0.012,-0.00767123192004017,-0.00761130012968259));
#23892=CARTESIAN_POINT('',(0.012,-0.00343283339125298,-0.0103179228000552));
#23893=CARTESIAN_POINT('Origin',(0.012,0.,0.));
#23894=CARTESIAN_POINT('',(0.012,-0.00338846752237705,-0.0115116587792462));
#23895=CARTESIAN_POINT('Origin',(0.012,0.0011472614614975,-0.0107453934304013));
#23896=CARTESIAN_POINT('',(0.012,-0.00308610073718608,-0.0115963779793494));
#23897=CARTESIAN_POINT('Origin',(0.012,0.,0.));
#23898=CARTESIAN_POINT('',(0.012,-0.00242794762255145,-0.0105994785882206));
#23899=CARTESIAN_POINT('Origin',(0.012,-0.00656337641804439,-0.00858497401453309));
#23900=CARTESIAN_POINT('',(0.012,-0.00199590282248128,-0.0106892585300951));
#23901=CARTESIAN_POINT('Origin',(0.012,0.,0.));
#23902=CARTESIAN_POINT('',(0.012,-0.00178940315151014,-0.0118658348362585));
#23903=CARTESIAN_POINT('Origin',(0.012,0.00259974002297325,-0.0104890915072803));
#23904=CARTESIAN_POINT('',(0.012,-0.00147831669728109,-0.0119085926852227));
#23905=CARTESIAN_POINT('Origin',(0.012,0.,0.));
#23906=CARTESIAN_POINT('',(0.012,-0.00096203810584863,-0.0108313599646072));
#23907=CARTESIAN_POINT('Origin',(0.012,-0.00533325763176552,-0.00939872607688746));
#23908=CARTESIAN_POINT('',(0.012,-0.000521792360519925,-0.0108614735985732));
#23909=CARTESIAN_POINT('Origin',(0.012,0.,0.));
#23910=CARTESIAN_POINT('',(0.012,-0.000157005585611382,-0.011998972841293));
#23911=CARTESIAN_POINT('Origin',(0.012,0.00400379034671803,-0.010037397655502));
#23912=CARTESIAN_POINT('',(0.012,0.000157005585611632,-0.011998972841293));
#23913=CARTESIAN_POINT('Origin',(0.012,0.,0.));
#23914=CARTESIAN_POINT('',(0.012,0.000521792360520154,-0.0108614735985732));
#23915=CARTESIAN_POINT('Origin',(0.012,-0.00400379034671782,-0.0100373976555021));
#23916=CARTESIAN_POINT('',(0.012,0.000962038105848858,-0.0108313599646072));
#23917=CARTESIAN_POINT('Origin',(0.012,0.,0.));
#23918=CARTESIAN_POINT('',(0.012,0.00147831669728134,-0.0119085926852227));
#23919=CARTESIAN_POINT('Origin',(0.012,0.00533325763176572,-0.00939872607688735));
#23920=CARTESIAN_POINT('',(0.012,0.00178940315151039,-0.0118658348362584));
#23921=CARTESIAN_POINT('Origin',(0.012,0.,0.));
#23922=CARTESIAN_POINT('',(0.012,0.00199590282248151,-0.0106892585300951));
#23923=CARTESIAN_POINT('Origin',(0.012,-0.00259974002297304,-0.0104890915072804));
#23924=CARTESIAN_POINT('',(0.012,0.00242794762255167,-0.0105994785882205));
#23925=CARTESIAN_POINT('Origin',(0.012,0.,0.));
#23926=CARTESIAN_POINT('',(0.012,0.00308610073718632,-0.0115963779793493));
#23927=CARTESIAN_POINT('Origin',(0.012,0.00656337641804457,-0.00858497401453295));
#23928=CARTESIAN_POINT('',(0.012,0.00338846752237729,-0.0115116587792461));
#23929=CARTESIAN_POINT('Origin',(0.012,0.,0.));
#23930=CARTESIAN_POINT('',(0.012,0.00343283339125319,-0.0103179228000551));
#23931=CARTESIAN_POINT('Origin',(0.012,-0.00114726146149728,-0.0107453934304014));
#23932=CARTESIAN_POINT('',(0.012,0.00384862906889967,-0.010170148980719));
#23933=CARTESIAN_POINT('Origin',(0.012,0.,0.));
#23934=CARTESIAN_POINT('',(0.012,0.00463639655948435,-0.0110681446929104));
#23935=CARTESIAN_POINT('Origin',(0.012,0.00767123192004033,-0.00761130012968243));
#23936=CARTESIAN_POINT('',(0.012,0.00492441115452905,-0.0109430423000713));
#23937=CARTESIAN_POINT('Origin',(0.012,0.,0.));
#23938=CARTESIAN_POINT('',(0.012,0.00480581676911604,-0.00975438369050977));
#23939=CARTESIAN_POINT('Origin',(0.012,0.000326588410304114,-0.0108015290049791));
#23940=CARTESIAN_POINT('',(0.012,0.00519761783757991,-0.00955136874036759));
#23941=CARTESIAN_POINT('Origin',(0.012,0.,0.));
#23942=CARTESIAN_POINT('',(0.012,0.00610032508627836,-0.0103337328125766));
#23943=CARTESIAN_POINT('Origin',(0.012,0.00863618688589394,-0.00649584212454884));
#23944=CARTESIAN_POINT('',(0.012,0.00636862232421567,-0.0101705776478773));
#23945=CARTESIAN_POINT('Origin',(0.012,0.,0.));
#23946=CARTESIAN_POINT('',(0.012,0.00608927687352478,-0.00900913886881295));
#23947=CARTESIAN_POINT('Origin',(0.012,0.00179435455795055,-0.0106564525314718));
#23948=CARTESIAN_POINT('',(0.012,0.00644978482021666,-0.00875466457226676));
#23949=CARTESIAN_POINT('Origin',(0.012,0.,0.));
#23950=CARTESIAN_POINT('',(0.012,0.00745061609897333,-0.00940682304211785));
#23951=CARTESIAN_POINT('Origin',(0.012,0.00944026603035645,-0.00525937887124018));
#23952=CARTESIAN_POINT('',(0.012,0.00769419810989834,-0.0092086543775753));
#23953=CARTESIAN_POINT('Origin',(0.012,0.,0.));
#23954=CARTESIAN_POINT('',(0.012,0.00725930527113406,-0.00809607083593549));
#23955=CARTESIAN_POINT('Origin',(0.012,0.00322869527523158,-0.0103128665100857));
#23956=CARTESIAN_POINT('',(0.012,0.0075818045151143,-0.0077948775676461));
#23957=CARTESIAN_POINT('Origin',(0.012,0.,0.));
#23958=CARTESIAN_POINT('',(0.012,0.00866211623085146,-0.00830468195677713));
#23959=CARTESIAN_POINT('Origin',(0.012,0.0100684908803427,-0.0039249433406873));
#23960=CARTESIAN_POINT('',(0.012,0.0088764455427755,-0.00807519129966225));
#23961=CARTESIAN_POINT('Origin',(0.012,0.,0.));
#23962=CARTESIAN_POINT('',(0.012,0.00829410654667516,-0.00703218832173885));
#23963=CARTESIAN_POINT('Origin',(0.012,0.0046028915084611,-0.00977717129830945));
#23964=CARTESIAN_POINT('',(0.012,0.00857258953722041,-0.00668988674241494));
#23965=CARTESIAN_POINT('Origin',(0.012,0.,0.));
#23966=CARTESIAN_POINT('',(0.012,0.00971225752670214,-0.00704784035964334));
#23967=CARTESIAN_POINT('Origin',(0.012,0.0105091587955445,-0.00251739354197541));
#23968=CARTESIAN_POINT('',(0.012,0.00989334159007069,-0.00679130268668519));
#23969=CARTESIAN_POINT('Origin',(0.012,0.,0.));
#23970=CARTESIAN_POINT('',(0.012,0.00917440431030394,-0.00583730944451949));
#23971=CARTESIAN_POINT('Origin',(0.012,0.00589134458189318,-0.00905934588436424));
#23972=CARTESIAN_POINT('',(0.012,0.0094036834362104,-0.0054602759849244));
#23973=CARTESIAN_POINT('Origin',(0.012,0.,0.));
#23974=CARTESIAN_POINT('',(0.012,0.0105814778411273,-0.00565971083163546));
#23975=CARTESIAN_POINT('Origin',(0.012,0.0107540609664773,-0.00106294946466802));
#23976=CARTESIAN_POINT('',(0.012,0.010725943402464,-0.00538090495429333));
#23977=CARTESIAN_POINT('Origin',(0.012,0.,0.));
#23978=CARTESIAN_POINT('',(0.012,0.00988380028027134,-0.00453369253696235));
#23979=CARTESIAN_POINT('Origin',(0.012,0.00707005305261661,-0.00817276199753401));
#23980=CARTESIAN_POINT('',(0.012,0.0100596045052361,-0.00412895061707364));
#23981=CARTESIAN_POINT('Origin',(0.012,0.,0.));
#23982=CARTESIAN_POINT('',(0.012,0.0112535852442972,-0.00416615159941835));
#23983=CARTESIAN_POINT('Origin',(0.012,0.0107986353290695,0.000411295349988523));
#23984=CARTESIAN_POINT('',(0.012,0.0113587411835337,-0.00387027114366614));
#23985=CARTESIAN_POINT('Origin',(0.012,0.,0.));
#23986=CARTESIAN_POINT('',(0.012,0.0104090797518856,-0.0031456215155173));
#23987=CARTESIAN_POINT('Origin',(0.012,0.00811705981202389,-0.00713393501814925));
#23988=CARTESIAN_POINT('',(0.012,0.010528134175832,-0.00272071071150138));
#23989=CARTESIAN_POINT('Origin',(0.012,0.,0.));
#23990=CARTESIAN_POINT('',(0.012,0.0117160596469668,-0.00259498484556562));
#23991=CARTESIAN_POINT('Origin',(0.012,0.0106420515472837,0.00187787851047546));
#23992=CARTESIAN_POINT('',(0.012,0.0117799471079179,-0.00228754150446667));
#23993=CARTESIAN_POINT('Origin',(0.012,0.,0.));
#23994=CARTESIAN_POINT('',(0.012,0.0107404577624574,-0.00169895351698263));
#23995=CARTESIAN_POINT('Origin',(0.012,0.00901286110520013,-0.00596221632729979));
#23996=CARTESIAN_POINT('',(0.012,0.0108005446267269,-0.0012617891131562));
#23997=CARTESIAN_POINT('Origin',(0.012,0.,0.));
#23998=CARTESIAN_POINT('',(0.012,0.0119602860260496,-0.000975478433939885));
#23999=CARTESIAN_POINT('Origin',(0.012,0.0102872264807069,0.00330948034739484));
#24000=CARTESIAN_POINT('',(0.012,0.0119817149061973,-0.000662199295233908));
#24001=CARTESIAN_POINT('Origin',(0.012,0.,0.));
#24002=CARTESIAN_POINT('',(0.012,0.0108717613666412,-0.000220637228970241));
#24003=CARTESIAN_POINT('Origin',(0.012,0.00974076984897452,-0.00467943282721939));
#24004=CARTESIAN_POINT('',(0.012,0.0108717613666412,0.000220637228970242));
#24005=CARTESIAN_POINT('Origin',(0.012,0.,0.));
#24006=CARTESIAN_POINT('',(0.012,0.0119817149061973,0.000662199295233908));
#24007=CARTESIAN_POINT('Origin',(0.012,0.00974076984897452,0.00467943282721939));
#24008=CARTESIAN_POINT('',(0.012,0.0119602860260496,0.00097547843394005));
#24009=CARTESIAN_POINT('Origin',(0.012,0.,0.));
#24010=CARTESIAN_POINT('',(0.012,0.0108005446267269,0.00126178911315635));
#24011=CARTESIAN_POINT('Origin',(0.012,0.0102872264807069,-0.00330948034739469));
#24012=CARTESIAN_POINT('',(0.012,0.0107404577624574,0.00169895351698278));
#24013=CARTESIAN_POINT('Origin',(0.012,0.,0.));
#24014=CARTESIAN_POINT('',(0.012,0.0117799471079178,0.00228754150446684));
#24015=CARTESIAN_POINT('Origin',(0.012,0.00901286110520005,0.00596221632729992));
#24016=CARTESIAN_POINT('',(0.012,0.0117160596469668,0.00259498484556578));
#24017=CARTESIAN_POINT('Origin',(0.012,0.,0.));
#24018=CARTESIAN_POINT('',(0.012,0.010528134175832,0.00272071071150152));
#24019=CARTESIAN_POINT('Origin',(0.012,0.0106420515472837,-0.00187787851047532));
#24020=CARTESIAN_POINT('',(0.012,0.0104090797518855,0.00314562151551744));
#24021=CARTESIAN_POINT('Origin',(0.012,0.,0.));
#24022=CARTESIAN_POINT('',(0.012,0.0113587411835337,0.0038702711436663));
#24023=CARTESIAN_POINT('Origin',(0.012,0.00811705981202379,0.00713393501814937));
#24024=CARTESIAN_POINT('',(0.012,0.0112535852442971,0.00416615159941851));
#24025=CARTESIAN_POINT('Origin',(0.012,0.,0.));
#24026=CARTESIAN_POINT('',(0.012,0.0100596045052361,0.00412895061707378));
#24027=CARTESIAN_POINT('Origin',(0.012,0.0107986353290695,-0.000411295349988374));
#24028=CARTESIAN_POINT('',(0.012,0.00988380028027128,0.00453369253696249));
#24029=CARTESIAN_POINT('Origin',(0.012,0.,0.));
#24030=CARTESIAN_POINT('',(0.012,0.0107259434024639,0.00538090495429348));
#24031=CARTESIAN_POINT('Origin',(0.012,0.0070700530526165,0.00817276199753411));
#24032=CARTESIAN_POINT('',(0.012,0.0105814778411272,0.00565971083163561));
#24033=CARTESIAN_POINT('Origin',(0.012,0.,0.));
#24034=CARTESIAN_POINT('',(0.012,0.00940368343621032,0.00546027598492453));
#24035=CARTESIAN_POINT('Origin',(0.012,0.0107540609664773,0.00106294946466816));
#24036=CARTESIAN_POINT('',(0.012,0.00917440431030386,0.00583730944451961));
#24037=CARTESIAN_POINT('Origin',(0.012,0.,0.));
#24038=CARTESIAN_POINT('',(0.012,0.0098933415900706,0.00679130268668532));
#24039=CARTESIAN_POINT('Origin',(0.012,0.00589134458189306,0.00905934588436432));
#24040=CARTESIAN_POINT('',(0.012,0.00971225752670205,0.00704784035964347));
#24041=CARTESIAN_POINT('Origin',(0.012,0.,0.));
#24042=CARTESIAN_POINT('',(0.012,0.00857258953722032,0.00668988674241506));
#24043=CARTESIAN_POINT('Origin',(0.012,0.0105091587955444,0.00251739354197556));
#24044=CARTESIAN_POINT('',(0.012,0.00829410654667506,0.00703218832173896));
#24045=CARTESIAN_POINT('Origin',(0.012,0.,0.));
#24046=CARTESIAN_POINT('',(0.012,0.00887644554277539,0.00807519129966237));
#24047=CARTESIAN_POINT('Origin',(0.012,0.00460289150846097,0.00977717129830952));
#24048=CARTESIAN_POINT('',(0.012,0.00866211623085135,0.00830468195677725));
#24049=CARTESIAN_POINT('Origin',(0.012,0.,0.));
#24050=CARTESIAN_POINT('',(0.012,0.00758180451511419,0.00779487756764621));
#24051=CARTESIAN_POINT('Origin',(0.012,0.0100684908803426,0.00392494334068744));
#24052=CARTESIAN_POINT('',(0.012,0.00725930527113395,0.00809607083593559));
#24053=CARTESIAN_POINT('Origin',(0.012,0.,0.));
#24054=CARTESIAN_POINT('',(0.012,0.00769419810989822,0.00920865437757541));
#24055=CARTESIAN_POINT('Origin',(0.012,0.00322869527523144,0.0103128665100857));
#24056=CARTESIAN_POINT('',(0.012,0.00745061609897321,0.00940682304211795));
#24057=CARTESIAN_POINT('Origin',(0.012,0.,0.));
#24058=CARTESIAN_POINT('',(0.012,0.00644978482021654,0.00875466457226685));
#24059=CARTESIAN_POINT('Origin',(0.012,0.00944026603035638,0.00525937887124031));
#24060=CARTESIAN_POINT('',(0.012,0.00608927687352466,0.00900913886881303));
#24061=CARTESIAN_POINT('Origin',(0.012,0.,0.));
#24062=CARTESIAN_POINT('',(0.012,0.00636862232421553,0.0101705776478774));
#24063=CARTESIAN_POINT('Origin',(0.012,0.00179435455795041,0.0106564525314718));
#24064=CARTESIAN_POINT('',(0.012,0.00610032508627822,0.0103337328125767));
#24065=CARTESIAN_POINT('Origin',(0.012,0.,0.));
#24066=CARTESIAN_POINT('',(0.012,0.00519761783757978,0.00955136874036766));
#24067=CARTESIAN_POINT('Origin',(0.012,0.00863618688589385,0.00649584212454895));
#24068=CARTESIAN_POINT('',(0.012,0.00480581676911591,0.00975438369050984));
#24069=CARTESIAN_POINT('Origin',(0.012,0.,0.));
#24070=CARTESIAN_POINT('',(0.012,0.00492441115452891,0.0109430423000714));
#24071=CARTESIAN_POINT('Origin',(0.012,0.00032658841030397,0.0108015290049791));
#24072=CARTESIAN_POINT('',(0.012,0.00463639655948419,0.0110681446929105));
#24073=CARTESIAN_POINT('Origin',(0.012,0.,0.));
#24074=CARTESIAN_POINT('',(0.012,0.00384862906889953,0.0101701489807191));
#24075=CARTESIAN_POINT('Origin',(0.012,0.00767123192004022,0.00761130012968254));
#24076=CARTESIAN_POINT('',(0.012,0.00343283339125305,0.0103179228000552));
#24077=CARTESIAN_POINT('Origin',(0.012,0.,0.));
#24078=CARTESIAN_POINT('',(0.012,0.00338846752237713,0.0115116587792462));
#24079=CARTESIAN_POINT('Origin',(0.012,-0.00114726146149743,0.0107453934304013));
#24080=CARTESIAN_POINT('',(0.012,0.00308610073718616,0.0115963779793494));
#24081=CARTESIAN_POINT('Origin',(0.012,0.,0.));
#24082=CARTESIAN_POINT('',(0.012,0.00242794762255152,0.0105994785882206));
#24083=CARTESIAN_POINT('Origin',(0.012,0.00656337641804445,0.00858497401453304));
#24084=CARTESIAN_POINT('',(0.012,0.00199590282248136,0.0106892585300951));
#24085=CARTESIAN_POINT('Origin',(0.012,0.,0.));
#24086=CARTESIAN_POINT('',(0.012,0.00178940315151022,0.0118658348362585));
#24087=CARTESIAN_POINT('Origin',(0.012,-0.00259974002297318,0.0104890915072804));
#24088=CARTESIAN_POINT('',(0.012,0.00147831669728117,0.0119085926852227));
#24089=CARTESIAN_POINT('Origin',(0.012,0.,0.));
#24090=CARTESIAN_POINT('',(0.012,0.000962038105848705,0.0108313599646072));
#24091=CARTESIAN_POINT('Origin',(0.012,0.00533325763176559,0.00939872607688742));
#24092=CARTESIAN_POINT('',(0.012,0.000521792360520001,0.0108614735985732));
#24093=CARTESIAN_POINT('Origin',(0.012,0.,0.));
#24094=CARTESIAN_POINT('',(0.012,0.000157005585611465,0.011998972841293));
#24095=CARTESIAN_POINT('Origin',(0.012,-0.00400379034671796,0.010037397655502));
#24096=CARTESIAN_POINT('Origin',(0.012,0.,0.));
#24097=CARTESIAN_POINT('',(0.012,-1.10218211923262E-18,-0.009));
#24098=CARTESIAN_POINT('Origin',(0.012,0.,0.));
#24099=CARTESIAN_POINT('Origin',(-0.01,0.,0.));
#24100=CARTESIAN_POINT('',(0.,-0.000157005585611549,0.011998972841293));
#24101=CARTESIAN_POINT('',(0.006,-0.000157005585611549,0.011998972841293));
#24102=CARTESIAN_POINT('',(0.,0.000157005585611465,0.011998972841293));
#24103=CARTESIAN_POINT('',(0.006,0.000157005585611465,0.011998972841293));
#24104=CARTESIAN_POINT('Origin',(0.,0.,0.));
#24105=CARTESIAN_POINT('Origin',(-0.01,0.,0.));
#24106=CARTESIAN_POINT('',(0.,-0.00147831669728126,0.0119085926852227));
#24107=CARTESIAN_POINT('',(0.006,-0.00147831669728126,0.0119085926852227));
#24108=CARTESIAN_POINT('',(0.,-0.0017894031515103,0.0118658348362585));
#24109=CARTESIAN_POINT('Origin',(0.,0.,0.));
#24110=CARTESIAN_POINT('',(0.006,-0.0017894031515103,0.0118658348362585));
#24111=CARTESIAN_POINT('Origin',(-0.01,0.,0.));
#24112=CARTESIAN_POINT('',(0.,0.00147831669728117,0.0119085926852227));
#24113=CARTESIAN_POINT('',(0.006,0.00147831669728117,0.0119085926852227));
#24114=CARTESIAN_POINT('',(0.,0.00178940315151022,0.0118658348362585));
#24115=CARTESIAN_POINT('',(0.006,0.00178940315151022,0.0118658348362585));
#24116=CARTESIAN_POINT('Origin',(0.,0.,0.));
#24117=CARTESIAN_POINT('Origin',(-0.01,0.,0.));
#24118=CARTESIAN_POINT('',(0.,0.00308610073718616,0.0115963779793494));
#24119=CARTESIAN_POINT('',(0.006,0.00308610073718616,0.0115963779793494));
#24120=CARTESIAN_POINT('',(0.,0.00338846752237713,0.0115116587792462));
#24121=CARTESIAN_POINT('',(0.006,0.00338846752237713,0.0115116587792462));
#24122=CARTESIAN_POINT('Origin',(0.,0.,0.));
#24123=CARTESIAN_POINT('Origin',(-0.01,0.,0.));
#24124=CARTESIAN_POINT('',(0.,0.00745061609897321,0.00940682304211795));
#24125=CARTESIAN_POINT('',(0.006,0.00745061609897321,0.00940682304211795));
#24126=CARTESIAN_POINT('',(0.,0.00769419810989822,0.00920865437757541));
#24127=CARTESIAN_POINT('',(0.006,0.00769419810989822,0.00920865437757541));
#24128=CARTESIAN_POINT('Origin',(0.,0.,0.));
#24129=CARTESIAN_POINT('Origin',(-0.01,0.,0.));
#24130=CARTESIAN_POINT('',(0.,0.00636862232421553,0.0101705776478774));
#24131=CARTESIAN_POINT('',(0.006,0.00636862232421553,0.0101705776478774));
#24132=CARTESIAN_POINT('',(0.,0.00610032508627822,0.0103337328125767));
#24133=CARTESIAN_POINT('Origin',(0.,0.,0.));
#24134=CARTESIAN_POINT('',(0.006,0.00610032508627822,0.0103337328125767));
#24135=CARTESIAN_POINT('Origin',(-0.01,0.,0.));
#24136=CARTESIAN_POINT('',(0.,0.00492441115452891,0.0109430423000714));
#24137=CARTESIAN_POINT('',(0.006,0.00492441115452891,0.0109430423000714));
#24138=CARTESIAN_POINT('',(0.,0.00463639655948419,0.0110681446929105));
#24139=CARTESIAN_POINT('Origin',(0.,0.,0.));
#24140=CARTESIAN_POINT('',(0.006,0.00463639655948419,0.0110681446929105));
#24141=CARTESIAN_POINT('Origin',(-0.01,0.,0.));
#24142=CARTESIAN_POINT('',(0.,0.0105814778411272,0.00565971083163561));
#24143=CARTESIAN_POINT('',(0.006,0.0105814778411272,0.00565971083163561));
#24144=CARTESIAN_POINT('',(0.,0.0107259434024639,0.00538090495429348));
#24145=CARTESIAN_POINT('',(0.006,0.0107259434024639,0.00538090495429348));
#24146=CARTESIAN_POINT('Origin',(0.,0.,0.));
#24147=CARTESIAN_POINT('Origin',(-0.01,0.,0.));
#24148=CARTESIAN_POINT('',(0.,0.0098933415900706,0.00679130268668532));
#24149=CARTESIAN_POINT('',(0.006,0.0098933415900706,0.00679130268668532));
#24150=CARTESIAN_POINT('',(0.,0.00971225752670205,0.00704784035964347));
#24151=CARTESIAN_POINT('Origin',(0.,0.,0.));
#24152=CARTESIAN_POINT('',(0.006,0.00971225752670205,0.00704784035964347));
#24153=CARTESIAN_POINT('Origin',(-0.01,0.,0.));
#24154=CARTESIAN_POINT('',(0.,0.00866211623085135,0.00830468195677725));
#24155=CARTESIAN_POINT('',(0.006,0.00866211623085135,0.00830468195677725));
#24156=CARTESIAN_POINT('',(0.,0.00887644554277539,0.00807519129966237));
#24157=CARTESIAN_POINT('',(0.006,0.00887644554277539,0.00807519129966237));
#24158=CARTESIAN_POINT('Origin',(0.,0.,0.));
#24159=CARTESIAN_POINT('Origin',(-0.01,0.,0.));
#24160=CARTESIAN_POINT('',(0.,0.0112535852442971,0.00416615159941851));
#24161=CARTESIAN_POINT('',(0.006,0.0112535852442971,0.00416615159941851));
#24162=CARTESIAN_POINT('',(0.,0.0113587411835337,0.0038702711436663));
#24163=CARTESIAN_POINT('',(0.006,0.0113587411835337,0.0038702711436663));
#24164=CARTESIAN_POINT('Origin',(0.,0.,0.));
#24165=CARTESIAN_POINT('Origin',(-0.01,0.,0.));
#24166=CARTESIAN_POINT('',(0.,0.0117160596469668,0.00259498484556578));
#24167=CARTESIAN_POINT('',(0.006,0.0117160596469668,0.00259498484556578));
#24168=CARTESIAN_POINT('',(0.,0.0117799471079178,0.00228754150446684));
#24169=CARTESIAN_POINT('',(0.006,0.0117799471079178,0.00228754150446684));
#24170=CARTESIAN_POINT('Origin',(0.,0.,0.));
#24171=CARTESIAN_POINT('Origin',(-0.01,0.,0.));
#24172=CARTESIAN_POINT('',(0.,-0.0119817149061973,0.000662199295233824));
#24173=CARTESIAN_POINT('',(0.006,-0.0119817149061973,0.000662199295233823));
#24174=CARTESIAN_POINT('',(0.,-0.0119602860260496,0.000975478433939967));
#24175=CARTESIAN_POINT('',(0.006,-0.0119602860260496,0.000975478433939967));
#24176=CARTESIAN_POINT('Origin',(0.,0.,0.));
#24177=CARTESIAN_POINT('Origin',(-0.01,0.,0.));
#24178=CARTESIAN_POINT('',(0.,-0.0119817149061973,-0.000662199295233991));
#24179=CARTESIAN_POINT('',(0.006,-0.0119817149061973,-0.000662199295233991));
#24180=CARTESIAN_POINT('',(0.,-0.0119602860260496,-0.000975478433940136));
#24181=CARTESIAN_POINT('Origin',(0.,0.,0.));
#24182=CARTESIAN_POINT('',(0.006,-0.0119602860260496,-0.000975478433940136));
#24183=CARTESIAN_POINT('Origin',(-0.01,0.,0.));
#24184=CARTESIAN_POINT('',(0.,-0.0117799471079178,0.00228754150446675));
#24185=CARTESIAN_POINT('',(0.006,-0.0117799471079178,0.00228754150446675));
#24186=CARTESIAN_POINT('',(0.,-0.0117160596469668,0.0025949848455657));
#24187=CARTESIAN_POINT('',(0.006,-0.0117160596469668,0.0025949848455657));
#24188=CARTESIAN_POINT('Origin',(0.,0.,0.));
#24189=CARTESIAN_POINT('Origin',(-0.01,0.,0.));
#24190=CARTESIAN_POINT('',(0.,-0.0113587411835337,0.00387027114366622));
#24191=CARTESIAN_POINT('',(0.006,-0.0113587411835337,0.00387027114366622));
#24192=CARTESIAN_POINT('',(0.,-0.0112535852442972,0.00416615159941843));
#24193=CARTESIAN_POINT('',(0.006,-0.0112535852442972,0.00416615159941843));
#24194=CARTESIAN_POINT('Origin',(0.,0.,0.));
#24195=CARTESIAN_POINT('Origin',(-0.01,0.,0.));
#24196=CARTESIAN_POINT('',(0.,-0.00887644554277545,0.00807519129966231));
#24197=CARTESIAN_POINT('',(0.006,-0.00887644554277545,0.00807519129966231));
#24198=CARTESIAN_POINT('',(0.,-0.00866211623085141,0.00830468195677719));
#24199=CARTESIAN_POINT('',(0.006,-0.00866211623085141,0.00830468195677719));
#24200=CARTESIAN_POINT('Origin',(0.,0.,0.));
#24201=CARTESIAN_POINT('Origin',(-0.01,0.,0.));
#24202=CARTESIAN_POINT('',(0.,-0.0097122575267021,0.0070478403596434));
#24203=CARTESIAN_POINT('',(0.006,-0.0097122575267021,0.0070478403596434));
#24204=CARTESIAN_POINT('',(0.,-0.00989334159007065,0.00679130268668526));
#24205=CARTESIAN_POINT('Origin',(0.,0.,0.));
#24206=CARTESIAN_POINT('',(0.006,-0.00989334159007065,0.00679130268668526));
#24207=CARTESIAN_POINT('Origin',(-0.01,0.,0.));
#24208=CARTESIAN_POINT('',(0.,-0.0105814778411273,0.00565971083163554));
#24209=CARTESIAN_POINT('',(0.006,-0.0105814778411273,0.00565971083163554));
#24210=CARTESIAN_POINT('',(0.,-0.010725943402464,0.0053809049542934));
#24211=CARTESIAN_POINT('Origin',(0.,0.,0.));
#24212=CARTESIAN_POINT('',(0.006,-0.010725943402464,0.0053809049542934));
#24213=CARTESIAN_POINT('Origin',(-0.01,0.,0.));
#24214=CARTESIAN_POINT('',(0.,-0.00492441115452898,0.0109430423000713));
#24215=CARTESIAN_POINT('',(0.006,-0.00492441115452898,0.0109430423000713));
#24216=CARTESIAN_POINT('',(0.,-0.00463639655948427,0.0110681446929105));
#24217=CARTESIAN_POINT('',(0.006,-0.00463639655948427,0.0110681446929105));
#24218=CARTESIAN_POINT('Origin',(0.,0.,0.));
#24219=CARTESIAN_POINT('Origin',(-0.01,0.,0.));
#24220=CARTESIAN_POINT('',(0.,-0.00610032508627829,0.0103337328125767));
#24221=CARTESIAN_POINT('',(0.006,-0.00610032508627829,0.0103337328125767));
#24222=CARTESIAN_POINT('',(0.,-0.0063686223242156,0.0101705776478774));
#24223=CARTESIAN_POINT('Origin',(0.,0.,0.));
#24224=CARTESIAN_POINT('',(0.006,-0.0063686223242156,0.0101705776478774));
#24225=CARTESIAN_POINT('Origin',(-0.01,0.,0.));
#24226=CARTESIAN_POINT('',(0.,-0.00769419810989828,0.00920865437757535));
#24227=CARTESIAN_POINT('',(0.006,-0.00769419810989828,0.00920865437757535));
#24228=CARTESIAN_POINT('',(0.,-0.00745061609897327,0.0094068230421179));
#24229=CARTESIAN_POINT('',(0.006,-0.00745061609897327,0.0094068230421179));
#24230=CARTESIAN_POINT('Origin',(0.,0.,0.));
#24231=CARTESIAN_POINT('Origin',(-0.01,0.,0.));
#24232=CARTESIAN_POINT('',(0.,-0.00338846752237721,0.0115116587792461));
#24233=CARTESIAN_POINT('',(0.006,-0.00338846752237721,0.0115116587792461));
#24234=CARTESIAN_POINT('',(0.,-0.00308610073718624,0.0115963779793493));
#24235=CARTESIAN_POINT('',(0.006,-0.00308610073718624,0.0115963779793493));
#24236=CARTESIAN_POINT('Origin',(0.,0.,0.));
#24237=CARTESIAN_POINT('Origin',(-0.01,0.,0.));
#24238=CARTESIAN_POINT('',(0.,-0.00147831669728109,-0.0119085926852227));
#24239=CARTESIAN_POINT('',(0.006,-0.00147831669728109,-0.0119085926852227));
#24240=CARTESIAN_POINT('',(0.,-0.00178940315151014,-0.0118658348362585));
#24241=CARTESIAN_POINT('',(0.006,-0.00178940315151014,-0.0118658348362585));
#24242=CARTESIAN_POINT('Origin',(0.,0.,0.));
#24243=CARTESIAN_POINT('Origin',(-0.01,0.,0.));
#24244=CARTESIAN_POINT('',(0.,-0.000157005585611382,-0.011998972841293));
#24245=CARTESIAN_POINT('',(0.006,-0.000157005585611383,-0.011998972841293));
#24246=CARTESIAN_POINT('',(0.,0.000157005585611632,-0.011998972841293));
#24247=CARTESIAN_POINT('Origin',(0.,0.,0.));
#24248=CARTESIAN_POINT('',(0.006,0.000157005585611632,-0.011998972841293));
#24249=CARTESIAN_POINT('Origin',(-0.01,0.,0.));
#24250=CARTESIAN_POINT('',(0.,-0.00308610073718608,-0.0115963779793494));
#24251=CARTESIAN_POINT('',(0.006,-0.00308610073718608,-0.0115963779793494));
#24252=CARTESIAN_POINT('',(0.,-0.00338846752237705,-0.0115116587792462));
#24253=CARTESIAN_POINT('',(0.006,-0.00338846752237705,-0.0115116587792462));
#24254=CARTESIAN_POINT('Origin',(0.,0.,0.));
#24255=CARTESIAN_POINT('Origin',(-0.01,0.,0.));
#24256=CARTESIAN_POINT('',(0.,-0.00463639655948412,-0.0110681446929105));
#24257=CARTESIAN_POINT('',(0.006,-0.00463639655948412,-0.0110681446929105));
#24258=CARTESIAN_POINT('',(0.,-0.00492441115452883,-0.0109430423000714));
#24259=CARTESIAN_POINT('',(0.006,-0.00492441115452883,-0.0109430423000714));
#24260=CARTESIAN_POINT('Origin',(0.,0.,0.));
#24261=CARTESIAN_POINT('Origin',(-0.01,0.,0.));
#24262=CARTESIAN_POINT('',(0.,-0.00866211623085129,-0.00830468195677731));
#24263=CARTESIAN_POINT('',(0.006,-0.00866211623085129,-0.0083046819567773));
#24264=CARTESIAN_POINT('',(0.,-0.00887644554277534,-0.00807519129966243));
#24265=CARTESIAN_POINT('',(0.006,-0.00887644554277533,-0.00807519129966243));
#24266=CARTESIAN_POINT('Origin',(0.,0.,0.));
#24267=CARTESIAN_POINT('Origin',(-0.01,0.,0.));
#24268=CARTESIAN_POINT('',(0.,-0.00769419810989815,-0.00920865437757546));
#24269=CARTESIAN_POINT('',(0.006,-0.00769419810989815,-0.00920865437757546));
#24270=CARTESIAN_POINT('',(0.,-0.00745061609897314,-0.009406823042118));
#24271=CARTESIAN_POINT('Origin',(0.,0.,0.));
#24272=CARTESIAN_POINT('',(0.006,-0.00745061609897314,-0.009406823042118));
#24273=CARTESIAN_POINT('Origin',(-0.01,0.,0.));
#24274=CARTESIAN_POINT('',(0.,-0.00610032508627815,-0.0103337328125767));
#24275=CARTESIAN_POINT('',(0.006,-0.00610032508627815,-0.0103337328125767));
#24276=CARTESIAN_POINT('',(0.,-0.00636862232421547,-0.0101705776478774));
#24277=CARTESIAN_POINT('',(0.006,-0.00636862232421547,-0.0101705776478774));
#24278=CARTESIAN_POINT('Origin',(0.,0.,0.));
#24279=CARTESIAN_POINT('Origin',(-0.01,0.,0.));
#24280=CARTESIAN_POINT('',(0.,-0.0105814778411272,-0.00565971083163568));
#24281=CARTESIAN_POINT('',(0.006,-0.0105814778411272,-0.00565971083163568));
#24282=CARTESIAN_POINT('',(0.,-0.0107259434024639,-0.00538090495429355));
#24283=CARTESIAN_POINT('',(0.006,-0.0107259434024639,-0.00538090495429355));
#24284=CARTESIAN_POINT('Origin',(0.,0.,0.));
#24285=CARTESIAN_POINT('Origin',(-0.01,0.,0.));
#24286=CARTESIAN_POINT('',(0.,-0.00989334159007055,-0.00679130268668539));
#24287=CARTESIAN_POINT('',(0.006,-0.00989334159007055,-0.00679130268668539));
#24288=CARTESIAN_POINT('',(0.,-0.009712257526702,-0.00704784035964354));
#24289=CARTESIAN_POINT('Origin',(0.,0.,0.));
#24290=CARTESIAN_POINT('',(0.006,-0.009712257526702,-0.00704784035964354));
#24291=CARTESIAN_POINT('Origin',(-0.01,0.,0.));
#24292=CARTESIAN_POINT('',(0.,-0.0112535852442971,-0.00416615159941858));
#24293=CARTESIAN_POINT('',(0.006,-0.0112535852442971,-0.00416615159941858));
#24294=CARTESIAN_POINT('',(0.,-0.0113587411835336,-0.00387027114366637));
#24295=CARTESIAN_POINT('',(0.006,-0.0113587411835336,-0.00387027114366637));
#24296=CARTESIAN_POINT('Origin',(0.,0.,0.));
#24297=CARTESIAN_POINT('Origin',(-0.01,0.,0.));
#24298=CARTESIAN_POINT('',(0.,-0.0117160596469668,-0.00259498484556586));
#24299=CARTESIAN_POINT('',(0.006,-0.0117160596469668,-0.00259498484556586));
#24300=CARTESIAN_POINT('',(0.,-0.0117799471079178,-0.00228754150446692));
#24301=CARTESIAN_POINT('',(0.006,-0.0117799471079178,-0.00228754150446692));
#24302=CARTESIAN_POINT('Origin',(0.,0.,0.));
#24303=CARTESIAN_POINT('Origin',(-0.01,0.,0.));
#24304=CARTESIAN_POINT('',(0.,0.0117799471079179,-0.00228754150446667));
#24305=CARTESIAN_POINT('',(0.006,0.0117799471079179,-0.00228754150446667));
#24306=CARTESIAN_POINT('',(0.,0.0117160596469668,-0.00259498484556562));
#24307=CARTESIAN_POINT('',(0.006,0.0117160596469668,-0.00259498484556562));
#24308=CARTESIAN_POINT('Origin',(0.,0.,0.));
#24309=CARTESIAN_POINT('Origin',(-0.01,0.,0.));
#24310=CARTESIAN_POINT('',(0.,0.0119602860260496,-0.000975478433939885));
#24311=CARTESIAN_POINT('',(0.006,0.0119602860260496,-0.000975478433939885));
#24312=CARTESIAN_POINT('',(0.,0.0119817149061973,-0.000662199295233908));
#24313=CARTESIAN_POINT('Origin',(0.,0.,0.));
#24314=CARTESIAN_POINT('',(0.006,0.0119817149061973,-0.000662199295233907));
#24315=CARTESIAN_POINT('Origin',(-0.01,0.,0.));
#24316=CARTESIAN_POINT('',(0.,0.0113587411835337,-0.00387027114366614));
#24317=CARTESIAN_POINT('',(0.006,0.0113587411835337,-0.00387027114366614));
#24318=CARTESIAN_POINT('',(0.,0.0112535852442972,-0.00416615159941835));
#24319=CARTESIAN_POINT('',(0.006,0.0112535852442972,-0.00416615159941835));
#24320=CARTESIAN_POINT('Origin',(0.,0.,0.));
#24321=CARTESIAN_POINT('Origin',(-0.01,0.,0.));
#24322=CARTESIAN_POINT('',(0.,0.010725943402464,-0.00538090495429333));
#24323=CARTESIAN_POINT('',(0.006,0.010725943402464,-0.00538090495429333));
#24324=CARTESIAN_POINT('',(0.,0.0105814778411273,-0.00565971083163546));
#24325=CARTESIAN_POINT('',(0.006,0.0105814778411273,-0.00565971083163546));
#24326=CARTESIAN_POINT('Origin',(0.,0.,0.));
#24327=CARTESIAN_POINT('Origin',(-0.01,0.,0.));
#24328=CARTESIAN_POINT('',(0.,0.00769419810989834,-0.0092086543775753));
#24329=CARTESIAN_POINT('',(0.006,0.00769419810989834,-0.0092086543775753));
#24330=CARTESIAN_POINT('',(0.,0.00745061609897333,-0.00940682304211785));
#24331=CARTESIAN_POINT('',(0.006,0.00745061609897333,-0.00940682304211785));
#24332=CARTESIAN_POINT('Origin',(0.,0.,0.));
#24333=CARTESIAN_POINT('Origin',(-0.01,0.,0.));
#24334=CARTESIAN_POINT('',(0.,0.00866211623085146,-0.00830468195677713));
#24335=CARTESIAN_POINT('',(0.006,0.00866211623085146,-0.00830468195677713));
#24336=CARTESIAN_POINT('',(0.,0.0088764455427755,-0.00807519129966225));
#24337=CARTESIAN_POINT('Origin',(0.,0.,0.));
#24338=CARTESIAN_POINT('',(0.006,0.0088764455427755,-0.00807519129966225));
#24339=CARTESIAN_POINT('Origin',(-0.01,0.,0.));
#24340=CARTESIAN_POINT('',(0.,0.00989334159007069,-0.00679130268668519));
#24341=CARTESIAN_POINT('',(0.006,0.00989334159007069,-0.00679130268668519));
#24342=CARTESIAN_POINT('',(0.,0.00971225752670214,-0.00704784035964334));
#24343=CARTESIAN_POINT('',(0.006,0.00971225752670214,-0.00704784035964334));
#24344=CARTESIAN_POINT('Origin',(0.,0.,0.));
#24345=CARTESIAN_POINT('Origin',(-0.01,0.,0.));
#24346=CARTESIAN_POINT('',(0.,0.00492441115452905,-0.0109430423000713));
#24347=CARTESIAN_POINT('',(0.006,0.00492441115452905,-0.0109430423000713));
#24348=CARTESIAN_POINT('',(0.,0.00463639655948435,-0.0110681446929104));
#24349=CARTESIAN_POINT('',(0.006,0.00463639655948435,-0.0110681446929104));
#24350=CARTESIAN_POINT('Origin',(0.,0.,0.));
#24351=CARTESIAN_POINT('Origin',(-0.01,0.,0.));
#24352=CARTESIAN_POINT('',(0.,0.00610032508627836,-0.0103337328125766));
#24353=CARTESIAN_POINT('',(0.006,0.00610032508627836,-0.0103337328125766));
#24354=CARTESIAN_POINT('',(0.,0.00636862232421567,-0.0101705776478773));
#24355=CARTESIAN_POINT('Origin',(0.,0.,0.));
#24356=CARTESIAN_POINT('',(0.006,0.00636862232421567,-0.0101705776478773));
#24357=CARTESIAN_POINT('Origin',(-0.01,0.,0.));
#24358=CARTESIAN_POINT('',(0.,0.00338846752237729,-0.0115116587792461));
#24359=CARTESIAN_POINT('',(0.006,0.00338846752237729,-0.0115116587792461));
#24360=CARTESIAN_POINT('',(0.,0.00308610073718632,-0.0115963779793493));
#24361=CARTESIAN_POINT('',(0.006,0.00308610073718632,-0.0115963779793493));
#24362=CARTESIAN_POINT('Origin',(0.,0.,0.));
#24363=CARTESIAN_POINT('Origin',(-0.01,0.,0.));
#24364=CARTESIAN_POINT('',(0.,0.00178940315151039,-0.0118658348362584));
#24365=CARTESIAN_POINT('',(0.006,0.00178940315151039,-0.0118658348362584));
#24366=CARTESIAN_POINT('',(0.,0.00147831669728134,-0.0119085926852227));
#24367=CARTESIAN_POINT('',(0.006,0.00147831669728134,-0.0119085926852227));
#24368=CARTESIAN_POINT('Origin',(0.,0.,0.));
#24369=CARTESIAN_POINT('Origin',(0.,0.,0.));
#24370=CARTESIAN_POINT('',(0.,-0.000521792360520078,0.0108614735985732));
#24371=CARTESIAN_POINT('Origin',(0.,0.00400379034671789,0.010037397655502));
#24372=CARTESIAN_POINT('',(0.,0.000521792360520001,0.0108614735985732));
#24373=CARTESIAN_POINT('Origin',(0.,-0.00400379034671796,0.010037397655502));
#24374=CARTESIAN_POINT('',(0.,0.000962038105848705,0.0108313599646072));
#24375=CARTESIAN_POINT('Origin',(0.,0.,0.));
#24376=CARTESIAN_POINT('Origin',(0.,0.00533325763176559,0.00939872607688742));
#24377=CARTESIAN_POINT('',(0.,0.00199590282248136,0.0106892585300951));
#24378=CARTESIAN_POINT('Origin',(0.,-0.00259974002297318,0.0104890915072804));
#24379=CARTESIAN_POINT('',(0.,0.00242794762255152,0.0105994785882206));
#24380=CARTESIAN_POINT('Origin',(0.,0.,0.));
#24381=CARTESIAN_POINT('Origin',(0.,0.00656337641804445,0.00858497401453304));
#24382=CARTESIAN_POINT('',(0.,0.00343283339125305,0.0103179228000552));
#24383=CARTESIAN_POINT('Origin',(0.,-0.00114726146149743,0.0107453934304013));
#24384=CARTESIAN_POINT('',(0.,0.00384862906889953,0.0101701489807191));
#24385=CARTESIAN_POINT('Origin',(0.,0.,0.));
#24386=CARTESIAN_POINT('Origin',(0.,0.00767123192004022,0.00761130012968254));
#24387=CARTESIAN_POINT('',(0.,0.00480581676911591,0.00975438369050984));
#24388=CARTESIAN_POINT('Origin',(0.,0.00032658841030397,0.0108015290049791));
#24389=CARTESIAN_POINT('',(0.,0.00519761783757978,0.00955136874036766));
#24390=CARTESIAN_POINT('Origin',(0.,0.,0.));
#24391=CARTESIAN_POINT('Origin',(0.,0.00863618688589385,0.00649584212454895));
#24392=CARTESIAN_POINT('',(0.,0.00608927687352466,0.00900913886881303));
#24393=CARTESIAN_POINT('Origin',(0.,0.00179435455795041,0.0106564525314718));
#24394=CARTESIAN_POINT('',(0.,0.00644978482021654,0.00875466457226685));
#24395=CARTESIAN_POINT('Origin',(0.,0.,0.));
#24396=CARTESIAN_POINT('Origin',(0.,0.00944026603035638,0.00525937887124031));
#24397=CARTESIAN_POINT('',(0.,0.00725930527113395,0.00809607083593559));
#24398=CARTESIAN_POINT('Origin',(0.,0.00322869527523144,0.0103128665100857));
#24399=CARTESIAN_POINT('',(0.,0.00758180451511419,0.00779487756764621));
#24400=CARTESIAN_POINT('Origin',(0.,0.,0.));
#24401=CARTESIAN_POINT('Origin',(0.,0.0100684908803426,0.00392494334068744));
#24402=CARTESIAN_POINT('',(0.,0.00829410654667506,0.00703218832173896));
#24403=CARTESIAN_POINT('Origin',(0.,0.00460289150846097,0.00977717129830952));
#24404=CARTESIAN_POINT('',(0.,0.00857258953722032,0.00668988674241506));
#24405=CARTESIAN_POINT('Origin',(0.,0.,0.));
#24406=CARTESIAN_POINT('Origin',(0.,0.0105091587955444,0.00251739354197556));
#24407=CARTESIAN_POINT('',(0.,0.00917440431030386,0.00583730944451961));
#24408=CARTESIAN_POINT('Origin',(0.,0.00589134458189306,0.00905934588436432));
#24409=CARTESIAN_POINT('',(0.,0.00940368343621032,0.00546027598492453));
#24410=CARTESIAN_POINT('Origin',(0.,0.,0.));
#24411=CARTESIAN_POINT('Origin',(0.,0.0107540609664773,0.00106294946466816));
#24412=CARTESIAN_POINT('',(0.,0.00988380028027128,0.00453369253696249));
#24413=CARTESIAN_POINT('Origin',(0.,0.0070700530526165,0.00817276199753411));
#24414=CARTESIAN_POINT('',(0.,0.0100596045052361,0.00412895061707378));
#24415=CARTESIAN_POINT('Origin',(0.,0.,0.));
#24416=CARTESIAN_POINT('Origin',(0.,0.0107986353290695,-0.000411295349988374));
#24417=CARTESIAN_POINT('',(0.,0.0104090797518855,0.00314562151551744));
#24418=CARTESIAN_POINT('Origin',(0.,0.00811705981202379,0.00713393501814937));
#24419=CARTESIAN_POINT('',(0.,0.010528134175832,0.00272071071150152));
#24420=CARTESIAN_POINT('Origin',(0.,0.,0.));
#24421=CARTESIAN_POINT('Origin',(0.,0.0106420515472837,-0.00187787851047532));
#24422=CARTESIAN_POINT('',(0.,0.0107404577624574,0.00169895351698278));
#24423=CARTESIAN_POINT('Origin',(0.,0.00901286110520005,0.00596221632729992));
#24424=CARTESIAN_POINT('',(0.,0.0108005446267269,0.00126178911315635));
#24425=CARTESIAN_POINT('Origin',(0.,0.,0.));
#24426=CARTESIAN_POINT('',(0.,0.0119602860260496,0.00097547843394005));
#24427=CARTESIAN_POINT('Origin',(0.,0.0102872264807069,-0.00330948034739469));
#24428=CARTESIAN_POINT('',(0.,0.0119817149061973,0.000662199295233908));
#24429=CARTESIAN_POINT('Origin',(0.,0.,0.));
#24430=CARTESIAN_POINT('',(0.,0.0108717613666412,0.000220637228970242));
#24431=CARTESIAN_POINT('Origin',(0.,0.00974076984897452,0.00467943282721939));
#24432=CARTESIAN_POINT('',(0.,0.0108717613666412,-0.000220637228970241));
#24433=CARTESIAN_POINT('Origin',(0.,0.,0.));
#24434=CARTESIAN_POINT('Origin',(0.,0.00974076984897452,-0.00467943282721939));
#24435=CARTESIAN_POINT('',(0.,0.0108005446267269,-0.0012617891131562));
#24436=CARTESIAN_POINT('Origin',(0.,0.0102872264807069,0.00330948034739484));
#24437=CARTESIAN_POINT('',(0.,0.0107404577624574,-0.00169895351698263));
#24438=CARTESIAN_POINT('Origin',(0.,0.,0.));
#24439=CARTESIAN_POINT('Origin',(0.,0.00901286110520013,-0.00596221632729979));
#24440=CARTESIAN_POINT('',(0.,0.010528134175832,-0.00272071071150138));
#24441=CARTESIAN_POINT('Origin',(0.,0.0106420515472837,0.00187787851047546));
#24442=CARTESIAN_POINT('',(0.,0.0104090797518856,-0.0031456215155173));
#24443=CARTESIAN_POINT('Origin',(0.,0.,0.));
#24444=CARTESIAN_POINT('Origin',(0.,0.00811705981202389,-0.00713393501814925));
#24445=CARTESIAN_POINT('',(0.,0.0100596045052361,-0.00412895061707364));
#24446=CARTESIAN_POINT('Origin',(0.,0.0107986353290695,0.000411295349988523));
#24447=CARTESIAN_POINT('',(0.,0.00988380028027134,-0.00453369253696235));
#24448=CARTESIAN_POINT('Origin',(0.,0.,0.));
#24449=CARTESIAN_POINT('Origin',(0.,0.00707005305261661,-0.00817276199753401));
#24450=CARTESIAN_POINT('',(0.,0.0094036834362104,-0.0054602759849244));
#24451=CARTESIAN_POINT('Origin',(0.,0.0107540609664773,-0.00106294946466802));
#24452=CARTESIAN_POINT('',(0.,0.00917440431030394,-0.00583730944451949));
#24453=CARTESIAN_POINT('Origin',(0.,0.,0.));
#24454=CARTESIAN_POINT('Origin',(0.,0.00589134458189318,-0.00905934588436424));
#24455=CARTESIAN_POINT('',(0.,0.00857258953722041,-0.00668988674241494));
#24456=CARTESIAN_POINT('Origin',(0.,0.0105091587955445,-0.00251739354197541));
#24457=CARTESIAN_POINT('',(0.,0.00829410654667516,-0.00703218832173885));
#24458=CARTESIAN_POINT('Origin',(0.,0.,0.));
#24459=CARTESIAN_POINT('Origin',(0.,0.0046028915084611,-0.00977717129830945));
#24460=CARTESIAN_POINT('',(0.,0.0075818045151143,-0.0077948775676461));
#24461=CARTESIAN_POINT('Origin',(0.,0.0100684908803427,-0.0039249433406873));
#24462=CARTESIAN_POINT('',(0.,0.00725930527113406,-0.00809607083593549));
#24463=CARTESIAN_POINT('Origin',(0.,0.,0.));
#24464=CARTESIAN_POINT('Origin',(0.,0.00322869527523158,-0.0103128665100857));
#24465=CARTESIAN_POINT('',(0.,0.00644978482021666,-0.00875466457226676));
#24466=CARTESIAN_POINT('Origin',(0.,0.00944026603035645,-0.00525937887124018));
#24467=CARTESIAN_POINT('',(0.,0.00608927687352479,-0.00900913886881295));
#24468=CARTESIAN_POINT('Origin',(0.,0.,0.));
#24469=CARTESIAN_POINT('Origin',(0.,0.00179435455795055,-0.0106564525314718));
#24470=CARTESIAN_POINT('',(0.,0.00519761783757991,-0.00955136874036759));
#24471=CARTESIAN_POINT('Origin',(0.,0.00863618688589394,-0.00649584212454884));
#24472=CARTESIAN_POINT('',(0.,0.00480581676911604,-0.00975438369050977));
#24473=CARTESIAN_POINT('Origin',(0.,0.,0.));
#24474=CARTESIAN_POINT('Origin',(0.,0.000326588410304114,-0.0108015290049791));
#24475=CARTESIAN_POINT('',(0.,0.00384862906889967,-0.010170148980719));
#24476=CARTESIAN_POINT('Origin',(0.,0.00767123192004033,-0.00761130012968243));
#24477=CARTESIAN_POINT('',(0.,0.00343283339125319,-0.0103179228000551));
#24478=CARTESIAN_POINT('Origin',(0.,0.,0.));
#24479=CARTESIAN_POINT('Origin',(0.,-0.00114726146149728,-0.0107453934304014));
#24480=CARTESIAN_POINT('',(0.,0.00242794762255167,-0.0105994785882205));
#24481=CARTESIAN_POINT('Origin',(0.,0.00656337641804457,-0.00858497401453295));
#24482=CARTESIAN_POINT('',(0.,0.00199590282248151,-0.0106892585300951));
#24483=CARTESIAN_POINT('Origin',(0.,0.,0.));
#24484=CARTESIAN_POINT('Origin',(0.,-0.00259974002297304,-0.0104890915072804));
#24485=CARTESIAN_POINT('',(0.,0.000962038105848858,-0.0108313599646072));
#24486=CARTESIAN_POINT('Origin',(0.,0.00533325763176572,-0.00939872607688735));
#24487=CARTESIAN_POINT('',(0.,0.000521792360520154,-0.0108614735985732));
#24488=CARTESIAN_POINT('Origin',(0.,0.,0.));
#24489=CARTESIAN_POINT('Origin',(0.,-0.00400379034671782,-0.0100373976555021));
#24490=CARTESIAN_POINT('',(0.,-0.000521792360519925,-0.0108614735985732));
#24491=CARTESIAN_POINT('Origin',(0.,0.00400379034671803,-0.010037397655502));
#24492=CARTESIAN_POINT('',(0.,-0.00096203810584863,-0.0108313599646072));
#24493=CARTESIAN_POINT('Origin',(0.,0.,0.));
#24494=CARTESIAN_POINT('Origin',(0.,-0.00533325763176552,-0.00939872607688746));
#24495=CARTESIAN_POINT('',(0.,-0.00199590282248128,-0.0106892585300951));
#24496=CARTESIAN_POINT('Origin',(0.,0.00259974002297325,-0.0104890915072803));
#24497=CARTESIAN_POINT('',(0.,-0.00242794762255145,-0.0105994785882206));
#24498=CARTESIAN_POINT('Origin',(0.,0.,0.));
#24499=CARTESIAN_POINT('Origin',(0.,-0.00656337641804439,-0.00858497401453309));
#24500=CARTESIAN_POINT('',(0.,-0.00343283339125298,-0.0103179228000552));
#24501=CARTESIAN_POINT('Origin',(0.,0.0011472614614975,-0.0107453934304013));
#24502=CARTESIAN_POINT('',(0.,-0.00384862906889946,-0.0101701489807191));
#24503=CARTESIAN_POINT('Origin',(0.,0.,0.));
#24504=CARTESIAN_POINT('Origin',(0.,-0.00767123192004017,-0.00761130012968259));
#24505=CARTESIAN_POINT('',(0.,-0.00480581676911584,-0.00975438369050987));
#24506=CARTESIAN_POINT('Origin',(0.,-0.000326588410303897,-0.0108015290049791));
#24507=CARTESIAN_POINT('',(0.,-0.00519761783757972,-0.00955136874036769));
#24508=CARTESIAN_POINT('Origin',(0.,0.,0.));
#24509=CARTESIAN_POINT('Origin',(0.,-0.00863618688589381,-0.00649584212454901));
#24510=CARTESIAN_POINT('',(0.,-0.0060892768735246,-0.00900913886881307));
#24511=CARTESIAN_POINT('Origin',(0.,-0.00179435455795034,-0.0106564525314718));
#24512=CARTESIAN_POINT('',(0.,-0.00644978482021648,-0.00875466457226689));
#24513=CARTESIAN_POINT('Origin',(0.,0.,0.));
#24514=CARTESIAN_POINT('Origin',(0.,-0.00944026603035634,-0.00525937887124037));
#24515=CARTESIAN_POINT('',(0.,-0.0072593052711339,-0.00809607083593564));
#24516=CARTESIAN_POINT('Origin',(0.,-0.00322869527523136,-0.0103128665100857));
#24517=CARTESIAN_POINT('',(0.,-0.00758180451511414,-0.00779487756764626));
#24518=CARTESIAN_POINT('Origin',(0.,0.,0.));
#24519=CARTESIAN_POINT('Origin',(0.,-0.0100684908803426,-0.00392494334068751));
#24520=CARTESIAN_POINT('',(0.,-0.00829410654667501,-0.00703218832173902));
#24521=CARTESIAN_POINT('Origin',(0.,-0.0046028915084609,-0.00977717129830955));
#24522=CARTESIAN_POINT('',(0.,-0.00857258953722027,-0.00668988674241512));
#24523=CARTESIAN_POINT('Origin',(0.,0.,0.));
#24524=CARTESIAN_POINT('Origin',(0.,-0.0105091587955444,-0.00251739354197563));
#24525=CARTESIAN_POINT('',(0.,-0.00917440431030382,-0.00583730944451968));
#24526=CARTESIAN_POINT('Origin',(0.,-0.00589134458189299,-0.00905934588436437));
#24527=CARTESIAN_POINT('',(0.,-0.00940368343621029,-0.0054602759849246));
#24528=CARTESIAN_POINT('Origin',(0.,0.,0.));
#24529=CARTESIAN_POINT('Origin',(0.,-0.0107540609664773,-0.00106294946466824));
#24530=CARTESIAN_POINT('',(0.,-0.00988380028027125,-0.00453369253696255));
#24531=CARTESIAN_POINT('Origin',(0.,-0.00707005305261645,-0.00817276199753415));
#24532=CARTESIAN_POINT('',(0.,-0.010059604505236,-0.00412895061707385));
#24533=CARTESIAN_POINT('Origin',(0.,0.,0.));
#24534=CARTESIAN_POINT('Origin',(0.,-0.0107986353290695,0.0004112953499883));
#24535=CARTESIAN_POINT('',(0.,-0.0104090797518855,-0.00314562151551751));
#24536=CARTESIAN_POINT('Origin',(0.,-0.00811705981202375,-0.00713393501814942));
#24537=CARTESIAN_POINT('',(0.,-0.0105281341758319,-0.00272071071150159));
#24538=CARTESIAN_POINT('Origin',(0.,0.,0.));
#24539=CARTESIAN_POINT('Origin',(0.,-0.0106420515472838,0.00187787851047525));
#24540=CARTESIAN_POINT('',(0.,-0.0107404577624574,-0.00169895351698286));
#24541=CARTESIAN_POINT('Origin',(0.,-0.0090128611052,-0.00596221632729998));
#24542=CARTESIAN_POINT('',(0.,-0.0108005446267269,-0.00126178911315643));
#24543=CARTESIAN_POINT('Origin',(0.,0.,0.));
#24544=CARTESIAN_POINT('Origin',(0.,-0.0102872264807069,0.00330948034739461));
#24545=CARTESIAN_POINT('',(0.,-0.0108717613666412,-0.000220637228970318));
#24546=CARTESIAN_POINT('Origin',(0.,-0.00974076984897448,-0.00467943282721946));
#24547=CARTESIAN_POINT('',(0.,-0.0108717613666412,0.000220637228970165));
#24548=CARTESIAN_POINT('Origin',(0.,0.,0.));
#24549=CARTESIAN_POINT('Origin',(0.,-0.00974076984897455,0.00467943282721932));
#24550=CARTESIAN_POINT('',(0.,-0.0108005446267269,0.00126178911315627));
#24551=CARTESIAN_POINT('Origin',(0.,-0.0102872264807069,-0.00330948034739476));
#24552=CARTESIAN_POINT('',(0.,-0.0107404577624574,0.00169895351698271));
#24553=CARTESIAN_POINT('Origin',(0.,0.,0.));
#24554=CARTESIAN_POINT('Origin',(0.,-0.00901286110520009,0.00596221632729986));
#24555=CARTESIAN_POINT('',(0.,-0.010528134175832,0.00272071071150145));
#24556=CARTESIAN_POINT('Origin',(0.,-0.0106420515472837,-0.00187787851047538));
#24557=CARTESIAN_POINT('',(0.,-0.0104090797518856,0.00314562151551737));
#24558=CARTESIAN_POINT('Origin',(0.,0.,0.));
#24559=CARTESIAN_POINT('Origin',(0.,-0.00811705981202384,0.00713393501814931));
#24560=CARTESIAN_POINT('',(0.,-0.0100596045052361,0.00412895061707371));
#24561=CARTESIAN_POINT('Origin',(0.,-0.0107986353290695,-0.000411295349988447));
#24562=CARTESIAN_POINT('',(0.,-0.00988380028027131,0.00453369253696241));
#24563=CARTESIAN_POINT('Origin',(0.,0.,0.));
#24564=CARTESIAN_POINT('Origin',(0.,-0.00707005305261656,0.00817276199753406));
#24565=CARTESIAN_POINT('',(0.,-0.00940368343621036,0.00546027598492447));
#24566=CARTESIAN_POINT('Origin',(0.,-0.0107540609664773,0.00106294946466809));
#24567=CARTESIAN_POINT('',(0.,-0.0091744043103039,0.00583730944451955));
#24568=CARTESIAN_POINT('Origin',(0.,0.,0.));
#24569=CARTESIAN_POINT('Origin',(0.,-0.00589134458189312,0.00905934588436428));
#24570=CARTESIAN_POINT('',(0.,-0.00857258953722036,0.006689886742415));
#24571=CARTESIAN_POINT('Origin',(0.,-0.0105091587955445,0.00251739354197548));
#24572=CARTESIAN_POINT('',(0.,-0.00829410654667511,0.00703218832173891));
#24573=CARTESIAN_POINT('Origin',(0.,0.,0.));
#24574=CARTESIAN_POINT('Origin',(0.,-0.00460289150846104,0.00977717129830948));
#24575=CARTESIAN_POINT('',(0.,-0.00758180451511425,0.00779487756764615));
#24576=CARTESIAN_POINT('Origin',(0.,-0.0100684908803427,0.00392494334068737));
#24577=CARTESIAN_POINT('',(0.,-0.00725930527113401,0.00809607083593554));
#24578=CARTESIAN_POINT('Origin',(0.,0.,0.));
#24579=CARTESIAN_POINT('Origin',(0.,-0.00322869527523151,0.0103128665100857));
#24580=CARTESIAN_POINT('',(0.,-0.0064497848202166,0.0087546645722668));
#24581=CARTESIAN_POINT('Origin',(0.,-0.00944026603035641,0.00525937887124024));
#24582=CARTESIAN_POINT('',(0.,-0.00608927687352473,0.00900913886881298));
#24583=CARTESIAN_POINT('Origin',(0.,0.,0.));
#24584=CARTESIAN_POINT('Origin',(0.,-0.00179435455795048,0.0106564525314718));
#24585=CARTESIAN_POINT('',(0.,-0.00519761783757985,0.00955136874036762));
#24586=CARTESIAN_POINT('Origin',(0.,-0.0086361868858939,0.00649584212454889));
#24587=CARTESIAN_POINT('',(0.,-0.00480581676911598,0.0097543836905098));
#24588=CARTESIAN_POINT('Origin',(0.,0.,0.));
#24589=CARTESIAN_POINT('Origin',(0.,-0.000326588410304044,0.0108015290049791));
#24590=CARTESIAN_POINT('',(0.,-0.0038486290688996,0.0101701489807191));
#24591=CARTESIAN_POINT('Origin',(0.,-0.00767123192004028,0.00761130012968249));
#24592=CARTESIAN_POINT('',(0.,-0.00343283339125312,0.0103179228000551));
#24593=CARTESIAN_POINT('Origin',(0.,0.,0.));
#24594=CARTESIAN_POINT('Origin',(0.,0.00114726146149736,0.0107453934304013));
#24595=CARTESIAN_POINT('',(0.,-0.0024279476225516,0.0105994785882205));
#24596=CARTESIAN_POINT('Origin',(0.,-0.00656337641804451,0.008584974014533));
#24597=CARTESIAN_POINT('',(0.,-0.00199590282248143,0.0106892585300951));
#24598=CARTESIAN_POINT('Origin',(0.,0.,0.));
#24599=CARTESIAN_POINT('Origin',(0.,0.00259974002297311,0.0104890915072804));
#24600=CARTESIAN_POINT('',(0.,-0.000962038105848782,0.0108313599646072));
#24601=CARTESIAN_POINT('Origin',(0.,-0.00533325763176565,0.00939872607688738));
#24602=CARTESIAN_POINT('Origin',(0.,0.,0.));
#24603=CARTESIAN_POINT('',(0.,0.,-0.009));
#24604=CARTESIAN_POINT('Origin',(0.,0.,0.));
#24605=CARTESIAN_POINT('Origin',(-0.01,0.,0.));
#24606=CARTESIAN_POINT('',(0.006,0.0119602860260496,0.00097547843394005));
#24607=CARTESIAN_POINT('',(0.006,0.0119817149061973,0.000662199295233907));
#24608=CARTESIAN_POINT('Origin',(0.012,0.00974076984897452,-0.00467943282721939));
#24609=CARTESIAN_POINT('',(0.012,0.0108717613666412,-0.000220637228970241));
#24610=CARTESIAN_POINT('Origin',(0.012,0.00974076984897452,0.00467943282721939));
#24611=CARTESIAN_POINT('',(0.012,0.0108717613666412,0.000220637228970242));
#24612=CARTESIAN_POINT('Origin',(0.012,0.,0.));
#24613=CARTESIAN_POINT('Origin',(0.012,0.0102872264807069,-0.00330948034739469));
#24614=CARTESIAN_POINT('',(0.012,0.0108005446267269,0.00126178911315635));
#24615=CARTESIAN_POINT('Origin',(0.012,0.00901286110520005,0.00596221632729992));
#24616=CARTESIAN_POINT('',(0.012,0.0107404577624574,0.00169895351698278));
#24617=CARTESIAN_POINT('Origin',(0.012,0.,0.));
#24618=CARTESIAN_POINT('Origin',(0.012,-0.00400379034671782,-0.0100373976555021));
#24619=CARTESIAN_POINT('',(0.012,0.000521792360520154,-0.0108614735985732));
#24620=CARTESIAN_POINT('Origin',(0.012,0.00533325763176572,-0.00939872607688735));
#24621=CARTESIAN_POINT('',(0.012,0.000962038105848858,-0.0108313599646072));
#24622=CARTESIAN_POINT('Origin',(0.012,0.,0.));
#24623=CARTESIAN_POINT('Origin',(0.012,-0.00259974002297304,-0.0104890915072804));
#24624=CARTESIAN_POINT('',(0.012,0.00199590282248151,-0.0106892585300951));
#24625=CARTESIAN_POINT('Origin',(0.012,0.00656337641804457,-0.00858497401453295));
#24626=CARTESIAN_POINT('',(0.012,0.00242794762255167,-0.0105994785882205));
#24627=CARTESIAN_POINT('Origin',(0.012,0.,0.));
#24628=CARTESIAN_POINT('Origin',(0.012,-0.00114726146149728,-0.0107453934304014));
#24629=CARTESIAN_POINT('',(0.012,0.00343283339125319,-0.0103179228000551));
#24630=CARTESIAN_POINT('Origin',(0.012,0.00767123192004033,-0.00761130012968243));
#24631=CARTESIAN_POINT('',(0.012,0.00384862906889967,-0.010170148980719));
#24632=CARTESIAN_POINT('Origin',(0.012,0.,0.));
#24633=CARTESIAN_POINT('Origin',(0.012,0.00179435455795055,-0.0106564525314718));
#24634=CARTESIAN_POINT('',(0.012,0.00608927687352478,-0.00900913886881295));
#24635=CARTESIAN_POINT('Origin',(0.012,0.00944026603035645,-0.00525937887124018));
#24636=CARTESIAN_POINT('',(0.012,0.00644978482021666,-0.00875466457226676));
#24637=CARTESIAN_POINT('Origin',(0.012,0.,0.));
#24638=CARTESIAN_POINT('Origin',(0.012,0.000326588410304114,-0.0108015290049791));
#24639=CARTESIAN_POINT('',(0.012,0.00480581676911604,-0.00975438369050977));
#24640=CARTESIAN_POINT('Origin',(0.012,0.00863618688589394,-0.00649584212454884));
#24641=CARTESIAN_POINT('',(0.012,0.00519761783757991,-0.00955136874036759));
#24642=CARTESIAN_POINT('Origin',(0.012,0.,0.));
#24643=CARTESIAN_POINT('Origin',(0.012,0.0046028915084611,-0.00977717129830945));
#24644=CARTESIAN_POINT('',(0.012,0.00829410654667516,-0.00703218832173885));
#24645=CARTESIAN_POINT('Origin',(0.012,0.0105091587955445,-0.00251739354197541));
#24646=CARTESIAN_POINT('',(0.012,0.00857258953722041,-0.00668988674241494));
#24647=CARTESIAN_POINT('Origin',(0.012,0.,0.));
#24648=CARTESIAN_POINT('Origin',(0.012,0.00589134458189318,-0.00905934588436424));
#24649=CARTESIAN_POINT('',(0.012,0.00917440431030394,-0.00583730944451949));
#24650=CARTESIAN_POINT('Origin',(0.012,0.0107540609664773,-0.00106294946466802));
#24651=CARTESIAN_POINT('',(0.012,0.0094036834362104,-0.0054602759849244));
#24652=CARTESIAN_POINT('Origin',(0.012,0.,0.));
#24653=CARTESIAN_POINT('Origin',(0.012,0.00322869527523158,-0.0103128665100857));
#24654=CARTESIAN_POINT('',(0.012,0.00725930527113406,-0.00809607083593549));
#24655=CARTESIAN_POINT('Origin',(0.012,0.0100684908803427,-0.0039249433406873));
#24656=CARTESIAN_POINT('',(0.012,0.0075818045151143,-0.0077948775676461));
#24657=CARTESIAN_POINT('Origin',(0.012,0.,0.));
#24658=CARTESIAN_POINT('Origin',(0.012,0.00707005305261661,-0.00817276199753401));
#24659=CARTESIAN_POINT('',(0.012,0.00988380028027134,-0.00453369253696235));
#24660=CARTESIAN_POINT('Origin',(0.012,0.0107986353290695,0.000411295349988523));
#24661=CARTESIAN_POINT('',(0.012,0.0100596045052361,-0.00412895061707364));
#24662=CARTESIAN_POINT('Origin',(0.012,0.,0.));
#24663=CARTESIAN_POINT('Origin',(0.012,0.00811705981202389,-0.00713393501814925));
#24664=CARTESIAN_POINT('',(0.012,0.0104090797518856,-0.0031456215155173));
#24665=CARTESIAN_POINT('Origin',(0.012,0.0106420515472837,0.00187787851047546));
#24666=CARTESIAN_POINT('',(0.012,0.010528134175832,-0.00272071071150138));
#24667=CARTESIAN_POINT('Origin',(0.012,0.,0.));
#24668=CARTESIAN_POINT('Origin',(0.012,0.00901286110520013,-0.00596221632729979));
#24669=CARTESIAN_POINT('',(0.012,0.0107404577624574,-0.00169895351698263));
#24670=CARTESIAN_POINT('Origin',(0.012,0.0102872264807069,0.00330948034739484));
#24671=CARTESIAN_POINT('',(0.012,0.0108005446267269,-0.0012617891131562));
#24672=CARTESIAN_POINT('Origin',(0.012,0.,0.));
#24673=CARTESIAN_POINT('Origin',(0.012,-0.0102872264807069,0.00330948034739461));
#24674=CARTESIAN_POINT('',(0.012,-0.0108005446267269,-0.00126178911315643));
#24675=CARTESIAN_POINT('Origin',(0.012,-0.0090128611052,-0.00596221632729998));
#24676=CARTESIAN_POINT('',(0.012,-0.0107404577624574,-0.00169895351698286));
#24677=CARTESIAN_POINT('Origin',(0.012,0.,0.));
#24678=CARTESIAN_POINT('Origin',(0.012,-0.0106420515472838,0.00187787851047525));
#24679=CARTESIAN_POINT('',(0.012,-0.0105281341758319,-0.00272071071150159));
#24680=CARTESIAN_POINT('Origin',(0.012,-0.00811705981202375,-0.00713393501814942));
#24681=CARTESIAN_POINT('',(0.012,-0.0104090797518855,-0.00314562151551751));
#24682=CARTESIAN_POINT('Origin',(0.012,0.,0.));
#24683=CARTESIAN_POINT('Origin',(0.012,-0.0107986353290695,0.0004112953499883));
#24684=CARTESIAN_POINT('',(0.012,-0.010059604505236,-0.00412895061707385));
#24685=CARTESIAN_POINT('Origin',(0.012,-0.00707005305261645,-0.00817276199753415));
#24686=CARTESIAN_POINT('',(0.012,-0.00988380028027125,-0.00453369253696255));
#24687=CARTESIAN_POINT('Origin',(0.012,0.,0.));
#24688=CARTESIAN_POINT('Origin',(0.012,-0.0105091587955444,-0.00251739354197563));
#24689=CARTESIAN_POINT('',(0.012,-0.00857258953722027,-0.00668988674241512));
#24690=CARTESIAN_POINT('Origin',(0.012,-0.0046028915084609,-0.00977717129830955));
#24691=CARTESIAN_POINT('',(0.012,-0.00829410654667501,-0.00703218832173902));
#24692=CARTESIAN_POINT('Origin',(0.012,0.,0.));
#24693=CARTESIAN_POINT('Origin',(0.012,-0.0107540609664773,-0.00106294946466824));
#24694=CARTESIAN_POINT('',(0.012,-0.00940368343621029,-0.0054602759849246));
#24695=CARTESIAN_POINT('Origin',(0.012,-0.00589134458189299,-0.00905934588436437));
#24696=CARTESIAN_POINT('',(0.012,-0.00917440431030382,-0.00583730944451968));
#24697=CARTESIAN_POINT('Origin',(0.012,0.,0.));
#24698=CARTESIAN_POINT('Origin',(0.012,-0.00944026603035634,-0.00525937887124037));
#24699=CARTESIAN_POINT('',(0.012,-0.00644978482021648,-0.00875466457226689));
#24700=CARTESIAN_POINT('Origin',(0.012,-0.00179435455795034,-0.0106564525314718));
#24701=CARTESIAN_POINT('',(0.012,-0.0060892768735246,-0.00900913886881307));
#24702=CARTESIAN_POINT('Origin',(0.012,0.,0.));
#24703=CARTESIAN_POINT('Origin',(0.012,-0.00863618688589381,-0.00649584212454901));
#24704=CARTESIAN_POINT('',(0.012,-0.00519761783757972,-0.00955136874036769));
#24705=CARTESIAN_POINT('Origin',(0.012,-0.000326588410303897,-0.0108015290049791));
#24706=CARTESIAN_POINT('',(0.012,-0.00480581676911584,-0.00975438369050987));
#24707=CARTESIAN_POINT('Origin',(0.012,0.,0.));
#24708=CARTESIAN_POINT('Origin',(0.012,-0.0100684908803426,-0.00392494334068751));
#24709=CARTESIAN_POINT('',(0.012,-0.00758180451511414,-0.00779487756764626));
#24710=CARTESIAN_POINT('Origin',(0.012,-0.00322869527523136,-0.0103128665100857));
#24711=CARTESIAN_POINT('',(0.012,-0.0072593052711339,-0.00809607083593564));
#24712=CARTESIAN_POINT('Origin',(0.012,0.,0.));
#24713=CARTESIAN_POINT('Origin',(0.012,-0.00767123192004017,-0.00761130012968259));
#24714=CARTESIAN_POINT('',(0.012,-0.00384862906889946,-0.0101701489807191));
#24715=CARTESIAN_POINT('Origin',(0.012,0.0011472614614975,-0.0107453934304013));
#24716=CARTESIAN_POINT('',(0.012,-0.00343283339125298,-0.0103179228000552));
#24717=CARTESIAN_POINT('Origin',(0.012,0.,0.));
#24718=CARTESIAN_POINT('Origin',(0.012,-0.00656337641804439,-0.00858497401453309));
#24719=CARTESIAN_POINT('',(0.012,-0.00242794762255145,-0.0105994785882206));
#24720=CARTESIAN_POINT('Origin',(0.012,0.00259974002297325,-0.0104890915072803));
#24721=CARTESIAN_POINT('',(0.012,-0.00199590282248128,-0.0106892585300951));
#24722=CARTESIAN_POINT('Origin',(0.012,0.,0.));
#24723=CARTESIAN_POINT('Origin',(0.012,-0.00533325763176552,-0.00939872607688746));
#24724=CARTESIAN_POINT('',(0.012,-0.00096203810584863,-0.0108313599646072));
#24725=CARTESIAN_POINT('Origin',(0.012,0.00400379034671803,-0.010037397655502));
#24726=CARTESIAN_POINT('',(0.012,-0.000521792360519925,-0.0108614735985732));
#24727=CARTESIAN_POINT('Origin',(0.012,0.,0.));
#24728=CARTESIAN_POINT('Origin',(0.012,0.00259974002297311,0.0104890915072804));
#24729=CARTESIAN_POINT('',(0.012,-0.00199590282248143,0.0106892585300951));
#24730=CARTESIAN_POINT('Origin',(0.012,-0.00656337641804451,0.008584974014533));
#24731=CARTESIAN_POINT('',(0.012,-0.0024279476225516,0.0105994785882205));
#24732=CARTESIAN_POINT('Origin',(0.012,0.,0.));
#24733=CARTESIAN_POINT('Origin',(0.012,0.00114726146149736,0.0107453934304013));
#24734=CARTESIAN_POINT('',(0.012,-0.00343283339125312,0.0103179228000551));
#24735=CARTESIAN_POINT('Origin',(0.012,-0.00767123192004028,0.00761130012968249));
#24736=CARTESIAN_POINT('',(0.012,-0.0038486290688996,0.0101701489807191));
#24737=CARTESIAN_POINT('Origin',(0.012,0.,0.));
#24738=CARTESIAN_POINT('Origin',(0.012,-0.00179435455795048,0.0106564525314718));
#24739=CARTESIAN_POINT('',(0.012,-0.00608927687352473,0.00900913886881298));
#24740=CARTESIAN_POINT('Origin',(0.012,-0.00944026603035641,0.00525937887124024));
#24741=CARTESIAN_POINT('',(0.012,-0.0064497848202166,0.0087546645722668));
#24742=CARTESIAN_POINT('Origin',(0.012,0.,0.));
#24743=CARTESIAN_POINT('Origin',(0.012,-0.00322869527523151,0.0103128665100857));
#24744=CARTESIAN_POINT('',(0.012,-0.00725930527113401,0.00809607083593554));
#24745=CARTESIAN_POINT('Origin',(0.012,-0.0100684908803427,0.00392494334068737));
#24746=CARTESIAN_POINT('',(0.012,-0.00758180451511425,0.00779487756764615));
#24747=CARTESIAN_POINT('Origin',(0.012,0.,0.));
#24748=CARTESIAN_POINT('Origin',(0.012,-0.000326588410304044,0.0108015290049791));
#24749=CARTESIAN_POINT('',(0.012,-0.00480581676911598,0.0097543836905098));
#24750=CARTESIAN_POINT('Origin',(0.012,-0.0086361868858939,0.00649584212454889));
#24751=CARTESIAN_POINT('',(0.012,-0.00519761783757985,0.00955136874036762));
#24752=CARTESIAN_POINT('Origin',(0.012,0.,0.));
#24753=CARTESIAN_POINT('Origin',(0.012,-0.00707005305261656,0.00817276199753406));
#24754=CARTESIAN_POINT('',(0.012,-0.00988380028027131,0.00453369253696241));
#24755=CARTESIAN_POINT('Origin',(0.012,-0.0107986353290695,-0.000411295349988447));
#24756=CARTESIAN_POINT('',(0.012,-0.0100596045052361,0.00412895061707371));
#24757=CARTESIAN_POINT('Origin',(0.012,0.,0.));
#24758=CARTESIAN_POINT('Origin',(0.012,-0.00589134458189312,0.00905934588436428));
#24759=CARTESIAN_POINT('',(0.012,-0.0091744043103039,0.00583730944451955));
#24760=CARTESIAN_POINT('Origin',(0.012,-0.0107540609664773,0.00106294946466809));
#24761=CARTESIAN_POINT('',(0.012,-0.00940368343621036,0.00546027598492447));
#24762=CARTESIAN_POINT('Origin',(0.012,0.,0.));
#24763=CARTESIAN_POINT('Origin',(0.012,-0.00460289150846104,0.00977717129830948));
#24764=CARTESIAN_POINT('',(0.012,-0.00829410654667511,0.00703218832173891));
#24765=CARTESIAN_POINT('Origin',(0.012,-0.0105091587955445,0.00251739354197548));
#24766=CARTESIAN_POINT('',(0.012,-0.00857258953722036,0.006689886742415));
#24767=CARTESIAN_POINT('Origin',(0.012,0.,0.));
#24768=CARTESIAN_POINT('Origin',(0.012,-0.00811705981202384,0.00713393501814931));
#24769=CARTESIAN_POINT('',(0.012,-0.0104090797518856,0.00314562151551737));
#24770=CARTESIAN_POINT('Origin',(0.012,-0.0106420515472837,-0.00187787851047538));
#24771=CARTESIAN_POINT('',(0.012,-0.010528134175832,0.00272071071150145));
#24772=CARTESIAN_POINT('Origin',(0.012,0.,0.));
#24773=CARTESIAN_POINT('Origin',(0.012,-0.00901286110520009,0.00596221632729986));
#24774=CARTESIAN_POINT('',(0.012,-0.0107404577624574,0.00169895351698271));
#24775=CARTESIAN_POINT('Origin',(0.012,-0.0102872264807069,-0.00330948034739476));
#24776=CARTESIAN_POINT('',(0.012,-0.0108005446267269,0.00126178911315627));
#24777=CARTESIAN_POINT('Origin',(0.012,0.,0.));
#24778=CARTESIAN_POINT('Origin',(0.012,-0.00974076984897455,0.00467943282721932));
#24779=CARTESIAN_POINT('',(0.012,-0.0108717613666412,0.000220637228970165));
#24780=CARTESIAN_POINT('Origin',(0.012,-0.00974076984897448,-0.00467943282721946));
#24781=CARTESIAN_POINT('',(0.012,-0.0108717613666412,-0.000220637228970318));
#24782=CARTESIAN_POINT('Origin',(0.012,0.,0.));
#24783=CARTESIAN_POINT('Origin',(0.012,0.0106420515472837,-0.00187787851047532));
#24784=CARTESIAN_POINT('',(0.012,0.010528134175832,0.00272071071150152));
#24785=CARTESIAN_POINT('Origin',(0.012,0.00811705981202379,0.00713393501814937));
#24786=CARTESIAN_POINT('',(0.012,0.0104090797518855,0.00314562151551744));
#24787=CARTESIAN_POINT('Origin',(0.012,0.,0.));
#24788=CARTESIAN_POINT('Origin',(0.012,0.0107986353290695,-0.000411295349988374));
#24789=CARTESIAN_POINT('',(0.012,0.0100596045052361,0.00412895061707378));
#24790=CARTESIAN_POINT('Origin',(0.012,0.0070700530526165,0.00817276199753411));
#24791=CARTESIAN_POINT('',(0.012,0.00988380028027128,0.00453369253696249));
#24792=CARTESIAN_POINT('Origin',(0.012,0.,0.));
#24793=CARTESIAN_POINT('Origin',(0.012,0.0105091587955444,0.00251739354197556));
#24794=CARTESIAN_POINT('',(0.012,0.00857258953722032,0.00668988674241506));
#24795=CARTESIAN_POINT('Origin',(0.012,0.00460289150846097,0.00977717129830952));
#24796=CARTESIAN_POINT('',(0.012,0.00829410654667506,0.00703218832173896));
#24797=CARTESIAN_POINT('Origin',(0.012,0.,0.));
#24798=CARTESIAN_POINT('Origin',(0.012,0.0100684908803426,0.00392494334068744));
#24799=CARTESIAN_POINT('',(0.012,0.00758180451511419,0.00779487756764621));
#24800=CARTESIAN_POINT('Origin',(0.012,0.00322869527523144,0.0103128665100857));
#24801=CARTESIAN_POINT('',(0.012,0.00725930527113395,0.00809607083593559));
#24802=CARTESIAN_POINT('Origin',(0.012,0.,0.));
#24803=CARTESIAN_POINT('Origin',(0.012,0.0107540609664773,0.00106294946466816));
#24804=CARTESIAN_POINT('',(0.012,0.00940368343621032,0.00546027598492453));
#24805=CARTESIAN_POINT('Origin',(0.012,0.00589134458189306,0.00905934588436432));
#24806=CARTESIAN_POINT('',(0.012,0.00917440431030386,0.00583730944451961));
#24807=CARTESIAN_POINT('Origin',(0.012,0.,0.));
#24808=CARTESIAN_POINT('Origin',(0.012,0.00767123192004022,0.00761130012968254));
#24809=CARTESIAN_POINT('',(0.012,0.00384862906889953,0.0101701489807191));
#24810=CARTESIAN_POINT('Origin',(0.012,-0.00114726146149743,0.0107453934304013));
#24811=CARTESIAN_POINT('',(0.012,0.00343283339125305,0.0103179228000552));
#24812=CARTESIAN_POINT('Origin',(0.012,0.,0.));
#24813=CARTESIAN_POINT('Origin',(0.012,0.00863618688589385,0.00649584212454895));
#24814=CARTESIAN_POINT('',(0.012,0.00519761783757978,0.00955136874036766));
#24815=CARTESIAN_POINT('Origin',(0.012,0.00032658841030397,0.0108015290049791));
#24816=CARTESIAN_POINT('',(0.012,0.00480581676911591,0.00975438369050984));
#24817=CARTESIAN_POINT('Origin',(0.012,0.,0.));
#24818=CARTESIAN_POINT('Origin',(0.012,0.00944026603035638,0.00525937887124031));
#24819=CARTESIAN_POINT('',(0.012,0.00644978482021654,0.00875466457226685));
#24820=CARTESIAN_POINT('Origin',(0.012,0.00179435455795041,0.0106564525314718));
#24821=CARTESIAN_POINT('',(0.012,0.00608927687352466,0.00900913886881303));
#24822=CARTESIAN_POINT('Origin',(0.012,0.,0.));
#24823=CARTESIAN_POINT('Origin',(0.012,0.00656337641804445,0.00858497401453304));
#24824=CARTESIAN_POINT('',(0.012,0.00242794762255152,0.0105994785882206));
#24825=CARTESIAN_POINT('Origin',(0.012,-0.00259974002297318,0.0104890915072804));
#24826=CARTESIAN_POINT('',(0.012,0.00199590282248136,0.0106892585300951));
#24827=CARTESIAN_POINT('Origin',(0.012,0.,0.));
#24828=CARTESIAN_POINT('Origin',(0.012,0.00533325763176559,0.00939872607688742));
#24829=CARTESIAN_POINT('',(0.012,0.000962038105848705,0.0108313599646072));
#24830=CARTESIAN_POINT('Origin',(0.012,-0.00400379034671796,0.010037397655502));
#24831=CARTESIAN_POINT('',(0.012,0.000521792360520001,0.0108614735985732));
#24832=CARTESIAN_POINT('Origin',(0.012,0.,0.));
#24833=CARTESIAN_POINT('Origin',(0.012,0.00400379034671789,0.010037397655502));
#24834=CARTESIAN_POINT('',(0.012,-0.000521792360520078,0.0108614735985732));
#24835=CARTESIAN_POINT('Origin',(0.012,-0.00533325763176565,0.00939872607688738));
#24836=CARTESIAN_POINT('',(0.012,-0.000962038105848782,0.0108313599646072));
#24837=CARTESIAN_POINT('Origin',(0.012,0.,0.));
#24838=CARTESIAN_POINT('Origin',(0.0500000508,0.,0.));
#24839=CARTESIAN_POINT('',(0.0500000508,-1.10218211923262E-18,-0.009));
#24840=CARTESIAN_POINT('',(0.,0.,0.));
#24841=CARTESIAN_POINT('Ctrl Pts',(-0.180492715511507,0.00208357847138839,
0.00778381458262853));
#24842=CARTESIAN_POINT('Ctrl Pts',(-0.18,0.00208768551873161,0.00777792629190908));
#24843=CARTESIAN_POINT('Ctrl Pts',(-0.18,0.00236958913814357,0.00737375990977421));
#24844=CARTESIAN_POINT('Ctrl Pts',(-0.180494324020048,0.00106537901854582,
0.00707337168038232));
#24845=CARTESIAN_POINT('Ctrl Pts',(-0.18,0.00106751218715109,0.00706776299687777));
#24846=CARTESIAN_POINT('Ctrl Pts',(-0.18,0.0014052360688775,0.00670086601600097));
#24847=CARTESIAN_POINT('Ctrl Pts',(-0.180498282439035,-0.000688149212900568,
0.00524596704164286));
#24848=CARTESIAN_POINT('Ctrl Pts',(-0.18,-0.000692161918799494,0.00523579826232968));
#24849=CARTESIAN_POINT('Ctrl Pts',(-0.18,-0.000255396373108266,0.00497022946835977));
#24850=CARTESIAN_POINT('Ctrl Pts',(-0.180508571884256,-0.00206121245391611,
0.00171196042612565));
#24851=CARTESIAN_POINT('Ctrl Pts',(-0.18,-0.00207089065980965,0.0017061119940659));
#24852=CARTESIAN_POINT('Ctrl Pts',(-0.18,-0.00155636923028695,0.001622484125152));
#24853=CARTESIAN_POINT('Ctrl Pts',(-0.180507701632299,-0.00198984920249958,
-0.00207534072170255));
#24854=CARTESIAN_POINT('Ctrl Pts',(-0.18,-0.00199898872775875,-0.00206848014615668));
#24855=CARTESIAN_POINT('Ctrl Pts',(-0.18,-0.0014886043286521,-0.00196703616742313));
#24856=CARTESIAN_POINT('Ctrl Pts',(-0.180497559880866,-0.000482912630366871,
-0.00555392798696781));
#24857=CARTESIAN_POINT('Ctrl Pts',(-0.18,-0.000486526972169703,-0.00554405840433583));
#24858=CARTESIAN_POINT('Ctrl Pts',(-0.18,-6.11665353613021E-5,-0.00526163542994926));
#24859=CARTESIAN_POINT('Ctrl Pts',(-0.180491867056987,0.00224576313070539,
-0.0081898374281038));
#24860=CARTESIAN_POINT('Ctrl Pts',(-0.18,0.00224601031558402,-0.00818083867958575));
#24861=CARTESIAN_POINT('Ctrl Pts',(-0.18,0.00252313449484398,-0.00775830380791825));
#24862=CARTESIAN_POINT('Ctrl Pts',(-0.180488462887617,0.00577942932125372,
-0.00958054386633694));
#24863=CARTESIAN_POINT('Ctrl Pts',(-0.18,0.00577937831377157,-0.00956893262499887));
#24864=CARTESIAN_POINT('Ctrl Pts',(-0.18,0.00587025317906997,-0.00907572435223234));
#24865=CARTESIAN_POINT('Ctrl Pts',(-0.180488629342552,0.00957710911122243,
-0.00950944489475148));
#24866=CARTESIAN_POINT('Ctrl Pts',(-0.18,0.00957712259305036,-0.00949788380666547));
#24867=CARTESIAN_POINT('Ctrl Pts',(-0.18,0.0094675316846421,-0.00900837007444288));
#24868=CARTESIAN_POINT('Ctrl Pts',(-0.180492343722264,0.0130567083237039,
-0.00798771374964044));
#24869=CARTESIAN_POINT('Ctrl Pts',(-0.18,0.0130566470856787,-0.00797903414015096));
#24870=CARTESIAN_POINT('Ctrl Pts',(-0.18,0.0127633603172519,-0.00756679005675688));
#24871=CARTESIAN_POINT('Ctrl Pts',(-0.180498277776074,0.0156878479525759,
-0.00524728696109442));
#24872=CARTESIAN_POINT('Ctrl Pts',(-0.18,0.0156918696359066,-0.00523708434816095));
#24873=CARTESIAN_POINT('Ctrl Pts',(-0.18,0.0152551103542225,-0.00497147978047479));
#24874=CARTESIAN_POINT('Ctrl Pts',(-0.180508590057067,0.0170631420237172,
-0.00170670572622402));
#24875=CARTESIAN_POINT('Ctrl Pts',(-0.18,0.0170728417288127,-0.00170085628138549));
#24876=CARTESIAN_POINT('Ctrl Pts',(-0.18,0.0165581992152197,-0.00161750652259339));
#24877=CARTESIAN_POINT('Ctrl Pts',(-0.180507676294974,0.0169879516360366,
0.00208672420876621));
#24878=CARTESIAN_POINT('Ctrl Pts',(-0.18,0.0169970776392087,0.00207981994539201));
#24879=CARTESIAN_POINT('Ctrl Pts',(-0.18,0.0164868018720009,0.00197783354485042));
#24880=CARTESIAN_POINT('Ctrl Pts',(-0.180497532146321,0.0154750030588555,
0.00556552633006958));
#24881=CARTESIAN_POINT('Ctrl Pts',(-0.18,0.0154786081176936,0.00555565825322737));
#24882=CARTESIAN_POINT('Ctrl Pts',(-0.18,0.0150536805229185,0.00527261080601529));
#24883=CARTESIAN_POINT('Ctrl Pts',(-0.180491851706073,0.0127430969971975,
0.00819641820051746));
#24884=CARTESIAN_POINT('Ctrl Pts',(-0.18,0.0127428333825127,0.00818741797918455));
#24885=CARTESIAN_POINT('Ctrl Pts',(-0.18,0.01246631245657,0.00776454042759482));
#24886=CARTESIAN_POINT('Ctrl Pts',(-0.180488461754297,0.00921325615876769,
0.00958099954636007));
#24887=CARTESIAN_POINT('Ctrl Pts',(-0.18,0.00921330243936221,0.00956938959009847));
#24888=CARTESIAN_POINT('Ctrl Pts',(-0.18,0.00912281682762101,0.00907615564159787));
#24889=CARTESIAN_POINT('Ctrl Pts',(-0.18048863138779,0.00542104750415485,
0.00950862445512012));
#24890=CARTESIAN_POINT('Ctrl Pts',(-0.18,0.00542103959480098,0.00949706815102514));
#24891=CARTESIAN_POINT('Ctrl Pts',(-0.18,0.00553072204248816,0.00900759283099922));
#24892=CARTESIAN_POINT('Ctrl Pts',(-0.180491107002967,0.00310177792423096,
0.00849425748487474));
#24893=CARTESIAN_POINT('Ctrl Pts',(-0.18,0.00310463170987884,0.00848584310919716));
#24894=CARTESIAN_POINT('Ctrl Pts',(-0.18,0.00333394220740964,0.00804665380354745));
#24895=CARTESIAN_POINT('Ctrl Pts',(-0.180492715511507,0.00208357847138839,
0.00778381458262853));
#24896=CARTESIAN_POINT('Ctrl Pts',(-0.18,0.00208768551873161,0.00777792629190908));
#24897=CARTESIAN_POINT('Ctrl Pts',(-0.18,0.00236958913814357,0.00737375990977421));
#24898=CARTESIAN_POINT('',(-0.180000000092441,0.002369415201346,0.00737400928367846));
#24899=CARTESIAN_POINT('',(-0.180492713748997,0.00208357848608163,0.00778381456156277));
#24900=CARTESIAN_POINT('Ctrl Pts',(-0.180000000092441,0.002369415201346,
0.00737400928367846));
#24901=CARTESIAN_POINT('Ctrl Pts',(-0.180000299553135,0.00208768401511753,
0.0077779284476468));
#24902=CARTESIAN_POINT('Ctrl Pts',(-0.180492713748996,0.00208357848608164,
0.00778381456156275));
#24903=CARTESIAN_POINT('',(-0.180000000073866,0.00163303568495152,0.0068004616007287));
#24904=CARTESIAN_POINT('Ctrl Pts',(-0.180000000073866,0.00163303568495152,
0.0068004616007287));
#24905=CARTESIAN_POINT('Ctrl Pts',(-0.180000000059821,0.00118804839875416,
0.00641493294655719));
#24906=CARTESIAN_POINT('Ctrl Pts',(-0.18,0.000780603533896183,0.00598502981387675));
#24907=CARTESIAN_POINT('Ctrl Pts',(-0.18,0.000418942701838473,0.00551967293650249));
#24908=CARTESIAN_POINT('Ctrl Pts',(-0.18,0.000249927081888821,0.0053021968535113));
#24909=CARTESIAN_POINT('Ctrl Pts',(-0.18,9.09590595398255E-5,0.00507695666847608));
#24910=CARTESIAN_POINT('Ctrl Pts',(-0.18,-5.70670721416072E-5,0.00484493104806877));
#24911=CARTESIAN_POINT('Ctrl Pts',(-0.18,-6.74294721945815E-5,0.00482868835987657));
#24912=CARTESIAN_POINT('Ctrl Pts',(-0.18,-7.77382685084171E-5,0.00481241242995712));
#24913=CARTESIAN_POINT('Ctrl Pts',(-0.18,-8.79933143911442E-5,0.00479610367742078));
#24914=CARTESIAN_POINT('Ctrl Pts',(-0.18,-0.000244740945435163,0.00454682558012237));
#24915=CARTESIAN_POINT('Ctrl Pts',(-0.179999999906675,-0.000388909840019564,
0.00428990581472337));
#24916=CARTESIAN_POINT('Ctrl Pts',(-0.180000000093167,-0.00052030903126298,
0.00402694496455378));
#24917=CARTESIAN_POINT('Ctrl Pts',(-0.180000000279659,-0.000651708222506395,
0.00376398411438418));
#24918=CARTESIAN_POINT('Ctrl Pts',(-0.18000000050776,-0.000769903124688603,
0.00349473306770954));
#24919=CARTESIAN_POINT('Ctrl Pts',(-0.180000000457489,-0.000874579938457122,
0.00322047030539096));
#24920=CARTESIAN_POINT('Ctrl Pts',(-0.180000000360256,-0.00107704602882691,
0.00268999075388821));
#24921=CARTESIAN_POINT('Ctrl Pts',(-0.180000000153618,-0.00122935539601011,
0.00214080127837629));
#24922=CARTESIAN_POINT('Ctrl Pts',(-0.180000000091491,-0.00132854406997328,
0.00158224127209026));
#24923=CARTESIAN_POINT('Ctrl Pts',(-0.180000000057257,-0.00138319974100772,
0.00127445943837102));
#24924=CARTESIAN_POINT('Ctrl Pts',(-0.18000000004624,-0.00142172317863241,
0.000963827247457888));
#24925=CARTESIAN_POINT('Ctrl Pts',(-0.180000000066894,-0.00144417813514861,
0.000651961194282699));
#24926=CARTESIAN_POINT('Ctrl Pts',(-0.180000000123781,-0.00150602452449947,
-0.000206993457269628));
#24927=CARTESIAN_POINT('Ctrl Pts',(-0.180000000048164,-0.00144517176436833,
-0.0010756726768805));
#24928=CARTESIAN_POINT('Ctrl Pts',(-0.180000000134111,-0.0012623500650625,
-0.00191796030930795));
#24929=CARTESIAN_POINT('Ctrl Pts',(-0.180000000165279,-0.00119605058425185,
-0.00222341219458856));
#24930=CARTESIAN_POINT('Ctrl Pts',(-0.180000000216682,-0.00111371887405417,
-0.00252539704694802));
#24931=CARTESIAN_POINT('Ctrl Pts',(-0.180000000371265,-0.00101602267705604,
-0.00282231615756755));
#24932=CARTESIAN_POINT('Ctrl Pts',(-0.180000000516477,-0.000924248987460435,
-0.00310123553345199));
#24933=CARTESIAN_POINT('Ctrl Pts',(-0.180000000323103,-0.0008186164521681,
-0.00337562307708563));
#24934=CARTESIAN_POINT('Ctrl Pts',(-0.180000000193685,-0.000699874970982025,
-0.00364426841946957));
#24935=CARTESIAN_POINT('Ctrl Pts',(-0.17999999994348,-0.000470313038758882,
-0.00416363825774677));
#24936=CARTESIAN_POINT('Ctrl Pts',(-0.180000000003078,-0.000191886024868714,
-0.0046617027692084));
#24937=CARTESIAN_POINT('Ctrl Pts',(-0.180000000003089,0.00013159832191248,
-0.00512867861339497));
#24938=CARTESIAN_POINT('Ctrl Pts',(-0.180000000003096,0.000310083227245415,
-0.00538633602455492));
#24939=CARTESIAN_POINT('Ctrl Pts',(-0.180000000005194,0.000502280903413068,
-0.00563452896521551));
#24940=CARTESIAN_POINT('Ctrl Pts',(-0.180000000017907,0.000706915973500765,
-0.00587200864424154));
#24941=CARTESIAN_POINT('Ctrl Pts',(-0.180000000029826,0.000898753882513541,
-0.00609463717530347));
#24942=CARTESIAN_POINT('Ctrl Pts',(-0.180000000008953,0.00110165204133482,
-0.00630779073382734));
#24943=CARTESIAN_POINT('Ctrl Pts',(-0.180000000005369,0.00131446604763071,
-0.00651061213963826));
#24944=CARTESIAN_POINT('Ctrl Pts',(-0.179999999998451,0.00172518580215862,
-0.00690204670476666));
#24945=CARTESIAN_POINT('Ctrl Pts',(-0.179999999991229,0.00217302812516551,
-0.00725489163512563));
#24946=CARTESIAN_POINT('Ctrl Pts',(-0.180000000010711,0.00265021480579363,
-0.00756184956024018));
#24947=CARTESIAN_POINT('Ctrl Pts',(-0.180000000021513,0.00291478944637761,
-0.00773204140759998));
#24948=CARTESIAN_POINT('Ctrl Pts',(-0.180000000040581,0.00318838199463977,
-0.00788813229953453));
#24949=CARTESIAN_POINT('Ctrl Pts',(-0.180000000141286,0.00346927698327818,
-0.00802948180824356));
#24950=CARTESIAN_POINT('Ctrl Pts',(-0.180000000235397,0.00373178266338216,
-0.0081615776106496));
#24951=CARTESIAN_POINT('Ctrl Pts',(-0.180000000150774,0.00400081715481969,
-0.00828058078675498));
#24952=CARTESIAN_POINT('Ctrl Pts',(-0.18000000009043,0.00427498444480135,
-0.00838619566190851));
#24953=CARTESIAN_POINT('Ctrl Pts',(-0.179999999973844,0.00480469075812819,
-0.00859024942103415));
#24954=CARTESIAN_POINT('Ctrl Pts',(-0.17999999998725,0.00535362645522928,
-0.00874446366426804));
#24955=CARTESIAN_POINT('Ctrl Pts',(-0.180000000024732,0.00591191863550963,
-0.00884508332764294));
#24956=CARTESIAN_POINT('Ctrl Pts',(-0.18000000004545,0.00622051505123686,
-0.00890070092102134));
#24957=CARTESIAN_POINT('Ctrl Pts',(-0.180000000083345,0.00653197023768919,
-0.00893994792029853));
#24958=CARTESIAN_POINT('Ctrl Pts',(-0.180000000289389,0.00684450224324547,
-0.00896290263578175));
#24959=CARTESIAN_POINT('Ctrl Pts',(-0.180000000482325,0.00713715030794149,
-0.00898439692418225));
#24960=CARTESIAN_POINT('Ctrl Pts',(-0.180000000600894,0.00743078154821022,
-0.00899143359818871));
#24961=CARTESIAN_POINT('Ctrl Pts',(-0.18000000053753,0.00772406620072347,
-0.0089840730882348));
#24962=CARTESIAN_POINT('Ctrl Pts',(-0.180000000414596,0.00829307322193137,
-0.00896979282567229));
#24963=CARTESIAN_POINT('Ctrl Pts',(-0.180000000392808,0.00886085876197087,
-0.00890178007901912));
#24964=CARTESIAN_POINT('Ctrl Pts',(-0.180000000358353,0.00941741794215845,
-0.00877991725364757));
#24965=CARTESIAN_POINT('Ctrl Pts',(-0.180000000339531,0.00972146465792907,
-0.00871334393467678));
#24966=CARTESIAN_POINT('Ctrl Pts',(-0.180000000318419,0.0100221583669829,
-0.00863069319347393));
#24967=CARTESIAN_POINT('Ctrl Pts',(-0.180000000285255,0.0103179911779754,
-0.00853255598738525));
#24968=CARTESIAN_POINT('Ctrl Pts',(-0.180000000222673,0.0108762287736087,
-0.00834737072079723));
#24969=CARTESIAN_POINT('Ctrl Pts',(-0.18,0.0114171707809986,-0.00810658998512941));
#24970=CARTESIAN_POINT('Ctrl Pts',(-0.18,0.0119298368797898,-0.00781556806782665));
#24971=CARTESIAN_POINT('Ctrl Pts',(-0.18,0.0121696484903194,-0.0076794357297369));
#24972=CARTESIAN_POINT('Ctrl Pts',(-0.18,0.0124032195712773,-0.00753222783046099));
#24973=CARTESIAN_POINT('Ctrl Pts',(-0.18,0.0126293472179787,-0.0073745016803242));
#24974=CARTESIAN_POINT('Ctrl Pts',(-0.18,0.0126449259219565,-0.00736363538848248));
#24975=CARTESIAN_POINT('Ctrl Pts',(-0.18,0.0126604693095513,-0.00735271919189223));
#24976=CARTESIAN_POINT('Ctrl Pts',(-0.18,0.0126759770760497,-0.00734175340323608));
#24977=CARTESIAN_POINT('Ctrl Pts',(-0.18,0.0129165828191756,-0.00717161725056425));
#24978=CARTESIAN_POINT('Ctrl Pts',(-0.179999999946229,0.0131485905079609,
-0.00698955702291025));
#24979=CARTESIAN_POINT('Ctrl Pts',(-0.180000000053711,0.0133711230714489,
-0.00679686694357883));
#24980=CARTESIAN_POINT('Ctrl Pts',(-0.180000000161193,0.013593655634937,
-0.00660417686424741));
#24981=CARTESIAN_POINT('Ctrl Pts',(-0.18000000018702,0.0138064196112521,
-0.00640048280567611));
#24982=CARTESIAN_POINT('Ctrl Pts',(-0.180000000112277,0.0140085963705019,
-0.00618691252231924));
#24983=CARTESIAN_POINT('Ctrl Pts',(-0.179999999967716,0.0143996253669064,
-0.00577384737144471));
#24984=CARTESIAN_POINT('Ctrl Pts',(-0.179999999997186,0.0147514853889812,
-0.00532407927780652));
#24985=CARTESIAN_POINT('Ctrl Pts',(-0.180000000012131,0.0150570930156507,
-0.00484509518207374));
#24986=CARTESIAN_POINT('Ctrl Pts',(-0.180000000020367,0.0152255174438687,
-0.00458112067551943));
#24987=CARTESIAN_POINT('Ctrl Pts',(-0.180000000036385,0.0153798945654668,
-0.00430827187588287));
#24988=CARTESIAN_POINT('Ctrl Pts',(-0.18000000012645,0.0155196673863458,
-0.00402817957933301));
#24989=CARTESIAN_POINT('Ctrl Pts',(-0.180000000210945,0.0156507980032042,
-0.00376540549068789));
#24990=CARTESIAN_POINT('Ctrl Pts',(-0.180000000145609,0.0157688706720626,
-0.00349613328218849));
#24991=CARTESIAN_POINT('Ctrl Pts',(-0.180000000087433,0.0158735896851957,
-0.00322174217319132));
#24992=CARTESIAN_POINT('Ctrl Pts',(-0.179999999974608,0.0160766802466698,
-0.00268959196739333));
#24993=CARTESIAN_POINT('Ctrl Pts',(-0.179999999994891,0.0162297495161568,
-0.00213813714056621));
#24994=CARTESIAN_POINT('Ctrl Pts',(-0.180000000013797,0.0163292338388839,
-0.00157729922827135));
#24995=CARTESIAN_POINT('Ctrl Pts',(-0.180000000024137,0.0163836399779672,
-0.00127058733012421));
#24996=CARTESIAN_POINT('Ctrl Pts',(-0.180000000043723,0.0164220223554685,
-0.000961069827483446));
#24997=CARTESIAN_POINT('Ctrl Pts',(-0.180000000149483,0.016444429808688,
-0.000650446720184491));
#24998=CARTESIAN_POINT('Ctrl Pts',(-0.180000000443122,0.0165066437688952,
0.000211993711915339));
#24999=CARTESIAN_POINT('Ctrl Pts',(-0.180000000296702,0.0164447645933107,
0.00108345095688852));
#25000=CARTESIAN_POINT('Ctrl Pts',(-0.180000000268535,0.0162603541706888,
0.0019278501776853));
#25001=CARTESIAN_POINT('Ctrl Pts',(-0.180000000258442,0.016194273293351,
0.0022304287442339));
#25002=CARTESIAN_POINT('Ctrl Pts',(-0.180000000268355,0.016112459702564,
0.00252954106943733));
#25003=CARTESIAN_POINT('Ctrl Pts',(-0.18000000035993,0.0160155755183459,
0.00282367481902353));
#25004=CARTESIAN_POINT('Ctrl Pts',(-0.180000000446714,0.0159237613421876,
0.00310241637128562));
#25005=CARTESIAN_POINT('Ctrl Pts',(-0.180000000236453,0.0158181267106129,
0.00337660925175313));
#25006=CARTESIAN_POINT('Ctrl Pts',(-0.180000000141743,0.0156994560460536,
0.00364506614002243));
#25007=CARTESIAN_POINT('Ctrl Pts',(-0.179999999957256,0.0154682929609363,
0.00416800348720764));
#25008=CARTESIAN_POINT('Ctrl Pts',(-0.180000000001891,0.0151875969475736,
0.00466925202736088));
#25009=CARTESIAN_POINT('Ctrl Pts',(-0.180000000003811,0.0148613567562351,
0.00513883810306275));
#25010=CARTESIAN_POINT('Ctrl Pts',(-0.180000000004847,0.0146851576377794,
0.00539245692371836));
#25011=CARTESIAN_POINT('Ctrl Pts',(-0.180000000008273,0.0144956778303638,
0.005636840304416));
#25012=CARTESIAN_POINT('Ctrl Pts',(-0.180000000027596,0.014294151952822,
0.00587080597888225));
#25013=CARTESIAN_POINT('Ctrl Pts',(-0.180000000045963,0.014102598737904,
0.00609319368249218));
#25014=CARTESIAN_POINT('Ctrl Pts',(-0.180000000030252,0.0139000517862225,
0.00630612585062232));
#25015=CARTESIAN_POINT('Ctrl Pts',(-0.18000000001814,0.0136875780978067,
0.00650871390624616));
#25016=CARTESIAN_POINT('Ctrl Pts',(-0.179999999994542,0.0132736146987159,
0.00690341708453866));
#25017=CARTESIAN_POINT('Ctrl Pts',(-0.179999999993531,0.0128219471861013,
0.00725894839754447));
#25018=CARTESIAN_POINT('Ctrl Pts',(-0.180000000009742,0.0123403444657045,
0.00756790445316537));
#25019=CARTESIAN_POINT('Ctrl Pts',(-0.180000000018493,0.0120803750574165,
0.00773467909866692));
#25020=CARTESIAN_POINT('Ctrl Pts',(-0.180000000034388,0.0118116845160434,
0.00788788425791664));
#25021=CARTESIAN_POINT('Ctrl Pts',(-0.180000000114831,0.0115358336793546,
0.00802690888367712));
#25022=CARTESIAN_POINT('Ctrl Pts',(-0.180000000191321,0.0112735421870466,
0.00815909980611903));
#25023=CARTESIAN_POINT('Ctrl Pts',(-0.180000000129546,0.0110046518767973,
0.00827827701382785));
#25024=CARTESIAN_POINT('Ctrl Pts',(-0.180000000077698,0.0107305462975331,
0.00838407719408214));
#25025=CARTESIAN_POINT('Ctrl Pts',(-0.179999999976826,0.0101972512619832,
0.00858992017999054));
#25026=CARTESIAN_POINT('Ctrl Pts',(-0.179999999991605,0.0096441953899426,
0.00874529488330738));
#25027=CARTESIAN_POINT('Ctrl Pts',(-0.180000000019558,0.0090814082947659,
0.00884626362895226));
#25028=CARTESIAN_POINT('Ctrl Pts',(-0.180000000034707,0.00877640323489228,
0.00890098410597584));
#25029=CARTESIAN_POINT('Ctrl Pts',(-0.180000000063481,0.00846854136355709,
0.00893972891457769));
#25030=CARTESIAN_POINT('Ctrl Pts',(-0.180000000199897,0.00815953756376133,
0.00896253601849186));
#25031=CARTESIAN_POINT('Ctrl Pts',(-0.180000000329273,0.00786648114315136,
0.00898416607042646));
#25032=CARTESIAN_POINT('Ctrl Pts',(-0.180000000237125,0.00757234589332953,
0.00899118671439754));
#25033=CARTESIAN_POINT('Ctrl Pts',(-0.180000000142269,0.00727854544340191,
0.00898381724086646));
#25034=CARTESIAN_POINT('Ctrl Pts',(-0.179999999957967,0.00670769761841669,
0.00896949851556314));
#25035=CARTESIAN_POINT('Ctrl Pts',(-0.179999999987481,0.0061380290887039,
0.00890113003428405));
#25036=CARTESIAN_POINT('Ctrl Pts',(-0.180000000028244,0.00558017359327183,
0.00877894937833312));
#25037=CARTESIAN_POINT('Ctrl Pts',(-0.18000000005042,0.0052766881758777,
0.00871248046716817));
#25038=CARTESIAN_POINT('Ctrl Pts',(-0.180000000091846,0.00497669798505343,
0.00863008892616214));
#25039=CARTESIAN_POINT('Ctrl Pts',(-0.180000000311714,0.0046817845363248,
0.00853248488801863));
#25040=CARTESIAN_POINT('Ctrl Pts',(-0.180000000519721,0.00440278044521801,
0.00844014618299184));
#25041=CARTESIAN_POINT('Ctrl Pts',(-0.180000000511612,0.00412836853147088,
0.00833392835474274));
#25042=CARTESIAN_POINT('Ctrl Pts',(-0.180000000373709,0.00385978342259457,
0.00821449183257972));
#25043=CARTESIAN_POINT('Ctrl Pts',(-0.180000000105832,0.00333805554982461,
0.00798248581072742));
#25044=CARTESIAN_POINT('Ctrl Pts',(-0.18000000010862,0.00283804754615616,
0.00770103805887969));
#25045=CARTESIAN_POINT('Ctrl Pts',(-0.180000000092441,0.002369415201346,
0.00737400928367846));
#25046=CARTESIAN_POINT('',(-0.180494077221453,0.00130607217168702,0.00717829214732416));
#25047=CARTESIAN_POINT('Ctrl Pts',(-0.180000000073866,0.00163303568495152,
0.0068004616007287));
#25048=CARTESIAN_POINT('Ctrl Pts',(-0.180000268510106,0.00130973850057992,
0.00717346067102031));
#25049=CARTESIAN_POINT('Ctrl Pts',(-0.180494077221453,0.00130607217168702,
0.00717829214732417));
#25050=CARTESIAN_POINT('',(-0.180505050469422,0.0166467264643195,0.00245334977916771));
#25051=CARTESIAN_POINT('Ctrl Pts',(-0.180505050469422,0.0166467264643195,
0.0024533497791677));
#25052=CARTESIAN_POINT('Ctrl Pts',(-0.180505306133657,0.0166837724953881,
0.00231446224061256));
#25053=CARTESIAN_POINT('Ctrl Pts',(-0.180505550682239,0.0167176593319398,
0.00217472825564444));
#25054=CARTESIAN_POINT('Ctrl Pts',(-0.180505778846172,0.0167483294518472,
0.00203428715171698));
#25055=CARTESIAN_POINT('Ctrl Pts',(-0.180507226251443,0.016942891723494,
0.00114336985842741));
#25056=CARTESIAN_POINT('Ctrl Pts',(-0.180508014307505,0.0170079758680575,
0.000223993120464905));
#25057=CARTESIAN_POINT('Ctrl Pts',(-0.18050756952682,0.0169427469804377,
-0.000685980192934213));
#25058=CARTESIAN_POINT('Ctrl Pts',(-0.180507409214296,0.0169192364999648,
-0.00101396232778566));
#25059=CARTESIAN_POINT('Ctrl Pts',(-0.180507095715993,0.0168787986842539,
-0.00134074577739527));
#25060=CARTESIAN_POINT('Ctrl Pts',(-0.180506641320586,0.0168213956365477,
-0.00166456445752732));
#25061=CARTESIAN_POINT('Ctrl Pts',(-0.180505382372451,0.016662354724553,
-0.00256173665076423));
#25062=CARTESIAN_POINT('Ctrl Pts',(-0.180503042799424,0.016373071623164,
-0.00343614135643362));
#25063=CARTESIAN_POINT('Ctrl Pts',(-0.180501039464594,0.0159665378030119,
-0.00425159980508381));
#25064=CARTESIAN_POINT('Ctrl Pts',(-0.18050031302138,0.0158191217393433,
-0.00454729888010876));
#25065=CARTESIAN_POINT('Ctrl Pts',(-0.180499580110058,0.0156562625227054,
-0.00483530720101641));
#25066=CARTESIAN_POINT('Ctrl Pts',(-0.180498891082393,0.0154785401533995,
-0.00511392775516268));
#25067=CARTESIAN_POINT('Ctrl Pts',(-0.180496994130169,0.0149892552365115,
-0.00588099402381038));
#25068=CARTESIAN_POINT('Ctrl Pts',(-0.180495429923449,0.0143873379575043,
-0.00657696679982974));
#25069=CARTESIAN_POINT('Ctrl Pts',(-0.180494085708543,0.0136985260558778,
-0.00717437305409498));
#25070=CARTESIAN_POINT('Ctrl Pts',(-0.180493597855415,0.0134485369807919,
-0.0073911884671296));
#25071=CARTESIAN_POINT('Ctrl Pts',(-0.180493140703323,0.0131869995586514,
-0.0075950898795007));
#25072=CARTESIAN_POINT('Ctrl Pts',(-0.180492709092622,0.0129152983549508,
-0.0077845977543531));
#25073=CARTESIAN_POINT('Ctrl Pts',(-0.180491519488495,0.0121664363094803,
-0.00830691879254459));
#25074=CARTESIAN_POINT('Ctrl Pts',(-0.180490524505021,0.0113402538840803,
-0.00871961155206156));
#25075=CARTESIAN_POINT('Ctrl Pts',(-0.180489841473695,0.010475431349535,
-0.00900643654204879));
#25076=CARTESIAN_POINT('Ctrl Pts',(-0.18048959464343,0.0101629063354497,
-0.00911008784674441));
#25077=CARTESIAN_POINT('Ctrl Pts',(-0.180489384500336,0.00984527055527501,
-0.00919737486172379));
#25078=CARTESIAN_POINT('Ctrl Pts',(-0.180489215197301,0.00952409565645105,
-0.00926767275065503));
#25079=CARTESIAN_POINT('Ctrl Pts',(-0.18048874602362,0.00863405367343233,
-0.00946248272084727));
#25080=CARTESIAN_POINT('Ctrl Pts',(-0.180488590053928,0.00771686160166094,
-0.00952699527599385));
#25081=CARTESIAN_POINT('Ctrl Pts',(-0.180488753127145,0.0068087871965689,
-0.00946093879366742));
#25082=CARTESIAN_POINT('Ctrl Pts',(-0.18048881243083,0.00647855419143593,
-0.00943691649929942));
#25083=CARTESIAN_POINT('Ctrl Pts',(-0.180488913882774,0.00614947823465072,
-0.00939559647679476));
#25084=CARTESIAN_POINT('Ctrl Pts',(-0.180489057263567,0.00582343159064595,
-0.0093369096156809));
#25085=CARTESIAN_POINT('Ctrl Pts',(-0.180489450424322,0.00492938753887127,
-0.00917598589491597));
#25086=CARTESIAN_POINT('Ctrl Pts',(-0.180490159006754,0.00405811752998488,
-0.00888442947496311));
#25087=CARTESIAN_POINT('Ctrl Pts',(-0.180491091913702,0.0032456634858749,
-0.00847615964082623));
#25088=CARTESIAN_POINT('Ctrl Pts',(-0.180491432870738,0.00294872934590647,
-0.00832694596781499));
#25089=CARTESIAN_POINT('Ctrl Pts',(-0.180491810468584,0.00265955199509477,
-0.00816209795373336));
#25090=CARTESIAN_POINT('Ctrl Pts',(-0.180492218351403,0.00237992845554504,
-0.00798230320031856));
#25091=CARTESIAN_POINT('Ctrl Pts',(-0.180493333494458,0.00161544357674557,
-0.00749074812418146));
#25092=CARTESIAN_POINT('Ctrl Pts',(-0.180494675200404,0.000922426457022649,
-0.00688739759659587));
#25093=CARTESIAN_POINT('Ctrl Pts',(-0.180496337220057,0.000329090474573647,
-0.00619926450814251));
#25094=CARTESIAN_POINT('Ctrl Pts',(-0.180496943504142,0.000112648892505816,
-0.00594824212159634));
#25095=CARTESIAN_POINT('Ctrl Pts',(-0.180497578128166,-9.05934709865707E-5,
-0.00568588146362153));
#25096=CARTESIAN_POINT('Ctrl Pts',(-0.180498255087495,-0.000279289301226472,
-0.005413481592156));
#25097=CARTESIAN_POINT('Ctrl Pts',(-0.180500112668822,-0.000797072033236919,
-0.00466601436160086));
#25098=CARTESIAN_POINT('Ctrl Pts',(-0.180502288445076,-0.00120528133270418,
-0.00384294365333793));
#25099=CARTESIAN_POINT('Ctrl Pts',(-0.180504030056536,-0.00148980242281501,
-0.0029799515977759));
#25100=CARTESIAN_POINT('Ctrl Pts',(-0.180504663447986,-0.00159327741133636,
-0.00266609755972017));
#25101=CARTESIAN_POINT('Ctrl Pts',(-0.180505273972546,-0.00168044127198726,
-0.00234683231956376));
#25102=CARTESIAN_POINT('Ctrl Pts',(-0.180505797177316,-0.00175059117883485,
-0.00202388931840672));
#25103=CARTESIAN_POINT('Ctrl Pts',(-0.180507236890724,-0.00194362413133551,
-0.00113524036926128));
#25104=CARTESIAN_POINT('Ctrl Pts',(-0.180508014788672,-0.00200773829548467,
-0.000218750017278828));
#25105=CARTESIAN_POINT('Ctrl Pts',(-0.18050756675746,-0.00194262103711012,
0.000687516385167797));
#25106=CARTESIAN_POINT('Ctrl Pts',(-0.18050740395279,-0.00191895886023441,
0.00101683362680998));
#25107=CARTESIAN_POINT('Ctrl Pts',(-0.180507087365724,-0.0018782492411139,
0.00134480018749305));
#25108=CARTESIAN_POINT('Ctrl Pts',(-0.18050662968436,-0.0018204757856677,
0.00166974486293542));
#25109=CARTESIAN_POINT('Ctrl Pts',(-0.180505370126551,-0.0016614808760678,
0.00256400588467813));
#25110=CARTESIAN_POINT('Ctrl Pts',(-0.180503042831105,-0.00137339807730806,
0.00343545636344477));
#25111=CARTESIAN_POINT('Ctrl Pts',(-0.180501042736115,-0.000967262940565802,
0.00425032043965544));
#25112=CARTESIAN_POINT('Ctrl Pts',(-0.180500316492093,-0.000819793337187815,
0.0045462014685407));
#25113=CARTESIAN_POINT('Ctrl Pts',(-0.180499582732681,-0.000656707144888704,
0.00483465770437334));
#25114=CARTESIAN_POINT('Ctrl Pts',(-0.180498892503896,-0.000478610824537603,
0.00511381696861555));
#25115=CARTESIAN_POINT('Ctrl Pts',(-0.180496991097895,1.19995639816014E-5,
0.00588283024647891));
#25116=CARTESIAN_POINT('Ctrl Pts',(-0.180495421036052,0.000616709580096667,
0.00658110736474186));
#25117=CARTESIAN_POINT('Ctrl Pts',(-0.180494077221384,0.00130607220731985,
0.00717829217819236));
#25118=CARTESIAN_POINT('Ctrl Pts',(-0.180492713748997,0.00208357848608163,
0.00778381456156277));
#25119=CARTESIAN_POINT('Ctrl Pts',(-0.180491527231616,0.00283280398077721,
0.00830658235132092));
#25120=CARTESIAN_POINT('Ctrl Pts',(-0.180490539611414,0.00365797125397222,
0.00871895924666266));
#25121=CARTESIAN_POINT('Ctrl Pts',(-0.180489844972134,0.00452428905665735,
0.0090063203212091));
#25122=CARTESIAN_POINT('Ctrl Pts',(-0.180489595209188,0.00483578034829864,
0.00910964322649913));
#25123=CARTESIAN_POINT('Ctrl Pts',(-0.180489383382281,0.00515266432219857,
0.00919681506862515));
#25124=CARTESIAN_POINT('Ctrl Pts',(-0.180489213232927,0.00547326492548861,
0.00926709504263265));
#25125=CARTESIAN_POINT('Ctrl Pts',(-0.180488740001119,0.00636494273336552,
0.00946256283813135));
#25126=CARTESIAN_POINT('Ctrl Pts',(-0.180488589317135,0.00728538046776418,
0.00952730360716332));
#25127=CARTESIAN_POINT('Ctrl Pts',(-0.180488753931549,0.00819563487316819,
0.00946063692069833));
#25128=CARTESIAN_POINT('Ctrl Pts',(-0.18048881296935,0.00852209120843912,
0.00943672738286055));
#25129=CARTESIAN_POINT('Ctrl Pts',(-0.180488913061566,0.00884732386434948,
0.00939591666247467));
#25130=CARTESIAN_POINT('Ctrl Pts',(-0.180489054012028,0.00916952818551784,
0.00933817345182018));
#25131=CARTESIAN_POINT('Ctrl Pts',(-0.180489447378089,0.0100687394631446,
0.00917702307978729));
#25132=CARTESIAN_POINT('Ctrl Pts',(-0.180490159114969,0.0109443343949455,
0.00888392857305358));
#25133=CARTESIAN_POINT('Ctrl Pts',(-0.180491097780424,0.0117599091286999,
0.00847339840641515));
#25134=CARTESIAN_POINT('Ctrl Pts',(-0.180491433329071,0.0120514560236885,
0.00832664447887299));
#25135=CARTESIAN_POINT('Ctrl Pts',(-0.180491803878337,0.0123354002447643,
0.00816486104868504));
#25136=CARTESIAN_POINT('Ctrl Pts',(-0.1804922034718,0.0126101076158722,
0.00798869938687643));
#25137=CARTESIAN_POINT('Ctrl Pts',(-0.180493322240716,0.0133792244714115,
0.00749548763631303));
#25138=CARTESIAN_POINT('Ctrl Pts',(-0.180494668822925,0.0140759154697159,
0.00688956279261156));
#25139=CARTESIAN_POINT('Ctrl Pts',(-0.180496341168924,0.0146721295242753,
0.00619783709289612));
#25140=CARTESIAN_POINT('Ctrl Pts',(-0.180496938961584,0.0148852507239376,
0.00595057453705201));
#25141=CARTESIAN_POINT('Ctrl Pts',(-0.180497564189998,0.0150855886906841,
0.00569228752533243));
#25142=CARTESIAN_POINT('Ctrl Pts',(-0.180498230460235,0.0152718433472023,
0.00542420786392051));
#25143=CARTESIAN_POINT('Ctrl Pts',(-0.180500093843356,0.0157927487763465,
0.0046744593546316));
#25144=CARTESIAN_POINT('Ctrl Pts',(-0.180502277572748,0.0162034481788898,
0.00384810331139103));
#25145=CARTESIAN_POINT('Ctrl Pts',(-0.180504027062762,0.0164893813621227,
0.0029812596211392));
#25146=CARTESIAN_POINT('Ctrl Pts',(-0.180504379031403,0.0165469064197915,
0.00280686491567759));
#25147=CARTESIAN_POINT('Ctrl Pts',(-0.180504723822302,0.0165993949346352,
0.00263079819845253));
#25148=CARTESIAN_POINT('Ctrl Pts',(-0.180505050469422,0.0166467264643195,
0.0024533497791677));
#25149=CARTESIAN_POINT('Ctrl Pts',(-0.238376419148325,0.0160572510994551,
0.00229523935965256));
#25150=CARTESIAN_POINT('Ctrl Pts',(-0.180143329927774,0.0166506887410553,
0.00245441214111993));
#25151=CARTESIAN_POINT('Ctrl Pts',(-0.238376419148325,0.0160499153270237,
0.00339695540894448));
#25152=CARTESIAN_POINT('Ctrl Pts',(-0.180143329927774,0.0163802403000704,
0.00346535234146251));
#25153=CARTESIAN_POINT('Ctrl Pts',(-0.238376419148325,0.0156043581343594,
0.00560766010208411));
#25154=CARTESIAN_POINT('Ctrl Pts',(-0.180143329927774,0.0155045639563625,
0.00538672371465897));
#25155=CARTESIAN_POINT('Ctrl Pts',(-0.238376419148325,0.0137116283891667,
0.00844195664423076));
#25156=CARTESIAN_POINT('Ctrl Pts',(-0.180143329927774,0.0133464539612027,
0.00767441593321455));
#25157=CARTESIAN_POINT('Ctrl Pts',(-0.238376419148325,0.0108665999736013,
0.0103474435450232));
#25158=CARTESIAN_POINT('Ctrl Pts',(-0.180143329927774,0.0105817751956803,
0.00914209790934899));
#25159=CARTESIAN_POINT('Ctrl Pts',(-0.238376419148325,0.0075,0.0110189940848823));
#25160=CARTESIAN_POINT('Ctrl Pts',(-0.180143329927774,0.0075,0.00964748427001006));
#25161=CARTESIAN_POINT('Ctrl Pts',(-0.238376419148325,0.00413340002639867,
0.0103474435450232));
#25162=CARTESIAN_POINT('Ctrl Pts',(-0.180143329927774,0.0044182248043197,
0.00914209790934899));
#25163=CARTESIAN_POINT('Ctrl Pts',(-0.238376419148325,0.00128837161083331,
0.00844195664423074));
#25164=CARTESIAN_POINT('Ctrl Pts',(-0.180143329927774,0.00165354603879735,
0.00767441593321453));
#25165=CARTESIAN_POINT('Ctrl Pts',(-0.238376419148325,-0.000604358134359394,
0.00560766010208411));
#25166=CARTESIAN_POINT('Ctrl Pts',(-0.180143329927774,-0.000504563956362522,
0.00538672371465897));
#25167=CARTESIAN_POINT('Ctrl Pts',(-0.238376419148325,-0.00104991532702373,
0.00339695540894447));
#25168=CARTESIAN_POINT('Ctrl Pts',(-0.180143329927774,-0.00138024030007043,
0.00346535234146251));
#25169=CARTESIAN_POINT('Ctrl Pts',(-0.238376419148325,-0.00105996989569538,
0.00188691951593846));
#25170=CARTESIAN_POINT('Ctrl Pts',(-0.180143329927774,-0.00175092279430951,
0.00207973579427586));
#25171=CARTESIAN_POINT('Ctrl Pts',(-0.238376419148325,-0.00106440179407383,
0.00111305841215638));
#25172=CARTESIAN_POINT('Ctrl Pts',(-0.180143329927774,-0.00191431390523475,
0.0012839986244053));
#25173=CARTESIAN_POINT('Ctrl Pts',(-0.238376419148325,-0.00106680965804379,
-1.88715094039015E-18));
#25174=CARTESIAN_POINT('Ctrl Pts',(-0.180143329927774,-0.00200308479649061,
-3.46556198647675E-18));
#25175=CARTESIAN_POINT('Ctrl Pts',(-0.238376419148325,-0.00106440179407383,
-0.00111305841215639));
#25176=CARTESIAN_POINT('Ctrl Pts',(-0.180143329927774,-0.00191431390523475,
-0.0012839986244053));
#25177=CARTESIAN_POINT('Ctrl Pts',(-0.238376419148325,-0.00105996989569538,
-0.00188691951593846));
#25178=CARTESIAN_POINT('Ctrl Pts',(-0.180143329927774,-0.00175092279430951,
-0.00207973579427587));
#25179=CARTESIAN_POINT('Ctrl Pts',(-0.238376419148325,-0.00104991532702373,
-0.00339695540894448));
#25180=CARTESIAN_POINT('Ctrl Pts',(-0.180143329927774,-0.00138024030007042,
-0.00346535234146251));
#25181=CARTESIAN_POINT('Ctrl Pts',(-0.238376419148325,-0.000604358134359395,
-0.00560766010208411));
#25182=CARTESIAN_POINT('Ctrl Pts',(-0.180143329927774,-0.000504563956362519,
-0.00538672371465899));
#25183=CARTESIAN_POINT('Ctrl Pts',(-0.238376419148325,0.00128837161083331,
-0.00844195664423075));
#25184=CARTESIAN_POINT('Ctrl Pts',(-0.180143329927774,0.00165354603879737,
-0.00767441593321454));
#25185=CARTESIAN_POINT('Ctrl Pts',(-0.238376419148325,0.00413340002639866,
-0.0103474435450231));
#25186=CARTESIAN_POINT('Ctrl Pts',(-0.180143329927774,0.0044182248043197,
-0.00914209790934901));
#25187=CARTESIAN_POINT('Ctrl Pts',(-0.238376419148325,0.0075,-0.0110189940848823));
#25188=CARTESIAN_POINT('Ctrl Pts',(-0.180143329927774,0.0075,-0.00964748427001004));
#25189=CARTESIAN_POINT('Ctrl Pts',(-0.238376419148325,0.0108665999736013,
-0.0103474435450232));
#25190=CARTESIAN_POINT('Ctrl Pts',(-0.180143329927774,0.0105817751956803,
-0.00914209790934901));
#25191=CARTESIAN_POINT('Ctrl Pts',(-0.238376419148325,0.0137116283891667,
-0.00844195664423074));
#25192=CARTESIAN_POINT('Ctrl Pts',(-0.180143329927774,0.0133464539612027,
-0.00767441593321454));
#25193=CARTESIAN_POINT('Ctrl Pts',(-0.238376419148325,0.0156043581343594,
-0.00560766010208412));
#25194=CARTESIAN_POINT('Ctrl Pts',(-0.180143329927774,0.0155045639563625,
-0.00538672371465897));
#25195=CARTESIAN_POINT('Ctrl Pts',(-0.238376419148325,0.0160499153270237,
-0.00339695540894448));
#25196=CARTESIAN_POINT('Ctrl Pts',(-0.180143329927774,0.0163802403000704,
-0.00346535234146251));
#25197=CARTESIAN_POINT('Ctrl Pts',(-0.238376419148325,0.0160599698956954,
-0.00188691951593846));
#25198=CARTESIAN_POINT('Ctrl Pts',(-0.180143329927774,0.0167509227943095,
-0.00207973579427587));
#25199=CARTESIAN_POINT('Ctrl Pts',(-0.238376419148325,0.0160644017940738,
-0.00111305841215638));
#25200=CARTESIAN_POINT('Ctrl Pts',(-0.180143329927774,0.0169143139052348,
-0.0012839986244053));
#25201=CARTESIAN_POINT('Ctrl Pts',(-0.238376419148325,0.0160668096580438,
-5.5742513075403E-20));
#25202=CARTESIAN_POINT('Ctrl Pts',(-0.180143329927774,0.0170030847964906,
-2.05506317145176E-18));
#25203=CARTESIAN_POINT('Ctrl Pts',(-0.238376419148325,0.0160644017940738,
0.00111305841215638));
#25204=CARTESIAN_POINT('Ctrl Pts',(-0.180143329927774,0.0169143139052348,
0.0012839986244053));
#25205=CARTESIAN_POINT('Ctrl Pts',(-0.238376419148325,0.0160599698956954,
0.00188691951593846));
#25206=CARTESIAN_POINT('Ctrl Pts',(-0.180143329927774,0.0167509227943095,
0.00207973579427586));
#25207=CARTESIAN_POINT('Ctrl Pts',(-0.238376419148325,0.0160572510994551,
0.00229523935965256));
#25208=CARTESIAN_POINT('Ctrl Pts',(-0.180143329927774,0.0166506887410553,
0.00245441214111993));
#25209=CARTESIAN_POINT('',(-0.238020422914454,0.0160608789606638,0.00229621243031557));
#25210=CARTESIAN_POINT('Ctrl Pts',(-0.180505053483848,0.0166470025142571,
0.00245342341554633));
#25211=CARTESIAN_POINT('Ctrl Pts',(-0.238020422914454,0.0160608789606638,
0.00229621243031557));
#25212=CARTESIAN_POINT('',(-0.237977937649492,0.00102548423602744,0.00782605181637851));
#25213=CARTESIAN_POINT('Ctrl Pts',(-0.180494073660068,0.00130587316507919,
0.0071785219603984));
#25214=CARTESIAN_POINT('Ctrl Pts',(-0.237977933526904,0.00102520228666307,
0.00782629549301537));
#25215=CARTESIAN_POINT('',(-0.238020316532522,-0.00106075457250487,0.00231025307800846));
#25216=CARTESIAN_POINT('Ctrl Pts',(-0.238020318599055,-0.00106098169283407,
0.00231040371569406));
#25217=CARTESIAN_POINT('Ctrl Pts',(-0.238014604516959,-0.00105350020411119,
0.00306190054704093));
#25218=CARTESIAN_POINT('Ctrl Pts',(-0.238004107697475,-0.000841551378611133,
0.00446246739893098));
#25219=CARTESIAN_POINT('Ctrl Pts',(-0.237993318101237,-0.00027785053263636,
0.00587614678579025));
#25220=CARTESIAN_POINT('Ctrl Pts',(-0.237986081899084,0.000251531250557718,
0.00680176374543222));
#25221=CARTESIAN_POINT('Ctrl Pts',(-0.237981570675819,0.000647625364551933,
0.00737065558877918));
#25222=CARTESIAN_POINT('Ctrl Pts',(-0.237979022233705,0.000907805533526721,
0.00768990840376775));
#25223=CARTESIAN_POINT('Ctrl Pts',(-0.237977937649492,0.00102548423602743,
0.00782605181637851));
#25224=CARTESIAN_POINT('',(-0.238020316532533,-0.00106075457252077,-0.0023102530755598));
#25225=CARTESIAN_POINT('Ctrl Pts',(-0.238020316619813,-0.00106075405523068,
-0.00231028189603671));
#25226=CARTESIAN_POINT('Ctrl Pts',(-0.238020352159604,-0.00106079956504005,
-0.00230559487996849));
#25227=CARTESIAN_POINT('Ctrl Pts',(-0.238020387591151,-0.00106084120528452,
-0.00230090505001212));
#25228=CARTESIAN_POINT('Ctrl Pts',(-0.238020422914453,-0.0010608789606638,
-0.00229621243031556));
#25229=CARTESIAN_POINT('Ctrl Pts',(-0.238023371086054,-0.0010640301194925,
-0.00190455459856342));
#25230=CARTESIAN_POINT('Ctrl Pts',(-0.238025565230501,-0.00106677025071908,
-0.00151323660125846));
#25231=CARTESIAN_POINT('Ctrl Pts',(-0.238027005347795,-0.00106864274316786,
-0.00112190150667839));
#25232=CARTESIAN_POINT('Ctrl Pts',(-0.238028380588602,-0.00107043088086772,
-0.000748195841613378));
#25233=CARTESIAN_POINT('Ctrl Pts',(-0.238029068209006,-0.0010714200523582,
-0.000374041179707509));
#25234=CARTESIAN_POINT('Ctrl Pts',(-0.238029068209006,-0.0010714200523582,
-5.10251228893053E-18));
#25235=CARTESIAN_POINT('Ctrl Pts',(-0.238029068209005,-0.0010714200523582,
0.000374041179701486));
#25236=CARTESIAN_POINT('Ctrl Pts',(-0.238028380588602,-0.00107043088086775,
0.000748195841607102));
#25237=CARTESIAN_POINT('Ctrl Pts',(-0.238027005347795,-0.00106864274316786,
0.00112190150667838));
#25238=CARTESIAN_POINT('Ctrl Pts',(-0.238025565230501,-0.00106677025071912,
0.00151323660125024));
#25239=CARTESIAN_POINT('Ctrl Pts',(-0.238023371086054,-0.00106403011949258,
0.00190455459855405));
#25240=CARTESIAN_POINT('Ctrl Pts',(-0.238020422914453,-0.0010608789606638,
0.00229621243031557));
#25241=CARTESIAN_POINT('Ctrl Pts',(-0.238020387591146,-0.00106084120527947,
0.00230090505063957));
#25242=CARTESIAN_POINT('Ctrl Pts',(-0.238020352159595,-0.00106079956502891,
0.00230559488122262));
#25243=CARTESIAN_POINT('Ctrl Pts',(-0.238020316619799,-0.00106075405521242,
0.0023102818979168));
#25244=CARTESIAN_POINT('',(-0.238020316532523,0.0160607545725048,-0.00231025307801074));
#25245=CARTESIAN_POINT('Ctrl Pts',(-0.238020318599054,0.0160609816928344,
-0.00231040371569625));
#25246=CARTESIAN_POINT('Ctrl Pts',(-0.238014604517819,0.016053500205237,
-0.00306190043396615));
#25247=CARTESIAN_POINT('Ctrl Pts',(-0.238004107699624,0.0158415514403933,
-0.00446246711947055));
#25248=CARTESIAN_POINT('Ctrl Pts',(-0.237993318103923,0.0152778506838575,
-0.00587614646494471));
#25249=CARTESIAN_POINT('Ctrl Pts',(-0.237986081901558,0.0147484689245685,
-0.00680176347060161));
#25250=CARTESIAN_POINT('Ctrl Pts',(-0.23798136150549,0.0143340090615772,
-0.00739703324374946));
#25251=CARTESIAN_POINT('Ctrl Pts',(-0.237977986253456,0.0139854138410196,
-0.00781963052493187));
#25252=CARTESIAN_POINT('Ctrl Pts',(-0.237975976938392,0.0137543357831049,
-0.0080725654215816));
#25253=CARTESIAN_POINT('Ctrl Pts',(-0.237974841983293,0.0136151820866611,
-0.00821658632941533));
#25254=CARTESIAN_POINT('Ctrl Pts',(-0.237974243379501,0.0135400220076929,
-0.00829300142009656));
#25255=CARTESIAN_POINT('Ctrl Pts',(-0.237972889875128,0.0133608675439882,
-0.00846684804851594));
#25256=CARTESIAN_POINT('Ctrl Pts',(-0.237971411861785,0.0131526205788322,
-0.0086569885059668));
#25257=CARTESIAN_POINT('Ctrl Pts',(-0.237968828324772,0.0127606952743352,
-0.00899010162830897));
#25258=CARTESIAN_POINT('Ctrl Pts',(-0.23796558142955,0.0121803403678554,
-0.00940998980172909));
#25259=CARTESIAN_POINT('Ctrl Pts',(-0.237962258740912,0.011442842468399,
-0.00983942706026314));
#25260=CARTESIAN_POINT('Ctrl Pts',(-0.237958641690952,0.0104233649905898,
-0.010304854326046));
#25261=CARTESIAN_POINT('Ctrl Pts',(-0.237955622814505,0.00909678549852576,
-0.0106872846852435));
#25262=CARTESIAN_POINT('Ctrl Pts',(-0.237954410173046,0.00750600282866814,
-0.0108341606636561));
#25263=CARTESIAN_POINT('Ctrl Pts',(-0.237955607770554,0.00591243383673865,
-0.0106891746012175));
#25264=CARTESIAN_POINT('Ctrl Pts',(-0.237958618664386,0.00458475323403587,
-0.0103078244918697));
#25265=CARTESIAN_POINT('Ctrl Pts',(-0.237962231319832,0.00356398336301219,
-0.00984298458230142));
#25266=CARTESIAN_POINT('Ctrl Pts',(-0.237965551695216,0.00282554706414488,
-0.00941384981571709));
#25267=CARTESIAN_POINT('Ctrl Pts',(-0.237968797940997,0.00224435283945219,
-0.00899403466574531));
#25268=CARTESIAN_POINT('Ctrl Pts',(-0.237971380735772,0.00185193966955052,
-0.00866100194975026));
#25269=CARTESIAN_POINT('Ctrl Pts',(-0.237972859646126,0.00164327921911097,
-0.00847073517420804));
#25270=CARTESIAN_POINT('Ctrl Pts',(-0.237974210547823,0.00146420766709804,
-0.00829721467232998));
#25271=CARTESIAN_POINT('Ctrl Pts',(-0.237974819394004,0.00138764039313657,
-0.00821947035633698));
#25272=CARTESIAN_POINT('Ctrl Pts',(-0.237975950670599,0.00124880288754097,
-0.0080759099575687));
#25273=CARTESIAN_POINT('Ctrl Pts',(-0.237977961897761,0.00101723345554436,
-0.00782271998155836));
#25274=CARTESIAN_POINT('Ctrl Pts',(-0.237981336299155,0.000668421674808697,
-0.00740024611366686));
#25275=CARTESIAN_POINT('Ctrl Pts',(-0.237986058550236,0.000253414863704401,
-0.00680477583222583));
#25276=CARTESIAN_POINT('Ctrl Pts',(-0.237993298003416,-0.000276649707725574,
-0.0058787917379549));
#25277=CARTESIAN_POINT('Ctrl Pts',(-0.238004094529999,-0.000841198091866792,
-0.00446423767063164));
#25278=CARTESIAN_POINT('Ctrl Pts',(-0.238014599650372,-0.00105349359705469,
-0.00306254026317131));
#25279=CARTESIAN_POINT('Ctrl Pts',(-0.23802031859663,-0.00106098145426406,
-0.00231040371318102));
#25280=CARTESIAN_POINT('Ctrl Pts',(-0.238020422914454,0.0160608789606638,
0.00229621243031557));
#25281=CARTESIAN_POINT('Ctrl Pts',(-0.238023371086056,0.0160640301194921,
0.00190455459861773));
#25282=CARTESIAN_POINT('Ctrl Pts',(-0.238025565230504,0.0160667702507188,
0.00151323660130437));
#25283=CARTESIAN_POINT('Ctrl Pts',(-0.238027005347798,0.0160686427431678,
0.00112190150667837));
#25284=CARTESIAN_POINT('Ctrl Pts',(-0.238028380588605,0.0160704308808675,
0.000748195841645495));
#25285=CARTESIAN_POINT('Ctrl Pts',(-0.238029068209008,0.0160714200523582,
0.000374041179736735));
#25286=CARTESIAN_POINT('Ctrl Pts',(-0.238029068209008,0.0160714200523582,
5.20127317150229E-18));
#25287=CARTESIAN_POINT('Ctrl Pts',(-0.238029068209007,0.0160714200523582,
-0.00037404117967552));
#25288=CARTESIAN_POINT('Ctrl Pts',(-0.238028380588604,0.0160704308808678,
-0.000748195841581645));
#25289=CARTESIAN_POINT('Ctrl Pts',(-0.238027005347796,0.0160686427431678,
-0.00112190150667836));
#25290=CARTESIAN_POINT('Ctrl Pts',(-0.238025565230502,0.0160667702507193,
-0.00151323660122079));
#25291=CARTESIAN_POINT('Ctrl Pts',(-0.238023371086054,0.0160640301194929,
-0.00190455459852223));
#25292=CARTESIAN_POINT('Ctrl Pts',(-0.238020422914453,0.0160608789606638,
-0.00229621243031559));
#25293=CARTESIAN_POINT('Ctrl Pts',(-0.238020387591146,0.0160608412052795,
-0.00230090505064033));
#25294=CARTESIAN_POINT('Ctrl Pts',(-0.238020352159595,0.0160607995650289,
-0.00230559488122414));
#25295=CARTESIAN_POINT('Ctrl Pts',(-0.238020316619799,0.0160607540552124,
-0.00231028189791906));
#25296=CARTESIAN_POINT('Origin',(-0.24,0.0075,0.));
#25297=CARTESIAN_POINT('',(-0.1795,0.0075,0.005));
#25298=CARTESIAN_POINT('',(-0.1795,0.0075,-0.005));
#25299=CARTESIAN_POINT('Origin',(-0.1795,0.0075,0.));
#25300=CARTESIAN_POINT('Origin',(-0.1795,0.0075,0.));
#25301=CARTESIAN_POINT('',(-0.1405,0.0075,0.005));
#25302=CARTESIAN_POINT('',(-0.24,0.0075,0.005));
#25303=CARTESIAN_POINT('',(-0.1405,0.0075,-0.005));
#25304=CARTESIAN_POINT('Origin',(-0.1405,0.0075,0.));
#25305=CARTESIAN_POINT('Origin',(-0.1405,0.0075,0.));
#25306=CARTESIAN_POINT('Origin',(-0.24,0.0075,0.));
#25307=CARTESIAN_POINT('',(-0.16,0.0075,0.0074756477610481));
#25308=CARTESIAN_POINT('Origin',(-0.16,0.0075,0.));
#25309=CARTESIAN_POINT('',(-0.1795,0.0075,0.0074756477610481));
#25310=CARTESIAN_POINT('',(-0.24,0.0075,0.0074756477610481));
#25311=CARTESIAN_POINT('',(-0.1795,0.0075,-0.0074756477610481));
#25312=CARTESIAN_POINT('Origin',(-0.1795,0.0075,0.));
#25313=CARTESIAN_POINT('Origin',(-0.1795,0.0075,0.));
#25314=CARTESIAN_POINT('Origin',(-0.16,0.0075,0.));
#25315=CARTESIAN_POINT('',(-0.1405,0.0075,0.00932888901198444));
#25316=CARTESIAN_POINT('',(-0.1405,0.0075,-0.00932888901198444));
#25317=CARTESIAN_POINT('Origin',(-0.1405,0.0075,0.));
#25318=CARTESIAN_POINT('Origin',(-0.1405,0.0075,0.));
#25319=CARTESIAN_POINT('',(-0.1406,0.0075,0.00932888901198444));
#25320=CARTESIAN_POINT('',(-0.16,0.0075,0.00932888901198444));
#25321=CARTESIAN_POINT('',(-0.1406,0.0075,-0.00932888901198444));
#25322=CARTESIAN_POINT('Origin',(-0.1406,0.0075,0.));
#25323=CARTESIAN_POINT('Origin',(-0.1406,0.0075,0.));
#25324=CARTESIAN_POINT('Origin',(-0.16,0.0075,0.));
#25325=CARTESIAN_POINT('',(-0.159473534924936,0.0075,0.00932888901198444));
#25326=CARTESIAN_POINT('Origin',(-0.159473534924936,0.0075,0.));
#25327=CARTESIAN_POINT('',(-0.1595,0.0075,0.00932888901198444));
#25328=CARTESIAN_POINT('',(-0.16,0.0075,0.00932888901198444));
#25329=CARTESIAN_POINT('',(-0.1595,0.0075,-0.00932888901198444));
#25330=CARTESIAN_POINT('Origin',(-0.1595,0.0075,0.));
#25331=CARTESIAN_POINT('Origin',(-0.1595,0.0075,0.));
#25332=CARTESIAN_POINT('Origin',(-0.14,0.,0.));
#25333=CARTESIAN_POINT('',(-0.14,0.0075,-0.00882888901198444));
#25334=CARTESIAN_POINT('Origin',(-0.14,0.0075,0.));
#25335=CARTESIAN_POINT('',(-0.14,0.0075,-0.0055));
#25336=CARTESIAN_POINT('Origin',(-0.14,0.0075,0.));
#25337=CARTESIAN_POINT('Origin',(-0.16,0.,0.));
#25338=CARTESIAN_POINT('',(-0.16,0.0075,-0.00882888901198444));
#25339=CARTESIAN_POINT('Origin',(-0.16,0.0075,0.));
#25340=CARTESIAN_POINT('Origin',(0.0540947251599426,0.0075,0.));
#25341=CARTESIAN_POINT('',(-0.1585,0.0075,-0.00898940279602035));
#25342=CARTESIAN_POINT('',(-0.1585,0.0075,0.00898940279602035));
#25343=CARTESIAN_POINT('Origin',(-0.1585,0.0075,0.));
#25344=CARTESIAN_POINT('Origin',(-0.1585,0.0075,0.));
#25345=CARTESIAN_POINT('',(-0.159,0.0075,0.00898940279602035));
#25346=CARTESIAN_POINT('',(0.0540947251599426,0.0075,0.00898940279602035));
#25347=CARTESIAN_POINT('Origin',(-0.159,0.0075,0.));
#25348=CARTESIAN_POINT('Origin',(0.0540947251599426,0.0075,0.));
#25349=CARTESIAN_POINT('',(-0.141,0.0075,-0.00912888901198444));
#25350=CARTESIAN_POINT('',(-0.141,0.0075,0.00912888901198444));
#25351=CARTESIAN_POINT('Origin',(-0.141,0.0075,0.));
#25352=CARTESIAN_POINT('Origin',(-0.141,0.0075,0.));
#25353=CARTESIAN_POINT('',(-0.1415,0.0075,0.00912888901198444));
#25354=CARTESIAN_POINT('',(0.0540947251599426,0.0075,0.00912888901198444));
#25355=CARTESIAN_POINT('Origin',(-0.1415,0.0075,0.));
#25356=CARTESIAN_POINT('Origin',(-0.16,0.0075,0.));
#25357=CARTESIAN_POINT('',(-0.150973534924937,0.0075,0.00932888901198444));
#25358=CARTESIAN_POINT('Origin',(-0.150973534924937,0.0075,0.));
#25359=CARTESIAN_POINT('',(-0.158026465075064,0.0075,0.00932888901198444));
#25360=CARTESIAN_POINT('',(-0.16,0.0075,0.00932888901198444));
#25361=CARTESIAN_POINT('',(-0.158026465075064,0.0075,-0.00932888901198444));
#25362=CARTESIAN_POINT('Origin',(-0.158026465075064,0.0075,0.));
#25363=CARTESIAN_POINT('Origin',(-0.158026465075064,0.0075,0.));
#25364=CARTESIAN_POINT('Origin',(-0.16,0.0075,0.));
#25365=CARTESIAN_POINT('',(-0.1419,0.0075,0.00932888901198444));
#25366=CARTESIAN_POINT('Origin',(-0.1419,0.0075,0.));
#25367=CARTESIAN_POINT('',(-0.1421,0.0075,0.00932888901198444));
#25368=CARTESIAN_POINT('',(-0.16,0.0075,0.00932888901198444));
#25369=CARTESIAN_POINT('',(-0.1421,0.0075,-0.00932888901198444));
#25370=CARTESIAN_POINT('Origin',(-0.1421,0.0075,0.));
#25371=CARTESIAN_POINT('Origin',(-0.1421,0.0075,0.));
#25372=CARTESIAN_POINT('Origin',(0.0540947251599426,0.0075,0.));
#25373=CARTESIAN_POINT('',(-0.15,0.0075,-0.00898940279602035));
#25374=CARTESIAN_POINT('',(-0.15,0.0075,0.00898940279602035));
#25375=CARTESIAN_POINT('Origin',(-0.15,0.0075,0.));
#25376=CARTESIAN_POINT('Origin',(-0.15,0.0075,0.));
#25377=CARTESIAN_POINT('',(-0.1505,0.0075,0.00898940279602035));
#25378=CARTESIAN_POINT('',(0.0540947251599426,0.0075,0.00898940279602035));
#25379=CARTESIAN_POINT('Origin',(-0.1505,0.0075,0.));
#25380=CARTESIAN_POINT('Origin',(0.0540947251599426,0.0075,0.));
#25381=CARTESIAN_POINT('',(-0.1425,0.0075,-0.00912888901198443));
#25382=CARTESIAN_POINT('',(-0.1425,0.0075,0.00912888901198443));
#25383=CARTESIAN_POINT('Origin',(-0.1425,0.0075,0.));
#25384=CARTESIAN_POINT('Origin',(-0.1425,0.0075,0.));
#25385=CARTESIAN_POINT('',(-0.143,0.0075,0.00912888901198443));
#25386=CARTESIAN_POINT('',(0.0540947251599426,0.0075,0.00912888901198443));
#25387=CARTESIAN_POINT('Origin',(-0.143,0.0075,0.));
#25388=CARTESIAN_POINT('Origin',(-0.16,0.0075,0.));
#25389=CARTESIAN_POINT('',(-0.1479,0.0075,0.00932888901198444));
#25390=CARTESIAN_POINT('Origin',(-0.1479,0.0075,0.));
#25391=CARTESIAN_POINT('',(-0.149526465075064,0.0075,0.00932888901198444));
#25392=CARTESIAN_POINT('',(-0.16,0.0075,0.00932888901198444));
#25393=CARTESIAN_POINT('',(-0.149526465075064,0.0075,-0.00932888901198444));
#25394=CARTESIAN_POINT('Origin',(-0.149526465075064,0.0075,0.));
#25395=CARTESIAN_POINT('Origin',(-0.149526465075064,0.0075,0.));
#25396=CARTESIAN_POINT('Origin',(0.0540947251599426,0.0075,0.));
#25397=CARTESIAN_POINT('',(-0.147,0.0075,-0.0091288890119844));
#25398=CARTESIAN_POINT('',(-0.147,0.0075,0.0091288890119844));
#25399=CARTESIAN_POINT('Origin',(-0.147,0.0075,0.));
#25400=CARTESIAN_POINT('Origin',(-0.147,0.0075,0.));
#25401=CARTESIAN_POINT('',(-0.1475,0.0075,0.0091288890119844));
#25402=CARTESIAN_POINT('',(0.0540947251599426,0.0075,0.0091288890119844));
#25403=CARTESIAN_POINT('Origin',(-0.1475,0.0075,0.));
#25404=CARTESIAN_POINT('Origin',(-0.16,0.0075,0.));
#25405=CARTESIAN_POINT('',(-0.1464,0.0075,0.00932888901198444));
#25406=CARTESIAN_POINT('Origin',(-0.1464,0.0075,0.));
#25407=CARTESIAN_POINT('',(-0.1466,0.0075,0.00932888901198444));
#25408=CARTESIAN_POINT('',(-0.16,0.0075,0.00932888901198444));
#25409=CARTESIAN_POINT('',(-0.1466,0.0075,-0.00932888901198444));
#25410=CARTESIAN_POINT('Origin',(-0.1466,0.0075,0.));
#25411=CARTESIAN_POINT('Origin',(-0.1466,0.0075,0.));
#25412=CARTESIAN_POINT('Origin',(0.0540947251599426,0.0075,0.));
#25413=CARTESIAN_POINT('',(-0.1455,0.0075,-0.00912888901198441));
#25414=CARTESIAN_POINT('',(-0.1455,0.0075,0.00912888901198441));
#25415=CARTESIAN_POINT('Origin',(-0.1455,0.0075,0.));
#25416=CARTESIAN_POINT('Origin',(-0.1455,0.0075,0.));
#25417=CARTESIAN_POINT('',(-0.146,0.0075,0.00912888901198441));
#25418=CARTESIAN_POINT('',(0.0540947251599426,0.0075,0.00912888901198441));
#25419=CARTESIAN_POINT('Origin',(-0.146,0.0075,0.));
#25420=CARTESIAN_POINT('Origin',(-0.16,0.0075,0.));
#25421=CARTESIAN_POINT('',(-0.1449,0.0075,0.00932888901198444));
#25422=CARTESIAN_POINT('Origin',(-0.1449,0.0075,0.));
#25423=CARTESIAN_POINT('',(-0.1451,0.0075,0.00932888901198444));
#25424=CARTESIAN_POINT('',(-0.16,0.0075,0.00932888901198444));
#25425=CARTESIAN_POINT('',(-0.1451,0.0075,-0.00932888901198444));
#25426=CARTESIAN_POINT('Origin',(-0.1451,0.0075,0.));
#25427=CARTESIAN_POINT('Origin',(-0.1451,0.0075,0.));
#25428=CARTESIAN_POINT('Origin',(0.0540947251599426,0.0075,0.));
#25429=CARTESIAN_POINT('',(-0.144,0.0075,-0.00912888901198442));
#25430=CARTESIAN_POINT('',(-0.144,0.0075,0.00912888901198442));
#25431=CARTESIAN_POINT('Origin',(-0.144,0.0075,0.));
#25432=CARTESIAN_POINT('Origin',(-0.144,0.0075,0.));
#25433=CARTESIAN_POINT('',(-0.1445,0.0075,0.00912888901198442));
#25434=CARTESIAN_POINT('',(0.0540947251599426,0.0075,0.00912888901198442));
#25435=CARTESIAN_POINT('Origin',(-0.1445,0.0075,0.));
#25436=CARTESIAN_POINT('Origin',(-0.16,0.0075,0.));
#25437=CARTESIAN_POINT('',(-0.1434,0.0075,0.00932888901198444));
#25438=CARTESIAN_POINT('Origin',(-0.1434,0.0075,0.));
#25439=CARTESIAN_POINT('',(-0.1436,0.0075,0.00932888901198444));
#25440=CARTESIAN_POINT('',(-0.16,0.0075,0.00932888901198444));
#25441=CARTESIAN_POINT('',(-0.1436,0.0075,-0.00932888901198444));
#25442=CARTESIAN_POINT('Origin',(-0.1436,0.0075,0.));
#25443=CARTESIAN_POINT('Origin',(-0.1436,0.0075,0.));
#25444=CARTESIAN_POINT('Ctrl Pts',(-0.238376419148325,0.0160572510994551,
0.00229523935965256));
#25445=CARTESIAN_POINT('Ctrl Pts',(-0.180143329927774,0.0166506887410553,
0.00245441214111993));
#25446=CARTESIAN_POINT('Ctrl Pts',(-0.238376419148325,0.0160499153270237,
0.00339695540894448));
#25447=CARTESIAN_POINT('Ctrl Pts',(-0.180143329927774,0.0163802403000704,
0.00346535234146251));
#25448=CARTESIAN_POINT('Ctrl Pts',(-0.238376419148325,0.0156043581343594,
0.00560766010208411));
#25449=CARTESIAN_POINT('Ctrl Pts',(-0.180143329927774,0.0155045639563625,
0.00538672371465897));
#25450=CARTESIAN_POINT('Ctrl Pts',(-0.238376419148325,0.0137116283891667,
0.00844195664423076));
#25451=CARTESIAN_POINT('Ctrl Pts',(-0.180143329927774,0.0133464539612027,
0.00767441593321455));
#25452=CARTESIAN_POINT('Ctrl Pts',(-0.238376419148325,0.0108665999736013,
0.0103474435450232));
#25453=CARTESIAN_POINT('Ctrl Pts',(-0.180143329927774,0.0105817751956803,
0.00914209790934899));
#25454=CARTESIAN_POINT('Ctrl Pts',(-0.238376419148325,0.0075,0.0110189940848823));
#25455=CARTESIAN_POINT('Ctrl Pts',(-0.180143329927774,0.0075,0.00964748427001006));
#25456=CARTESIAN_POINT('Ctrl Pts',(-0.238376419148325,0.00413340002639867,
0.0103474435450232));
#25457=CARTESIAN_POINT('Ctrl Pts',(-0.180143329927774,0.0044182248043197,
0.00914209790934899));
#25458=CARTESIAN_POINT('Ctrl Pts',(-0.238376419148325,0.00128837161083331,
0.00844195664423074));
#25459=CARTESIAN_POINT('Ctrl Pts',(-0.180143329927774,0.00165354603879735,
0.00767441593321453));
#25460=CARTESIAN_POINT('Ctrl Pts',(-0.238376419148325,-0.000604358134359394,
0.00560766010208411));
#25461=CARTESIAN_POINT('Ctrl Pts',(-0.180143329927774,-0.000504563956362522,
0.00538672371465897));
#25462=CARTESIAN_POINT('Ctrl Pts',(-0.238376419148325,-0.00104991532702373,
0.00339695540894447));
#25463=CARTESIAN_POINT('Ctrl Pts',(-0.180143329927774,-0.00138024030007043,
0.00346535234146251));
#25464=CARTESIAN_POINT('Ctrl Pts',(-0.238376419148325,-0.00105996989569538,
0.00188691951593846));
#25465=CARTESIAN_POINT('Ctrl Pts',(-0.180143329927774,-0.00175092279430951,
0.00207973579427586));
#25466=CARTESIAN_POINT('Ctrl Pts',(-0.238376419148325,-0.00106440179407383,
0.00111305841215638));
#25467=CARTESIAN_POINT('Ctrl Pts',(-0.180143329927774,-0.00191431390523475,
0.0012839986244053));
#25468=CARTESIAN_POINT('Ctrl Pts',(-0.238376419148325,-0.00106680965804379,
-1.88715094039015E-18));
#25469=CARTESIAN_POINT('Ctrl Pts',(-0.180143329927774,-0.00200308479649061,
-3.46556198647675E-18));
#25470=CARTESIAN_POINT('Ctrl Pts',(-0.238376419148325,-0.00106440179407383,
-0.00111305841215639));
#25471=CARTESIAN_POINT('Ctrl Pts',(-0.180143329927774,-0.00191431390523475,
-0.0012839986244053));
#25472=CARTESIAN_POINT('Ctrl Pts',(-0.238376419148325,-0.00105996989569538,
-0.00188691951593846));
#25473=CARTESIAN_POINT('Ctrl Pts',(-0.180143329927774,-0.00175092279430951,
-0.00207973579427587));
#25474=CARTESIAN_POINT('Ctrl Pts',(-0.238376419148325,-0.00104991532702373,
-0.00339695540894448));
#25475=CARTESIAN_POINT('Ctrl Pts',(-0.180143329927774,-0.00138024030007042,
-0.00346535234146251));
#25476=CARTESIAN_POINT('Ctrl Pts',(-0.238376419148325,-0.000604358134359395,
-0.00560766010208411));
#25477=CARTESIAN_POINT('Ctrl Pts',(-0.180143329927774,-0.000504563956362519,
-0.00538672371465899));
#25478=CARTESIAN_POINT('Ctrl Pts',(-0.238376419148325,0.00128837161083331,
-0.00844195664423075));
#25479=CARTESIAN_POINT('Ctrl Pts',(-0.180143329927774,0.00165354603879737,
-0.00767441593321454));
#25480=CARTESIAN_POINT('Ctrl Pts',(-0.238376419148325,0.00413340002639866,
-0.0103474435450231));
#25481=CARTESIAN_POINT('Ctrl Pts',(-0.180143329927774,0.0044182248043197,
-0.00914209790934901));
#25482=CARTESIAN_POINT('Ctrl Pts',(-0.238376419148325,0.0075,-0.0110189940848823));
#25483=CARTESIAN_POINT('Ctrl Pts',(-0.180143329927774,0.0075,-0.00964748427001004));
#25484=CARTESIAN_POINT('Ctrl Pts',(-0.238376419148325,0.0108665999736013,
-0.0103474435450232));
#25485=CARTESIAN_POINT('Ctrl Pts',(-0.180143329927774,0.0105817751956803,
-0.00914209790934901));
#25486=CARTESIAN_POINT('Ctrl Pts',(-0.238376419148325,0.0137116283891667,
-0.00844195664423074));
#25487=CARTESIAN_POINT('Ctrl Pts',(-0.180143329927774,0.0133464539612027,
-0.00767441593321454));
#25488=CARTESIAN_POINT('Ctrl Pts',(-0.238376419148325,0.0156043581343594,
-0.00560766010208412));
#25489=CARTESIAN_POINT('Ctrl Pts',(-0.180143329927774,0.0155045639563625,
-0.00538672371465897));
#25490=CARTESIAN_POINT('Ctrl Pts',(-0.238376419148325,0.0160499153270237,
-0.00339695540894448));
#25491=CARTESIAN_POINT('Ctrl Pts',(-0.180143329927774,0.0163802403000704,
-0.00346535234146251));
#25492=CARTESIAN_POINT('Ctrl Pts',(-0.238376419148325,0.0160599698956954,
-0.00188691951593846));
#25493=CARTESIAN_POINT('Ctrl Pts',(-0.180143329927774,0.0167509227943095,
-0.00207973579427587));
#25494=CARTESIAN_POINT('Ctrl Pts',(-0.238376419148325,0.0160644017940738,
-0.00111305841215638));
#25495=CARTESIAN_POINT('Ctrl Pts',(-0.180143329927774,0.0169143139052348,
-0.0012839986244053));
#25496=CARTESIAN_POINT('Ctrl Pts',(-0.238376419148325,0.0160668096580438,
-5.5742513075403E-20));
#25497=CARTESIAN_POINT('Ctrl Pts',(-0.180143329927774,0.0170030847964906,
-2.05506317145176E-18));
#25498=CARTESIAN_POINT('Ctrl Pts',(-0.238376419148325,0.0160644017940738,
0.00111305841215638));
#25499=CARTESIAN_POINT('Ctrl Pts',(-0.180143329927774,0.0169143139052348,
0.0012839986244053));
#25500=CARTESIAN_POINT('Ctrl Pts',(-0.238376419148325,0.0160599698956954,
0.00188691951593846));
#25501=CARTESIAN_POINT('Ctrl Pts',(-0.180143329927774,0.0167509227943095,
0.00207973579427586));
#25502=CARTESIAN_POINT('Ctrl Pts',(-0.238376419148325,0.0160572510994551,
0.00229523935965256));
#25503=CARTESIAN_POINT('Ctrl Pts',(-0.180143329927774,0.0166506887410553,
0.00245441214111993));
#25504=CARTESIAN_POINT('',(-0.238020316532543,0.0160607545725302,0.00231025307448946));
#25505=CARTESIAN_POINT('Ctrl Pts',(-0.238020316619822,0.0160607540552411,
0.00231028189496567));
#25506=CARTESIAN_POINT('Ctrl Pts',(-0.23802035215961,0.0160607995650464,
0.00230559487925404));
#25507=CARTESIAN_POINT('Ctrl Pts',(-0.238020387591155,0.0160608412052874,
0.0023009050496547));
#25508=CARTESIAN_POINT('Ctrl Pts',(-0.238020422914454,0.0160608789606638,
0.00229621243031557));
#25509=CARTESIAN_POINT('Ctrl Pts',(-0.237977937649492,0.00102548423602743,
0.00782605181637851));
#25510=CARTESIAN_POINT('Ctrl Pts',(-0.237977771361891,0.00104352664243288,
0.0078469252176614));
#25511=CARTESIAN_POINT('Ctrl Pts',(-0.237976990708435,0.00112907719101165,
0.00794495085130883));
#25512=CARTESIAN_POINT('Ctrl Pts',(-0.237975976937705,0.0012456642779511,
0.00807256548637949));
#25513=CARTESIAN_POINT('Ctrl Pts',(-0.237974841982942,0.00138481794771289,
0.00821658636396061));
#25514=CARTESIAN_POINT('Ctrl Pts',(-0.237974243379628,0.00145997797384131,
0.00829300140192245));
#25515=CARTESIAN_POINT('Ctrl Pts',(-0.237972889874965,0.00163913249662495,
0.00846684808778011));
#25516=CARTESIAN_POINT('Ctrl Pts',(-0.237971411861517,0.00184737950156088,
0.00865698857652469));
#25517=CARTESIAN_POINT('Ctrl Pts',(-0.237968828324226,0.00223930487946204,
0.00899010176098222));
#25518=CARTESIAN_POINT('Ctrl Pts',(-0.237965581428728,0.00281965996064833,
0.0094099899606304));
#25519=CARTESIAN_POINT('Ctrl Pts',(-0.237962258739981,0.00355715761932815,
0.00983942728785487));
#25520=CARTESIAN_POINT('Ctrl Pts',(-0.237958641689478,0.00457663675962997,
0.0103048542155954));
#25521=CARTESIAN_POINT('Ctrl Pts',(-0.237955622816736,0.00590320392835369,
0.0106872867840954));
#25522=CARTESIAN_POINT('Ctrl Pts',(-0.237954410161632,0.00749403703264914,
0.0108341531591348));
#25523=CARTESIAN_POINT('Ctrl Pts',(-0.23795560781398,0.00908741729428714,
0.0106892025204542));
#25524=CARTESIAN_POINT('Ctrl Pts',(-0.237958618842412,0.0104152747494254,
0.0103078197503335));
#25525=CARTESIAN_POINT('Ctrl Pts',(-0.237962231600465,0.0114360766911925,
0.00984295543332729));
#25526=CARTESIAN_POINT('Ctrl Pts',(-0.237965552197248,0.0121745503730158,
0.00941378412783473));
#25527=CARTESIAN_POINT('Ctrl Pts',(-0.237968798249626,0.0127557129303162,
0.00899399101451944));
#25528=CARTESIAN_POINT('Ctrl Pts',(-0.2379713816927,0.0131481981613132,
0.00866087544582393));
#25529=CARTESIAN_POINT('Ctrl Pts',(-0.237972859766266,0.0133567445403098,
0.00847071847746978));
#25530=CARTESIAN_POINT('Ctrl Pts',(-0.237974213449617,0.0135361635963531,
0.00829684006850807));
#25531=CARTESIAN_POINT('Ctrl Pts',(-0.237974812051711,0.0136114201539808,
0.00822042272077482));
#25532=CARTESIAN_POINT('Ctrl Pts',(-0.237975947163907,0.0137507676709391,
0.00807638082371326));
#25533=CARTESIAN_POINT('Ctrl Pts',(-0.237977956915679,0.0139821694340823,
0.00782339731578715));
#25534=CARTESIAN_POINT('Ctrl Pts',(-0.237981333384561,0.014331271685258,
0.00740067143450062));
#25535=CARTESIAN_POINT('Ctrl Pts',(-0.2379860561487,0.0147463578891999,
0.00680513776468162));
#25536=CARTESIAN_POINT('Ctrl Pts',(-0.237993296733614,0.0152765669110609,
0.00587899756444639));
#25537=CARTESIAN_POINT('Ctrl Pts',(-0.238004094098004,0.0158411892598538,
0.00446430697140144));
#25538=CARTESIAN_POINT('Ctrl Pts',(-0.238014599575372,0.0160534934989504,
0.00306255012693011));
#25539=CARTESIAN_POINT('Ctrl Pts',(-0.238020318596638,0.0160609814542743,
0.00231040371210835));
#25540=CARTESIAN_POINT('Ctrl Pts',(-0.180494077221453,0.00130607217168702,
0.00717829214732417));
#25541=CARTESIAN_POINT('Ctrl Pts',(-0.180493592787613,0.0015545815750099,
0.00739357222966939));
#25542=CARTESIAN_POINT('Ctrl Pts',(-0.180493140404119,0.00181416743482917,
0.00759583454647146));
#25543=CARTESIAN_POINT('Ctrl Pts',(-0.180492713748997,0.00208357848608163,
0.00778381456156277));
#25544=CARTESIAN_POINT('Origin',(-0.18,0.0075,0.));
#25545=CARTESIAN_POINT('',(-0.18000000007387,0.00163316081088028,0.00680057000546517));
#25546=CARTESIAN_POINT('Ctrl Pts',(-0.18000000007387,0.00163316081088028,
0.00680057000546517));
#25547=CARTESIAN_POINT('Ctrl Pts',(-0.180000000073869,0.00163311910190787,
0.0068005338709428));
#25548=CARTESIAN_POINT('Ctrl Pts',(-0.180000000073867,0.00163307739326464,
0.00680049773603036));
#25549=CARTESIAN_POINT('Ctrl Pts',(-0.180000000073866,0.00163303568495152,
0.0068004616007287));
#25550=CARTESIAN_POINT('Ctrl Pts',(-0.180000000092441,0.002369415201346,
0.00737400928367846));
#25551=CARTESIAN_POINT('Ctrl Pts',(-0.180000000083634,0.00211429283077817,
0.0071959755706896));
#25552=CARTESIAN_POINT('Ctrl Pts',(-0.180000000081285,0.00186847253526104,
0.00700443205911563));
#25553=CARTESIAN_POINT('Ctrl Pts',(-0.18000000007387,0.00163316081088028,
0.00680057000546517));
#25554=CARTESIAN_POINT('',(-0.18,0.0075,-0.0079756477610481));
#25555=CARTESIAN_POINT('Origin',(-0.18,0.0075,0.));
#25556=CARTESIAN_POINT('Origin',(-0.18,0.0075,0.));
#25557=CARTESIAN_POINT('',(-0.18,0.0075,-0.0045));
#25558=CARTESIAN_POINT('Origin',(-0.18,0.0075,0.));
#25559=CARTESIAN_POINT('Origin',(-0.24,0.,0.));
#25560=CARTESIAN_POINT('',(-0.239999990168078,0.00093904782781612,0.00229080150890899));
#25561=CARTESIAN_POINT('',(-0.239999990171285,0.014060952172193,0.00229080150799885));
#25562=CARTESIAN_POINT('Ctrl Pts',(-0.239999996094951,0.00093904787461105,
0.00229080150892728));
#25563=CARTESIAN_POINT('Ctrl Pts',(-0.239999997101475,0.000948692154517853,
0.00327481805300442));
#25564=CARTESIAN_POINT('Ctrl Pts',(-0.239999998053108,0.00118441104025385,
0.00425953843427544));
#25565=CARTESIAN_POINT('Ctrl Pts',(-0.239999998922749,0.00162324794014383,
0.00514324753713933));
#25566=CARTESIAN_POINT('Ctrl Pts',(-0.239999999559175,0.0019444000203298,
0.0057899684868479));
#25567=CARTESIAN_POINT('Ctrl Pts',(-0.240000000150506,0.00237305339304198,
0.00638245831932459));
#25568=CARTESIAN_POINT('Ctrl Pts',(-0.240000000595735,0.00288415377574258,
0.00688859824331171));
#25569=CARTESIAN_POINT('Ctrl Pts',(-0.240000001209158,0.00358833160940053,
0.0075859417148971));
#25570=CARTESIAN_POINT('Ctrl Pts',(-0.240000001652703,0.00445542634564925,
0.00812227657472353));
#25571=CARTESIAN_POINT('Ctrl Pts',(-0.240000002018159,0.00539660868660465,
0.00844062167001609));
#25572=CARTESIAN_POINT('Ctrl Pts',(-0.240000002280407,0.00607199510526324,
0.0086690640710804));
#25573=CARTESIAN_POINT('Ctrl Pts',(-0.240000002506559,0.00678456933559004,
0.00878605448646416));
#25574=CARTESIAN_POINT('Ctrl Pts',(-0.240000002526878,0.0074955997506256,
0.00878612424472651));
#25575=CARTESIAN_POINT('Ctrl Pts',(-0.240000002554858,0.00847475043474964,
0.00878622030791714));
#25576=CARTESIAN_POINT('Ctrl Pts',(-0.240000002171471,0.0094577774348298,
0.00856303209124745));
#25577=CARTESIAN_POINT('Ctrl Pts',(-0.24000000179428,0.0103436536206028,
0.00813712929230807));
#25578=CARTESIAN_POINT('Ctrl Pts',(-0.240000001515866,0.0109975392046676,
0.00782276064247662));
#25579=CARTESIAN_POINT('Ctrl Pts',(-0.240000001257246,0.0115982954087712,
0.00739923147750592));
#25580=CARTESIAN_POINT('Ctrl Pts',(-0.240000000602187,0.0121128505559814,
0.00689155983415775));
#25581=CARTESIAN_POINT('Ctrl Pts',(-0.239999999683774,0.0128342721152729,
0.00617978915119394));
#25582=CARTESIAN_POINT('Ctrl Pts',(-0.23999999880627,0.0133885130222018,
0.00529542721886552));
#25583=CARTESIAN_POINT('Ctrl Pts',(-0.23999999800924,0.0137149174458767,
0.00433101787474712));
#25584=CARTESIAN_POINT('Ctrl Pts',(-0.239999997467613,0.0139367276453739,
0.00367564737882222));
#25585=CARTESIAN_POINT('Ctrl Pts',(-0.239999996808942,0.0140541566258168,
0.00298415385504518));
#25586=CARTESIAN_POINT('Ctrl Pts',(-0.239999996099761,0.0140609521253968,
0.00229080150801713));
#25587=CARTESIAN_POINT('',(-0.23999999609495,0.0140609521253889,-0.00229080150892896));
#25588=CARTESIAN_POINT('Ctrl Pts',(-0.239999978314326,0.0140609521966072,
0.00229080150800877));
#25589=CARTESIAN_POINT('Ctrl Pts',(-0.239999982890083,0.0140623369804884,
0.00214950739022427));
#25590=CARTESIAN_POINT('Ctrl Pts',(-0.239999985886701,0.0140636860354097,
0.00198109906617924));
#25591=CARTESIAN_POINT('Ctrl Pts',(-0.23999998754503,0.0140649627233419,
0.00179251014277393));
#25592=CARTESIAN_POINT('Ctrl Pts',(-0.239999988374194,0.014065601067308,
0.00169821568107128));
#25593=CARTESIAN_POINT('Ctrl Pts',(-0.23999998888584,0.0140662213195413,
0.00159887606952855));
#25594=CARTESIAN_POINT('Ctrl Pts',(-0.239999989109537,0.0140668601072055,
0.00148755770124551));
#25595=CARTESIAN_POINT('Ctrl Pts',(-0.239999989333234,0.0140674988948697,
0.00137623933296246));
#25596=CARTESIAN_POINT('Ctrl Pts',(-0.23999998921348,0.0140681562179323,
0.0012529422079391));
#25597=CARTESIAN_POINT('Ctrl Pts',(-0.239999988915679,0.014068685563465,
0.00114540075377642));
#25598=CARTESIAN_POINT('Ctrl Pts',(-0.239999988617878,0.0140692149089978,
0.00103785929961375));
#25599=CARTESIAN_POINT('Ctrl Pts',(-0.239999988207469,0.0140696162771043,
0.000946073516311766));
#25600=CARTESIAN_POINT('Ctrl Pts',(-0.239999987775988,0.0140699738331671,
0.000851201366531044));
#25601=CARTESIAN_POINT('Ctrl Pts',(-0.239999987344506,0.0140703313892298,
0.000756329216750322));
#25602=CARTESIAN_POINT('Ctrl Pts',(-0.239999986868716,0.0140706451332085,
0.00065837070049086));
#25603=CARTESIAN_POINT('Ctrl Pts',(-0.239999986453847,0.0140708940240656,
0.000562234778410537));
#25604=CARTESIAN_POINT('Ctrl Pts',(-0.239999985624108,0.0140713918057796,
0.00036996293424989));
#25605=CARTESIAN_POINT('Ctrl Pts',(-0.23999998509129,0.0140716301752879,
0.000184981466805796));
#25606=CARTESIAN_POINT('Ctrl Pts',(-0.23999998509129,0.014071630175288,
-4.55864146615709E-13));
#25607=CARTESIAN_POINT('Ctrl Pts',(-0.23999998509129,0.0140716301752881,
-0.000184981467717525));
#25608=CARTESIAN_POINT('Ctrl Pts',(-0.239999985624108,0.01407139180578,
-0.000369962934796753));
#25609=CARTESIAN_POINT('Ctrl Pts',(-0.239999986453847,0.0140708940240645,
-0.000562234779073522));
#25610=CARTESIAN_POINT('Ctrl Pts',(-0.239999986868716,0.0140706451332067,
-0.000658370701211906));
#25611=CARTESIAN_POINT('Ctrl Pts',(-0.239999987344507,0.0140703313892268,
-0.000756329217649677));
#25612=CARTESIAN_POINT('Ctrl Pts',(-0.239999987775988,0.0140699738331646,
-0.000851201367256255));
#25613=CARTESIAN_POINT('Ctrl Pts',(-0.23999998820747,0.0140696162771023,
-0.000946073516862834));
#25614=CARTESIAN_POINT('Ctrl Pts',(-0.239999988617878,0.014069214908998,
-0.00103785929963822));
#25615=CARTESIAN_POINT('Ctrl Pts',(-0.239999988915679,0.0140686855634605,
-0.00114540075468826));
#25616=CARTESIAN_POINT('Ctrl Pts',(-0.23999998921348,0.0140681562179229,
-0.00125294220973829));
#25617=CARTESIAN_POINT('Ctrl Pts',(-0.239999989333234,0.0140674988948486,
-0.00137623933706298));
#25618=CARTESIAN_POINT('Ctrl Pts',(-0.239999989109537,0.0140668601071775,
-0.00148755770664535));
#25619=CARTESIAN_POINT('Ctrl Pts',(-0.23999998888584,0.0140662213195064,
-0.00159887607622772));
#25620=CARTESIAN_POINT('Ctrl Pts',(-0.239999988374195,0.0140656010672713,
-0.00169821568806778));
#25621=CARTESIAN_POINT('Ctrl Pts',(-0.23999998754503,0.0140649627233053,
-0.00179251014966976));
#25622=CARTESIAN_POINT('Ctrl Pts',(-0.239999985886701,0.0140636860353734,
-0.00198109907287374));
#25623=CARTESIAN_POINT('Ctrl Pts',(-0.239999982890084,0.0140623369804603,
-0.00214950739512543));
#25624=CARTESIAN_POINT('Ctrl Pts',(-0.239999978314326,0.0140609521965983,
-0.00229080150892059));
#25625=CARTESIAN_POINT('',(-0.239999990171284,0.000939047827815039,-0.0022908015088178));
#25626=CARTESIAN_POINT('Ctrl Pts',(-0.23999999609495,0.0140609521253889,
-0.00229080150892896));
#25627=CARTESIAN_POINT('Ctrl Pts',(-0.239999997101474,0.0140513078454819,
-0.00327481805300426));
#25628=CARTESIAN_POINT('Ctrl Pts',(-0.239999998053107,0.0138155889597465,
-0.00425953843427357));
#25629=CARTESIAN_POINT('Ctrl Pts',(-0.239999998922749,0.0133767520598578,
-0.00514324753713624));
#25630=CARTESIAN_POINT('Ctrl Pts',(-0.239999999559175,0.0130555999797016,
-0.00578996848678572));
#25631=CARTESIAN_POINT('Ctrl Pts',(-0.240000000150506,0.0126269466070391,
-0.00638245831921348));
#25632=CARTESIAN_POINT('Ctrl Pts',(-0.240000000595735,0.0121158462244005,
-0.00688859824317014));
#25633=CARTESIAN_POINT('Ctrl Pts',(-0.240000001209157,0.0114116683907632,
-0.00758594171477775));
#25634=CARTESIAN_POINT('Ctrl Pts',(-0.240000001652703,0.0105445736545301,
-0.00812227657463066));
#25635=CARTESIAN_POINT('Ctrl Pts',(-0.240000002018158,0.0096033913135841,
-0.00844062166995183));
#25636=CARTESIAN_POINT('Ctrl Pts',(-0.240000002280407,0.00892800489499707,
-0.00866906407101473));
#25637=CARTESIAN_POINT('Ctrl Pts',(-0.240000002506559,0.00821543066474581,
-0.00878605448641982));
#25638=CARTESIAN_POINT('Ctrl Pts',(-0.240000002526877,0.00750440024977829,
-0.00878612424472624));
#25639=CARTESIAN_POINT('Ctrl Pts',(-0.240000002554857,0.0065252495656463,
-0.00878622030797757));
#25640=CARTESIAN_POINT('Ctrl Pts',(-0.240000002171471,0.00554222256554557,
-0.00856303209136526));
#25641=CARTESIAN_POINT('Ctrl Pts',(-0.240000001794279,0.00465634637974179,
-0.00813712929247474));
#25642=CARTESIAN_POINT('Ctrl Pts',(-0.240000001515865,0.00400246079572807,
-0.00782276064271482));
#25643=CARTESIAN_POINT('Ctrl Pts',(-0.240000001257246,0.0034017045916579,
-0.00739923147783583));
#25644=CARTESIAN_POINT('Ctrl Pts',(-0.240000000602186,0.00288714944445491,
-0.00689155983458874));
#25645=CARTESIAN_POINT('Ctrl Pts',(-0.239999999683773,0.00216572788509985,
-0.00617978915169404));
#25646=CARTESIAN_POINT('Ctrl Pts',(-0.239999998806269,0.00161148697809014,
-0.00529542721942));
#25647=CARTESIAN_POINT('Ctrl Pts',(-0.239999998009239,0.00128508255432472,
-0.00433101787533549));
#25648=CARTESIAN_POINT('Ctrl Pts',(-0.239999997467612,0.00106327235478633,
-0.00367564737949376));
#25649=CARTESIAN_POINT('Ctrl Pts',(-0.239999996808941,0.000945843374278495,
-0.00298415385579714));
#25650=CARTESIAN_POINT('Ctrl Pts',(-0.23999999609976,0.00093904787461117,
-0.00229080150883608));
#25651=CARTESIAN_POINT('Ctrl Pts',(-0.239999978314326,0.000939047803400774,
-0.00229080150882772));
#25652=CARTESIAN_POINT('Ctrl Pts',(-0.239999982890083,0.000937663019536478,
-0.00214950739458796));
#25653=CARTESIAN_POINT('Ctrl Pts',(-0.239999985886701,0.000936313964622287,
-0.00198109907211505));
#25654=CARTESIAN_POINT('Ctrl Pts',(-0.23999998754503,0.000935037276690134,
-0.00179251014885892));
#25655=CARTESIAN_POINT('Ctrl Pts',(-0.239999988374194,0.000934398932724057,
-0.00169821568723086));
#25656=CARTESIAN_POINT('Ctrl Pts',(-0.23999998888584,0.000933778680489091,
-0.001598876075407));
#25657=CARTESIAN_POINT('Ctrl Pts',(-0.239999989109537,0.000933139892818666,
-0.00148755770593738));
#25658=CARTESIAN_POINT('Ctrl Pts',(-0.239999989333234,0.000932501105148241,
-0.00137623933646776));
#25659=CARTESIAN_POINT('Ctrl Pts',(-0.23999998921348,0.000931843782075009,
-0.00125294220935238));
#25660=CARTESIAN_POINT('Ctrl Pts',(-0.239999988915679,0.000931314436538036,
-0.00114540075439106));
#25661=CARTESIAN_POINT('Ctrl Pts',(-0.239999988617877,0.000930785091001064,
-0.00103785929942974));
#25662=CARTESIAN_POINT('Ctrl Pts',(-0.239999988207469,0.000930383722896765,
-0.000946073516622472));
#25663=CARTESIAN_POINT('Ctrl Pts',(-0.239999987775988,0.000930026166834633,
-0.000851201367006931));
#25664=CARTESIAN_POINT('Ctrl Pts',(-0.239999987344506,0.000929668610772501,
-0.00075632921739139));
#25665=CARTESIAN_POINT('Ctrl Pts',(-0.239999986868716,0.000929354866792827,
-0.000658370700967577));
#25666=CARTESIAN_POINT('Ctrl Pts',(-0.239999986453847,0.000929105975935206,
-0.000562234778806111));
#25667=CARTESIAN_POINT('Ctrl Pts',(-0.239999985624108,0.000928608194219964,
-0.000369962934483178));
#25668=CARTESIAN_POINT('Ctrl Pts',(-0.239999985091289,0.000928369824712036,
-0.00018498146720963));
#25669=CARTESIAN_POINT('Ctrl Pts',(-0.239999985091289,0.000928369824712027,
4.55961963606762E-14));
#25670=CARTESIAN_POINT('Ctrl Pts',(-0.239999985091289,0.000928369824712017,
0.000184981467300823));
#25671=CARTESIAN_POINT('Ctrl Pts',(-0.239999985624108,0.000928608194219925,
0.000369962934537728));
#25672=CARTESIAN_POINT('Ctrl Pts',(-0.239999986453847,0.00092910597593532,
0.000562234778872252));
#25673=CARTESIAN_POINT('Ctrl Pts',(-0.239999986868716,0.000929354866793017,
0.000658370701039514));
#25674=CARTESIAN_POINT('Ctrl Pts',(-0.239999987344506,0.000929668610772811,
0.000756329217481181));
#25675=CARTESIAN_POINT('Ctrl Pts',(-0.239999987775988,0.000930026166834889,
0.000851201367079335));
#25676=CARTESIAN_POINT('Ctrl Pts',(-0.239999988207469,0.000930383722896967,
0.000946073516677489));
#25677=CARTESIAN_POINT('Ctrl Pts',(-0.239999988617877,0.000930785091001039,
0.00103785929943213));
#25678=CARTESIAN_POINT('Ctrl Pts',(-0.239999988915679,0.00093131443653849,
0.00114540075448225));
#25679=CARTESIAN_POINT('Ctrl Pts',(-0.23999998921348,0.000931843782075941,
0.00125294220953238));
#25680=CARTESIAN_POINT('Ctrl Pts',(-0.239999989333234,0.000932501105150358,
0.00137623933687799));
#25681=CARTESIAN_POINT('Ctrl Pts',(-0.239999989109537,0.000933139892821468,
0.0014875577064776));
#25682=CARTESIAN_POINT('Ctrl Pts',(-0.23999998888584,0.000933778680492577,
0.00159887607607722));
#25683=CARTESIAN_POINT('Ctrl Pts',(-0.239999988374194,0.000934398932727729,
0.00169821568793084));
#25684=CARTESIAN_POINT('Ctrl Pts',(-0.23999998754503,0.000935037276693792,
0.00179251014954883));
#25685=CARTESIAN_POINT('Ctrl Pts',(-0.239999985886701,0.000936313964625918,
0.00198109907278481));
#25686=CARTESIAN_POINT('Ctrl Pts',(-0.239999982890083,0.000937663019539288,
0.0021495073950783));
#25687=CARTESIAN_POINT('Ctrl Pts',(-0.239999978314326,0.000939047803401668,
0.00229080150891891));
#25688=CARTESIAN_POINT('Origin',(-0.238000089723382,0.000932439548048954,
8.085935608268E-7));
#25689=CARTESIAN_POINT('Ctrl Pts',(-0.239999996099768,0.000939047805433175,
-0.00229080150878961));
#25690=CARTESIAN_POINT('Ctrl Pts',(-0.240000043006653,0.000528617519648317,
-0.00229337348318028));
#25691=CARTESIAN_POINT('Ctrl Pts',(-0.239869494268692,0.000118749315230352,
-0.00229595732371585));
#25692=CARTESIAN_POINT('Ctrl Pts',(-0.239633235322195,-0.000215513325754126,
-0.00229850428565031));
#25693=CARTESIAN_POINT('Ctrl Pts',(-0.239569418327284,-0.000305802551093352,
-0.00229919225729845));
#25694=CARTESIAN_POINT('Ctrl Pts',(-0.239498166602568,-0.000390684708998686,
-0.0022998800374307));
#25695=CARTESIAN_POINT('Ctrl Pts',(-0.239420535407129,-0.000469012056432765,
-0.00230057142549143));
#25696=CARTESIAN_POINT('Ctrl Pts',(-0.239132270695065,-0.000759861760950644,
-0.00230313872822486));
#25697=CARTESIAN_POINT('Ctrl Pts',(-0.2387511004726,-0.000959690921395982,
-0.00230570344552429));
#25698=CARTESIAN_POINT('Ctrl Pts',(-0.238346576518808,-0.00103084593839461,
-0.00230827883574627));
#25699=CARTESIAN_POINT('Ctrl Pts',(-0.238238848668799,-0.00104979506841949,
-0.00230896468203286));
#25700=CARTESIAN_POINT('Ctrl Pts',(-0.238129594726146,-0.0010598784421159,
-0.00230965111096215));
#25701=CARTESIAN_POINT('Ctrl Pts',(-0.238020319825353,-0.00106098210578189,
-0.00231033750372615));
#25702=CARTESIAN_POINT('Ctrl Pts',(-0.238020319827727,-0.00106098234435247,
0.00231033750623555));
#25703=CARTESIAN_POINT('Ctrl Pts',(-0.238430653011175,-0.00105683802591466,
0.00230776006436476));
#25704=CARTESIAN_POINT('Ctrl Pts',(-0.238839618608655,-0.000922133765191787,
0.00230518882237866));
#25705=CARTESIAN_POINT('Ctrl Pts',(-0.239172040185025,-0.000681733222427424,
0.00230262217336099));
#25706=CARTESIAN_POINT('Ctrl Pts',(-0.239260566696896,-0.000617712644295366,
0.002301938654297));
#25707=CARTESIAN_POINT('Ctrl Pts',(-0.239343768351535,-0.00054646776209465,
0.00230125511985015));
#25708=CARTESIAN_POINT('Ctrl Pts',(-0.239420535523769,-0.000469012172569021,
0.00230057142670432));
#25709=CARTESIAN_POINT('Ctrl Pts',(-0.239707936442746,-0.000179033957119173,
0.00229801181648694));
#25710=CARTESIAN_POINT('Ctrl Pts',(-0.23990449768155,0.000202999713542514,
0.002295473453181));
#25711=CARTESIAN_POINT('Ctrl Pts',(-0.23997243007692,0.000607909087375879,
0.00229289178149579));
#25712=CARTESIAN_POINT('Ctrl Pts',(-0.239990779616387,0.000717281066604452,
0.00229219443398997));
#25713=CARTESIAN_POINT('Ctrl Pts',(-0.240000008778427,0.00082818455522576,
0.00229149623695115));
#25714=CARTESIAN_POINT('Ctrl Pts',(-0.239999996094959,0.000939047805435644,
0.00229080150888079));
#25715=CARTESIAN_POINT('Origin',(-0.237999996123667,0.00749999988066555,
0.00222451372646705));
#25716=CARTESIAN_POINT('Ctrl Pts',(-0.239999996099769,0.0140609521945749,
0.00229080150797066));
#25717=CARTESIAN_POINT('Ctrl Pts',(-0.240000043006654,0.0144713824803586,
0.00229337348232777));
#25718=CARTESIAN_POINT('Ctrl Pts',(-0.239869494268694,0.0148812506847756,
0.00229595732282965));
#25719=CARTESIAN_POINT('Ctrl Pts',(-0.239633235322198,0.0152155133257598,
0.002298504284731));
#25720=CARTESIAN_POINT('Ctrl Pts',(-0.239569418327287,0.015305802551099,
0.0022991922563702));
#25721=CARTESIAN_POINT('Ctrl Pts',(-0.239498166602572,0.0153906847090043,
0.00229988003649352));
#25722=CARTESIAN_POINT('Ctrl Pts',(-0.239420535407133,0.0154690120564384,
0.00230057142454528));
#25723=CARTESIAN_POINT('Ctrl Pts',(-0.239132270695066,0.0157598617609598,
0.00230313872724546));
#25724=CARTESIAN_POINT('Ctrl Pts',(-0.238751100472598,0.0159596909214074,
0.00230570344451184));
#25725=CARTESIAN_POINT('Ctrl Pts',(-0.238346576518801,0.0160308459384058,
0.00230827883470088));
#25726=CARTESIAN_POINT('Ctrl Pts',(-0.238238848668797,0.0160497950684295,
0.00230896468097866));
#25727=CARTESIAN_POINT('Ctrl Pts',(-0.238129594726149,0.0160598784421256,
0.00230965110989914));
#25728=CARTESIAN_POINT('Ctrl Pts',(-0.238020319825361,0.0160609821057921,
0.00231033750265435));
#25729=CARTESIAN_POINT('Origin',(-0.237999996123666,0.00750000011933441,
-0.00222451372646644));
#25730=CARTESIAN_POINT('Ctrl Pts',(-0.238020319827727,0.0160609823443528,
-0.00231033750623781));
#25731=CARTESIAN_POINT('Ctrl Pts',(-0.238430653011171,0.0160568380259149,
-0.00230776006436743));
#25732=CARTESIAN_POINT('Ctrl Pts',(-0.238839618608648,0.0159221337651943,
-0.00230518882238151));
#25733=CARTESIAN_POINT('Ctrl Pts',(-0.239172040185016,0.0156817332224338,
-0.00230262217336384));
#25734=CARTESIAN_POINT('Ctrl Pts',(-0.23926056669689,0.0156177126442999,
-0.00230193865429981));
#25735=CARTESIAN_POINT('Ctrl Pts',(-0.239343768351532,0.0155464677620968,
-0.00230125511985291));
#25736=CARTESIAN_POINT('Ctrl Pts',(-0.239420535523769,0.0154690121725683,
-0.00230057142670702));
#25737=CARTESIAN_POINT('Ctrl Pts',(-0.239707936442746,0.0151790339571179,
-0.00229801181648951));
#25738=CARTESIAN_POINT('Ctrl Pts',(-0.23990449768155,0.0147970002864556,
-0.00229547345318327));
#25739=CARTESIAN_POINT('Ctrl Pts',(-0.23997243007692,0.0143920909126221,
-0.00229289178149773));
#25740=CARTESIAN_POINT('Ctrl Pts',(-0.239990779616386,0.0142827189333941,
-0.00229219443399182));
#25741=CARTESIAN_POINT('Ctrl Pts',(-0.240000008778426,0.0141718154447735,
-0.00229149623695292));
#25742=CARTESIAN_POINT('Ctrl Pts',(-0.239999996094958,0.0140609521945643,
-0.00229080150888247));
#25743=CARTESIAN_POINT('Origin',(-0.238000089723382,0.0140675604519525,
-8.08593956556282E-7));
#25744=CARTESIAN_POINT('Origin',(-0.1795,0.0075,0.));
#25745=CARTESIAN_POINT('Origin',(-0.1795,0.0075,-0.0079756477610481));
#25746=CARTESIAN_POINT('Origin',(-0.1795,0.0075,0.));
#25747=CARTESIAN_POINT('Origin',(-0.1795,0.0075,-0.0045));
#25748=CARTESIAN_POINT('Origin',(-0.1405,0.0075,0.));
#25749=CARTESIAN_POINT('Origin',(-0.1405,0.0075,-0.0055));
#25750=CARTESIAN_POINT('Origin',(-0.1405,0.0075,0.));
#25751=CARTESIAN_POINT('Origin',(-0.1405,0.0075,-0.00882888901198444));
#25752=CARTESIAN_POINT('Origin',(-0.1406,0.0075,0.));
#25753=CARTESIAN_POINT('Origin',(-0.1406,0.0075,-0.00882888901198444));
#25754=CARTESIAN_POINT('Origin',(-0.1421,0.0075,0.));
#25755=CARTESIAN_POINT('Origin',(-0.1421,0.0075,-0.00882888901198444));
#25756=CARTESIAN_POINT('Origin',(-0.1419,0.0075,0.));
#25757=CARTESIAN_POINT('Origin',(-0.1419,0.0075,0.00882888901198444));
#25758=CARTESIAN_POINT('Origin',(-0.1436,0.0075,0.));
#25759=CARTESIAN_POINT('Origin',(-0.1436,0.0075,-0.00882888901198444));
#25760=CARTESIAN_POINT('Origin',(-0.1434,0.0075,0.));
#25761=CARTESIAN_POINT('Origin',(-0.1434,0.0075,0.00882888901198444));
#25762=CARTESIAN_POINT('Origin',(-0.1451,0.0075,0.));
#25763=CARTESIAN_POINT('Origin',(-0.1451,0.0075,-0.00882888901198444));
#25764=CARTESIAN_POINT('Origin',(-0.1449,0.0075,0.));
#25765=CARTESIAN_POINT('Origin',(-0.1449,0.0075,0.00882888901198444));
#25766=CARTESIAN_POINT('Origin',(-0.1464,0.0075,0.));
#25767=CARTESIAN_POINT('Origin',(-0.1464,0.0075,0.00882888901198444));
#25768=CARTESIAN_POINT('Origin',(-0.1466,0.0075,0.));
#25769=CARTESIAN_POINT('Origin',(-0.1466,0.0075,-0.00882888901198444));
#25770=CARTESIAN_POINT('Origin',(-0.1479,0.0075,0.));
#25771=CARTESIAN_POINT('Origin',(-0.1479,0.0075,0.00882888901198444));
#25772=CARTESIAN_POINT('Origin',(-0.149526465075064,0.0075,0.));
#25773=CARTESIAN_POINT('Origin',(-0.149526465075064,0.0075,-0.00882888901198444));
#25774=CARTESIAN_POINT('Origin',(-0.1595,0.0075,0.));
#25775=CARTESIAN_POINT('Origin',(-0.1595,0.0075,-0.00882888901198444));
#25776=CARTESIAN_POINT('Origin',(-0.159473534924936,0.0075,0.));
#25777=CARTESIAN_POINT('Origin',(-0.159473534924936,0.0075,0.00882888901198444));
#25778=CARTESIAN_POINT('Origin',(-0.158026465075064,0.0075,0.));
#25779=CARTESIAN_POINT('Origin',(-0.158026465075064,0.0075,-0.00882888901198444));
#25780=CARTESIAN_POINT('Origin',(-0.150973534924937,0.0075,0.));
#25781=CARTESIAN_POINT('Origin',(-0.150973534924937,0.0075,0.00882888901198444));
#25782=CARTESIAN_POINT('Ctrl Pts',(-0.180492715511507,0.00208357847138839,
0.00778381458262853));
#25783=CARTESIAN_POINT('Ctrl Pts',(-0.18,0.00208768551873161,0.00777792629190908));
#25784=CARTESIAN_POINT('Ctrl Pts',(-0.18,0.00236958913814357,0.00737375990977421));
#25785=CARTESIAN_POINT('Ctrl Pts',(-0.180494324020048,0.00106537901854582,
0.00707337168038232));
#25786=CARTESIAN_POINT('Ctrl Pts',(-0.18,0.00106751218715109,0.00706776299687777));
#25787=CARTESIAN_POINT('Ctrl Pts',(-0.18,0.0014052360688775,0.00670086601600097));
#25788=CARTESIAN_POINT('Ctrl Pts',(-0.180498282439035,-0.000688149212900568,
0.00524596704164286));
#25789=CARTESIAN_POINT('Ctrl Pts',(-0.18,-0.000692161918799494,0.00523579826232968));
#25790=CARTESIAN_POINT('Ctrl Pts',(-0.18,-0.000255396373108266,0.00497022946835977));
#25791=CARTESIAN_POINT('Ctrl Pts',(-0.180508571884256,-0.00206121245391611,
0.00171196042612565));
#25792=CARTESIAN_POINT('Ctrl Pts',(-0.18,-0.00207089065980965,0.0017061119940659));
#25793=CARTESIAN_POINT('Ctrl Pts',(-0.18,-0.00155636923028695,0.001622484125152));
#25794=CARTESIAN_POINT('Ctrl Pts',(-0.180507701632299,-0.00198984920249958,
-0.00207534072170255));
#25795=CARTESIAN_POINT('Ctrl Pts',(-0.18,-0.00199898872775875,-0.00206848014615668));
#25796=CARTESIAN_POINT('Ctrl Pts',(-0.18,-0.0014886043286521,-0.00196703616742313));
#25797=CARTESIAN_POINT('Ctrl Pts',(-0.180497559880866,-0.000482912630366871,
-0.00555392798696781));
#25798=CARTESIAN_POINT('Ctrl Pts',(-0.18,-0.000486526972169703,-0.00554405840433583));
#25799=CARTESIAN_POINT('Ctrl Pts',(-0.18,-6.11665353613021E-5,-0.00526163542994926));
#25800=CARTESIAN_POINT('Ctrl Pts',(-0.180491867056987,0.00224576313070539,
-0.0081898374281038));
#25801=CARTESIAN_POINT('Ctrl Pts',(-0.18,0.00224601031558402,-0.00818083867958575));
#25802=CARTESIAN_POINT('Ctrl Pts',(-0.18,0.00252313449484398,-0.00775830380791825));
#25803=CARTESIAN_POINT('Ctrl Pts',(-0.180488462887617,0.00577942932125372,
-0.00958054386633694));
#25804=CARTESIAN_POINT('Ctrl Pts',(-0.18,0.00577937831377157,-0.00956893262499887));
#25805=CARTESIAN_POINT('Ctrl Pts',(-0.18,0.00587025317906997,-0.00907572435223234));
#25806=CARTESIAN_POINT('Ctrl Pts',(-0.180488629342552,0.00957710911122243,
-0.00950944489475148));
#25807=CARTESIAN_POINT('Ctrl Pts',(-0.18,0.00957712259305036,-0.00949788380666547));
#25808=CARTESIAN_POINT('Ctrl Pts',(-0.18,0.0094675316846421,-0.00900837007444288));
#25809=CARTESIAN_POINT('Ctrl Pts',(-0.180492343722264,0.0130567083237039,
-0.00798771374964044));
#25810=CARTESIAN_POINT('Ctrl Pts',(-0.18,0.0130566470856787,-0.00797903414015096));
#25811=CARTESIAN_POINT('Ctrl Pts',(-0.18,0.0127633603172519,-0.00756679005675688));
#25812=CARTESIAN_POINT('Ctrl Pts',(-0.180498277776074,0.0156878479525759,
-0.00524728696109442));
#25813=CARTESIAN_POINT('Ctrl Pts',(-0.18,0.0156918696359066,-0.00523708434816095));
#25814=CARTESIAN_POINT('Ctrl Pts',(-0.18,0.0152551103542225,-0.00497147978047479));
#25815=CARTESIAN_POINT('Ctrl Pts',(-0.180508590057067,0.0170631420237172,
-0.00170670572622402));
#25816=CARTESIAN_POINT('Ctrl Pts',(-0.18,0.0170728417288127,-0.00170085628138549));
#25817=CARTESIAN_POINT('Ctrl Pts',(-0.18,0.0165581992152197,-0.00161750652259339));
#25818=CARTESIAN_POINT('Ctrl Pts',(-0.180507676294974,0.0169879516360366,
0.00208672420876621));
#25819=CARTESIAN_POINT('Ctrl Pts',(-0.18,0.0169970776392087,0.00207981994539201));
#25820=CARTESIAN_POINT('Ctrl Pts',(-0.18,0.0164868018720009,0.00197783354485042));
#25821=CARTESIAN_POINT('Ctrl Pts',(-0.180497532146321,0.0154750030588555,
0.00556552633006958));
#25822=CARTESIAN_POINT('Ctrl Pts',(-0.18,0.0154786081176936,0.00555565825322737));
#25823=CARTESIAN_POINT('Ctrl Pts',(-0.18,0.0150536805229185,0.00527261080601529));
#25824=CARTESIAN_POINT('Ctrl Pts',(-0.180491851706073,0.0127430969971975,
0.00819641820051746));
#25825=CARTESIAN_POINT('Ctrl Pts',(-0.18,0.0127428333825127,0.00818741797918455));
#25826=CARTESIAN_POINT('Ctrl Pts',(-0.18,0.01246631245657,0.00776454042759482));
#25827=CARTESIAN_POINT('Ctrl Pts',(-0.180488461754297,0.00921325615876769,
0.00958099954636007));
#25828=CARTESIAN_POINT('Ctrl Pts',(-0.18,0.00921330243936221,0.00956938959009847));
#25829=CARTESIAN_POINT('Ctrl Pts',(-0.18,0.00912281682762101,0.00907615564159787));
#25830=CARTESIAN_POINT('Ctrl Pts',(-0.18048863138779,0.00542104750415485,
0.00950862445512012));
#25831=CARTESIAN_POINT('Ctrl Pts',(-0.18,0.00542103959480098,0.00949706815102514));
#25832=CARTESIAN_POINT('Ctrl Pts',(-0.18,0.00553072204248816,0.00900759283099922));
#25833=CARTESIAN_POINT('Ctrl Pts',(-0.180491107002967,0.00310177792423096,
0.00849425748487474));
#25834=CARTESIAN_POINT('Ctrl Pts',(-0.18,0.00310463170987884,0.00848584310919716));
#25835=CARTESIAN_POINT('Ctrl Pts',(-0.18,0.00333394220740964,0.00804665380354745));
#25836=CARTESIAN_POINT('Ctrl Pts',(-0.180492715511507,0.00208357847138839,
0.00778381458262853));
#25837=CARTESIAN_POINT('Ctrl Pts',(-0.18,0.00208768551873161,0.00777792629190908));
#25838=CARTESIAN_POINT('Ctrl Pts',(-0.18,0.00236958913814357,0.00737375990977421));
#25839=CARTESIAN_POINT('',(0.,0.,0.));
#25840=CARTESIAN_POINT('Origin',(-0.00333123939879042,-0.00899999999999701,
0.));
#25841=CARTESIAN_POINT('',(-0.00333123939879042,-0.00779999999999701,-1.47348101581732E-35));
#25842=CARTESIAN_POINT('',(-0.00333123939879042,-0.010199999999997,0.));
#25843=CARTESIAN_POINT('Origin',(-0.00333123939879042,-0.00899999999999701,
0.));
#25844=CARTESIAN_POINT('',(0.,0.,0.));
#25845=CARTESIAN_POINT('Ctrl Pts',(-0.185819463593633,0.0166104930553049,
0.00236863820262676));
#25846=CARTESIAN_POINT('Ctrl Pts',(-0.203223508587672,0.0164247592890707,
0.00234416866113263));
#25847=CARTESIAN_POINT('Ctrl Pts',(-0.220627582451438,0.0162418056983084,
0.00231971009381821));
#25848=CARTESIAN_POINT('Ctrl Pts',(-0.238031675744303,0.0160611171225611,
0.00229373846137714));
#25849=CARTESIAN_POINT('Ctrl Pts',(-0.18581926440362,0.0166461165277183,
0.00221607060080922));
#25850=CARTESIAN_POINT('Ctrl Pts',(-0.203223313044138,0.0164497831264032,
0.00218726310900855));
#25851=CARTESIAN_POINT('Ctrl Pts',(-0.220627389279833,0.0162559154123599,
0.00215868502272393));
#25852=CARTESIAN_POINT('Ctrl Pts',(-0.238031485810861,0.0160641905057161,
0.0021289558365353));
#25853=CARTESIAN_POINT('Ctrl Pts',(-0.185818880874426,0.0167106984888996,
0.00190682671781972));
#25854=CARTESIAN_POINT('Ctrl Pts',(-0.203222934036142,0.0164938099422013,
0.00186885154579339));
#25855=CARTESIAN_POINT('Ctrl Pts',(-0.220627006269502,0.016278128585195,
0.00183193650018925));
#25856=CARTESIAN_POINT('Ctrl Pts',(-0.238031099947329,0.0160640878015832,
0.00179531454904686));
#25857=CARTESIAN_POINT('Ctrl Pts',(-0.185818335405062,0.0168157482814852,
0.00126613919744405));
#25858=CARTESIAN_POINT('Ctrl Pts',(-0.203222383696577,0.0165663597906042,
0.00122992539721983));
#25859=CARTESIAN_POINT('Ctrl Pts',(-0.220626440719063,0.016317358802535,
0.00119476376827596));
#25860=CARTESIAN_POINT('Ctrl Pts',(-0.238030512988197,0.0160691276034975,
0.00116079870997399));
#25861=CARTESIAN_POINT('Ctrl Pts',(-0.185817827209109,0.0169242355148058,
9.8641936611403E-5));
#25862=CARTESIAN_POINT('Ctrl Pts',(-0.203221858920215,0.0166409437466787,
9.11218039920294E-5));
#25863=CARTESIAN_POINT('Ctrl Pts',(-0.220625885580743,0.0163575362327447,
8.39196676156386E-5));
#25864=CARTESIAN_POINT('Ctrl Pts',(-0.238029902001653,0.0160736640759679,
7.73368998092213E-5));
#25865=CARTESIAN_POINT('Ctrl Pts',(-0.185818130580629,0.0168405937503755,
-0.00127155898818726));
#25866=CARTESIAN_POINT('Ctrl Pts',(-0.20322218710562,0.0165814424082619,
-0.00122048351610829));
#25867=CARTESIAN_POINT('Ctrl Pts',(-0.220626248932598,0.0163217805675101,
-0.0011714081373514));
#25868=CARTESIAN_POINT('Ctrl Pts',(-0.238030331796423,0.0160627645050436,
-0.00112492380137579));
#25869=CARTESIAN_POINT('Ctrl Pts',(-0.185819629874682,0.0165908497836556,
-0.00251327778772927));
#25870=CARTESIAN_POINT('Ctrl Pts',(-0.203223673996629,0.0164148787644927,
-0.00249147144795656));
#25871=CARTESIAN_POINT('Ctrl Pts',(-0.220627751907747,0.0162423115134214,
-0.00246930645840148));
#25872=CARTESIAN_POINT('Ctrl Pts',(-0.238031849291733,0.0160723190230807,
-0.00244485415145052));
#25873=CARTESIAN_POINT('Ctrl Pts',(-0.185821321884765,0.016234179304769,
-0.00369798898814236));
#25874=CARTESIAN_POINT('Ctrl Pts',(-0.203225319480993,0.0161450945583953,
-0.00371151425360031));
#25875=CARTESIAN_POINT('Ctrl Pts',(-0.220629323053567,0.0160579626760164,
-0.0037253545768972));
#25876=CARTESIAN_POINT('Ctrl Pts',(-0.238033334942443,0.0159726607261184,
-0.00373864195256771));
#25877=CARTESIAN_POINT('Ctrl Pts',(-0.185823245401148,0.0155679236134438,
-0.00510694903431088));
#25878=CARTESIAN_POINT('Ctrl Pts',(-0.203227224653483,0.0155630775790093,
-0.00518221799309441));
#25879=CARTESIAN_POINT('Ctrl Pts',(-0.220631203569159,0.0155602580016752,
-0.00525755181874107));
#25880=CARTESIAN_POINT('Ctrl Pts',(-0.238035184380882,0.0155591988240479,
-0.00533210507472633));
#25881=CARTESIAN_POINT('Ctrl Pts',(-0.185825309557818,0.0144549166529026,
-0.00659829769408909));
#25882=CARTESIAN_POINT('Ctrl Pts',(-0.203229286524981,0.0145155596341981,
-0.00676015088892623));
#25883=CARTESIAN_POINT('Ctrl Pts',(-0.22063325576454,0.0145775956365756,
-0.00692214625038456));
#25884=CARTESIAN_POINT('Ctrl Pts',(-0.238037222353744,0.0146408934228599,
-0.00708388886226514));
#25885=CARTESIAN_POINT('Ctrl Pts',(-0.185827024933535,0.0130736100782548,
-0.00784141832828519));
#25886=CARTESIAN_POINT('Ctrl Pts',(-0.203231018325486,0.0131627927804585,
-0.00809004931086922));
#25887=CARTESIAN_POINT('Ctrl Pts',(-0.220635004750871,0.0132529981228345,
-0.00833876091410667));
#25888=CARTESIAN_POINT('Ctrl Pts',(-0.238038987871232,0.0133440928006999,
-0.00858734922546909));
#25889=CARTESIAN_POINT('Ctrl Pts',(-0.18582832438757,0.0114765605098063,
-0.00878674958056091));
#25890=CARTESIAN_POINT('Ctrl Pts',(-0.203232338232321,0.0115609317972438,
-0.00910975493295771));
#25891=CARTESIAN_POINT('Ctrl Pts',(-0.220636347717917,0.011645972461393,
-0.00943280869850027));
#25892=CARTESIAN_POINT('Ctrl Pts',(-0.238040354954934,0.011731574352546,
-0.00975583575545302));
#25893=CARTESIAN_POINT('Ctrl Pts',(-0.185829453345315,0.0091451966229997,
-0.0096057242773119));
#25894=CARTESIAN_POINT('Ctrl Pts',(-0.203233491880005,0.00919013323193661,
-0.00999827176177371));
#25895=CARTESIAN_POINT('Ctrl Pts',(-0.220637530309762,0.00923531471374497,
-0.010390817424762));
#25896=CARTESIAN_POINT('Ctrl Pts',(-0.23804156864792,0.00928068353228921,
-0.0107833654056958));
#25897=CARTESIAN_POINT('Ctrl Pts',(-0.185829632293992,0.00601552622584051,
-0.00973743542872093));
#25898=CARTESIAN_POINT('Ctrl Pts',(-0.203233675322875,0.00597352188698778,
-0.0101422781507738));
#25899=CARTESIAN_POINT('Ctrl Pts',(-0.220637719137517,0.00593129183613322,
-0.0105471134497117));
#25900=CARTESIAN_POINT('Ctrl Pts',(-0.238041763362071,0.00588889329790392,
-0.0109519477983446));
#25901=CARTESIAN_POINT('Ctrl Pts',(-0.185828144842012,0.0030739290209801,
-0.00865481883805552));
#25902=CARTESIAN_POINT('Ctrl Pts',(-0.203232153522101,0.0029784477533647,
-0.00896475560878426));
#25903=CARTESIAN_POINT('Ctrl Pts',(-0.22063615670017,0.00288224573504626,
-0.00927474912637149));
#25904=CARTESIAN_POINT('Ctrl Pts',(-0.23804015699596,0.00278543581335185,
-0.00958473005637672));
#25905=CARTESIAN_POINT('Ctrl Pts',(-0.185826082022641,0.00110130832095057,
-0.00715935834428723));
#25906=CARTESIAN_POINT('Ctrl Pts',(-0.203230064435315,0.00102431113527,
-0.00735889669894074));
#25907=CARTESIAN_POINT('Ctrl Pts',(-0.220634039193033,0.000946044449726581,
-0.00755853937500263));
#25908=CARTESIAN_POINT('Ctrl Pts',(-0.238038010705833,0.000866655562235164,
-0.00775795997137017));
#25909=CARTESIAN_POINT('Ctrl Pts',(-0.185824164055499,-0.00013244480670859,
-0.0057658502018965));
#25910=CARTESIAN_POINT('Ctrl Pts',(-0.20322813912978,-0.000160334959886128,
-0.00587671276434198));
#25911=CARTESIAN_POINT('Ctrl Pts',(-0.220632108537853,-0.000189837833944718,
-0.0059877445582653));
#25912=CARTESIAN_POINT('Ctrl Pts',(-0.238036077190852,-0.000220820008254192,
-0.00609839080888522));
#25913=CARTESIAN_POINT('Ctrl Pts',(-0.185822299173595,-0.000912009378582172,
-0.00442360049681092));
#25914=CARTESIAN_POINT('Ctrl Pts',(-0.203226287658242,-0.000866786568362782,
-0.00446783414154759));
#25915=CARTESIAN_POINT('Ctrl Pts',(-0.220630281624252,-0.00082387334949089,
-0.00451207377872994));
#25916=CARTESIAN_POINT('Ctrl Pts',(-0.23803428087264,-0.000782904229550054,
-0.00455527877134414));
#25917=CARTESIAN_POINT('Ctrl Pts',(-0.185820718130017,-0.00137009218103609,
-0.00326760896710645));
#25918=CARTESIAN_POINT('Ctrl Pts',(-0.203224730158278,-0.00125053240292857,
-0.00326719962044019));
#25919=CARTESIAN_POINT('Ctrl Pts',(-0.220628754805288,-0.00113312156821255,
-0.00326706607813972));
#25920=CARTESIAN_POINT('Ctrl Pts',(-0.23803279135031,-0.00101767765869665,
-0.00326612878115765));
#25921=CARTESIAN_POINT('Ctrl Pts',(-0.185819647933685,-0.00158153457958364,
-0.00252531449976026));
#25922=CARTESIAN_POINT('Ctrl Pts',(-0.203223692052988,-0.00140575636354931,
-0.00250567473614365));
#25923=CARTESIAN_POINT('Ctrl Pts',(-0.220627772291069,-0.00123370234183487,
-0.00248543365897305));
#25924=CARTESIAN_POINT('Ctrl Pts',(-0.238031871675392,-0.001064293369006,
-0.00246259728183289));
#25925=CARTESIAN_POINT('Ctrl Pts',(-0.185818880874262,-0.00171069848643351,
-0.00190682671492207));
#25926=CARTESIAN_POINT('Ctrl Pts',(-0.203222934035982,-0.0014938099322336,
-0.00186885153402852));
#25927=CARTESIAN_POINT('Ctrl Pts',(-0.220627006269333,-0.00127812856598612,
-0.00183193647922556));
#25928=CARTESIAN_POINT('Ctrl Pts',(-0.238031099947143,-0.00106408777175675,
-0.00179531451994465));
#25929=CARTESIAN_POINT('Ctrl Pts',(-0.185818335405171,-0.0018157482831674,
-0.00126613919912989));
#25930=CARTESIAN_POINT('Ctrl Pts',(-0.203222383696684,-0.00156635979742609,
-0.00122992540382135));
#25931=CARTESIAN_POINT('Ctrl Pts',(-0.220626440719173,-0.00131735881546124,
-0.00119476377996408));
#25932=CARTESIAN_POINT('Ctrl Pts',(-0.238030512988314,-0.00106912762331005,
-0.00116079872610497));
#25933=CARTESIAN_POINT('Ctrl Pts',(-0.185817827208834,-0.00192423551004945,
-9.86419358357781E-5));
#25934=CARTESIAN_POINT('Ctrl Pts',(-0.203221858919953,-0.00164094372766557,
-9.11218007194661E-5));
#25935=CARTESIAN_POINT('Ctrl Pts',(-0.220625885580502,-0.00135753619911081,
-8.39196619480522E-5));
#25936=CARTESIAN_POINT('Ctrl Pts',(-0.238029902001436,-0.00107366402718548,
-7.73368926939811E-5));
#25937=CARTESIAN_POINT('Ctrl Pts',(-0.185818130581901,-0.00184059377323484,
0.00127155899038818));
#25938=CARTESIAN_POINT('Ctrl Pts',(-0.20322218710682,-0.00158144249928501,
0.00122048352511737));
#25939=CARTESIAN_POINT('Ctrl Pts',(-0.220626248933645,-0.00132178072462663,
0.0011714081546043));
#25940=CARTESIAN_POINT('Ctrl Pts',(-0.238030331797288,-0.00106276472807202,
0.00112492383001885));
#25941=CARTESIAN_POINT('Ctrl Pts',(-0.185819629872525,-0.00159084974486086,
0.00251327778358106));
#25942=CARTESIAN_POINT('Ctrl Pts',(-0.203223673994595,-0.00141487860996912,
0.00249147143135548));
#25943=CARTESIAN_POINT('Ctrl Pts',(-0.220627751905974,-0.00124231124688325,
0.00246930642685937));
#25944=CARTESIAN_POINT('Ctrl Pts',(-0.238031849290273,-0.00107231864497727,
0.00244485409969644));
#25945=CARTESIAN_POINT('Ctrl Pts',(-0.185821321898498,-0.00123417951568875,
0.00369798917224086));
#25946=CARTESIAN_POINT('Ctrl Pts',(-0.203225319494204,-0.00114509540859564,
0.003711514992569));
#25947=CARTESIAN_POINT('Ctrl Pts',(-0.22062932306665,-0.00105796426044417,
0.00372535589828007));
#25948=CARTESIAN_POINT('Ctrl Pts',(-0.238033334955726,-0.000972663126262614,
0.00373864380762799));
#25949=CARTESIAN_POINT('Ctrl Pts',(-0.185823245436368,-0.000567924396732498,
0.00510694905821607));
#25950=CARTESIAN_POINT('Ctrl Pts',(-0.203227224690427,-0.000563080693363035,
0.00518221807967137));
#25951=CARTESIAN_POINT('Ctrl Pts',(-0.220631203607128,-0.000560263335972913,
0.00525755189961067));
#25952=CARTESIAN_POINT('Ctrl Pts',(-0.238035184419129,-0.000559206262722732,
0.00533210518716677));
#25953=CARTESIAN_POINT('Ctrl Pts',(-0.185825309451763,0.000545085685742881,
0.00659829745055551));
#25954=CARTESIAN_POINT('Ctrl Pts',(-0.203229286420574,0.000484449699432902,
0.00676014989093362));
#25955=CARTESIAN_POINT('Ctrl Pts',(-0.220633255665466,0.000422420785569872,
0.00692214425104443));
#25956=CARTESIAN_POINT('Ctrl Pts',(-0.238037222262465,0.000359130275923251,
0.00708388576133197));
#25957=CARTESIAN_POINT('Ctrl Pts',(-0.18582702479622,0.00192639486310074,
0.00784141870119505));
#25958=CARTESIAN_POINT('Ctrl Pts',(-0.203231018176613,0.00183722692142162,
0.00809005081566443));
#25959=CARTESIAN_POINT('Ctrl Pts',(-0.22063500458984,0.00174703627304292,
0.00833876365528797));
#25960=CARTESIAN_POINT('Ctrl Pts',(-0.238038987697963,0.00165595618969436,
0.00858735323957588));
#25961=CARTESIAN_POINT('Ctrl Pts',(-0.185828324413572,0.00352344076961579,
0.00878675040966002));
#25962=CARTESIAN_POINT('Ctrl Pts',(-0.203232338254504,0.00343907331273139,
0.00910975824932868));
#25963=CARTESIAN_POINT('Ctrl Pts',(-0.220636347734676,0.00335403651878359,
0.00943281459138894));
#25964=CARTESIAN_POINT('Ctrl Pts',(-0.238040354964937,0.00326843848901562,
0.00975584429234039));
#25965=CARTESIAN_POINT('Ctrl Pts',(-0.185829453384424,0.00585480099283502,
0.00960572462550227));
#25966=CARTESIAN_POINT('Ctrl Pts',(-0.203233491922009,0.00580985725942693,
0.00999827314311295));
#25967=CARTESIAN_POINT('Ctrl Pts',(-0.220637530355488,0.00576466867020715,
0.0103908197967745));
#25968=CARTESIAN_POINT('Ctrl Pts',(-0.238041568698001,0.00571929278241239,
0.01078336873748));
#25969=CARTESIAN_POINT('Ctrl Pts',(-0.185829632324535,0.00898447703279034,
0.00973743551044517));
#25970=CARTESIAN_POINT('Ctrl Pts',(-0.20323367535712,0.00902649110858287,
0.0101422784667701));
#25971=CARTESIAN_POINT('Ctrl Pts',(-0.220637719176512,0.00906873086433049,
0.0105471139309657));
#25972=CARTESIAN_POINT('Ctrl Pts',(-0.238041763406542,0.00911113903768637,
0.0109519484055942));
#25973=CARTESIAN_POINT('Ctrl Pts',(-0.185828144821879,0.0119260676124901,
0.00865481978154805));
#25974=CARTESIAN_POINT('Ctrl Pts',(-0.203232153491178,0.0120215388163693,
0.00896475940006844));
#25975=CARTESIAN_POINT('Ctrl Pts',(-0.220636156655006,0.0121177307814799,
0.00927475599174944));
#25976=CARTESIAN_POINT('Ctrl Pts',(-0.238040156934043,0.0122145307595023,
0.00958474013175701));
#25977=CARTESIAN_POINT('Ctrl Pts',(-0.185826081864447,0.0138986875060143,
0.0071593582727713));
#25978=CARTESIAN_POINT('Ctrl Pts',(-0.203230064272376,0.0139756722252048,
0.00735889640414339));
#25979=CARTESIAN_POINT('Ctrl Pts',(-0.22063403902823,0.0140539264607635,
0.00755853873522353));
#25980=CARTESIAN_POINT('Ctrl Pts',(-0.238038010541502,0.0141333028562059,
0.00775795890451245));
#25981=CARTESIAN_POINT('Ctrl Pts',(-0.185824164045733,0.0151324448001649,
0.00576585000582876));
#25982=CARTESIAN_POINT('Ctrl Pts',(-0.203228139124408,0.0151603349181088,
0.00587671195695743));
#25983=CARTESIAN_POINT('Ctrl Pts',(-0.220632108538343,0.0151898375748212,
0.00598774292639455));
#25984=CARTESIAN_POINT('Ctrl Pts',(-0.238036077197705,0.0152208192897305,
0.00609838833446442));
#25985=CARTESIAN_POINT('Ctrl Pts',(-0.185822299200829,0.01591200987427,
0.00442360064358258));
#25986=CARTESIAN_POINT('Ctrl Pts',(-0.203226287685109,0.0158667885469009,
0.00446783472845091));
#25987=CARTESIAN_POINT('Ctrl Pts',(-0.220630281650178,0.0158238768216512,
0.00451207481602829));
#25988=CARTESIAN_POINT('Ctrl Pts',(-0.238034280897302,0.0157829092105071,
0.00455528026393975));
#25989=CARTESIAN_POINT('Ctrl Pts',(-0.185820718137045,0.0163700922862437,
0.00326760909611432));
#25990=CARTESIAN_POINT('Ctrl Pts',(-0.203224730165169,0.0162505328296095,
0.00326720013800919));
#25991=CARTESIAN_POINT('Ctrl Pts',(-0.220628754812585,0.0161331223929292,
0.00326706699899929));
#25992=CARTESIAN_POINT('Ctrl Pts',(-0.238032791358368,0.016017678941859,
0.00326613005920909));
#25993=CARTESIAN_POINT('Ctrl Pts',(-0.18581986197366,0.0165392461104783,
0.00267377340626184));
#25994=CARTESIAN_POINT('Ctrl Pts',(-0.203223899674741,0.0163747116144059,
0.00265797976538081));
#25995=CARTESIAN_POINT('Ctrl Pts',(-0.220627968794648,0.0162135862702056,
0.00264176023600675));
#25996=CARTESIAN_POINT('Ctrl Pts',(-0.238032055611188,0.016054970356251,
0.00262330371106081));
#25997=CARTESIAN_POINT('Ctrl Pts',(-0.185819463593633,0.0166104930553049,
0.00236863820262676));
#25998=CARTESIAN_POINT('Ctrl Pts',(-0.203223508587672,0.0164247592890707,
0.00234416866113263));
#25999=CARTESIAN_POINT('Ctrl Pts',(-0.220627582451438,0.0162418056983084,
0.00231971009381821));
#26000=CARTESIAN_POINT('Ctrl Pts',(-0.238031675744303,0.0160611171225611,
0.00229373846137714));
#26001=CARTESIAN_POINT('',(-0.220091864350141,0.0162481906744713,0.00232003547938548));
#26002=CARTESIAN_POINT('',(-0.230613780455036,0.0161371732180366,0.00230566860537552));
#26003=CARTESIAN_POINT('Ctrl Pts',(-0.220091864350141,0.0162481906744713,
0.00232003547938548));
#26004=CARTESIAN_POINT('Ctrl Pts',(-0.223599172161426,0.0162114519962125,
0.0023149748956921));
#26005=CARTESIAN_POINT('Ctrl Pts',(-0.227106480893481,0.016174812491324,
0.00230987413069827));
#26006=CARTESIAN_POINT('Ctrl Pts',(-0.230613790469045,0.0161382679437046,
0.00230472071158295));
#26007=CARTESIAN_POINT('',(-0.21500029174819,0.0153240929662069,0.00555316308125546));
#26008=CARTESIAN_POINT('Ctrl Pts',(-0.220091864350141,0.0162481906744713,
0.00232003547938548));
#26009=CARTESIAN_POINT('Ctrl Pts',(-0.219964032121089,0.0162246503855585,
0.00259808795516262));
#26010=CARTESIAN_POINT('Ctrl Pts',(-0.219813080900817,0.0161920738263575,
0.002863235307656));
#26011=CARTESIAN_POINT('Ctrl Pts',(-0.219641753631267,0.016149773489234,
0.00311424188670563));
#26012=CARTESIAN_POINT('Ctrl Pts',(-0.219606803621251,0.0161411444063679,
0.00316544612567476));
#26013=CARTESIAN_POINT('Ctrl Pts',(-0.219571005329045,0.0161321311914261,
0.003216013187459));
#26014=CARTESIAN_POINT('Ctrl Pts',(-0.219534386818884,0.01612274284289,
0.00326596109874446));
#26015=CARTESIAN_POINT('Ctrl Pts',(-0.219355791305947,0.016076954062432,
0.00350956666317138));
#26016=CARTESIAN_POINT('Ctrl Pts',(-0.21915768525195,0.0160222778157506,
0.00373830735842303));
#26017=CARTESIAN_POINT('Ctrl Pts',(-0.218943331145544,0.0159637685900893,
0.00394877190880269));
#26018=CARTESIAN_POINT('Ctrl Pts',(-0.21885802655045,0.0159404841945253,
0.00403252861191818));
#26019=CARTESIAN_POINT('Ctrl Pts',(-0.218770149187462,0.0159165696614574,
0.00411347490234016));
#26020=CARTESIAN_POINT('Ctrl Pts',(-0.218679854877443,0.0158923302275234,
0.00419142907760536));
#26021=CARTESIAN_POINT('Ctrl Pts',(-0.218223322396706,0.0157697744551469,
0.00458556922896357));
#26022=CARTESIAN_POINT('Ctrl Pts',(-0.217705003227418,0.0156391436947526,
0.00490281618706478));
#26023=CARTESIAN_POINT('Ctrl Pts',(-0.217145035305693,0.0155351186744745,
0.00513162883065141));
#26024=CARTESIAN_POINT('Ctrl Pts',(-0.216474315366188,0.0154105192954726,
0.00540569667723717));
#26025=CARTESIAN_POINT('Ctrl Pts',(-0.215743833615192,0.0153264023738546,
0.00555341322890043));
#26026=CARTESIAN_POINT('Ctrl Pts',(-0.21500029174819,0.0153240929662069,
0.00555316308125546));
#26027=CARTESIAN_POINT('',(-0.192201188944086,0.015241534078835,0.00554549074872928));
#26028=CARTESIAN_POINT('Ctrl Pts',(-0.192201188944086,0.015241534078835,
0.00554549074872928));
#26029=CARTESIAN_POINT('Ctrl Pts',(-0.192678589700584,0.0152435315770371,
0.00554564496900607));
#26030=CARTESIAN_POINT('Ctrl Pts',(-0.193156755420166,0.0152455145072555,
0.00554579898090145));
#26031=CARTESIAN_POINT('Ctrl Pts',(-0.193630507624624,0.0152474620561553,
0.00554595109465557));
#26032=CARTESIAN_POINT('Ctrl Pts',(-0.194104259909824,0.0152494096053871,
0.00554610320843563));
#26033=CARTESIAN_POINT('Ctrl Pts',(-0.194573598676706,0.0152513221215489,
0.0055462536667817));
#26034=CARTESIAN_POINT('Ctrl Pts',(-0.195054059361393,0.0152532621127367,
0.00554640792672152));
#26035=CARTESIAN_POINT('Ctrl Pts',(-0.195294289703737,0.0152542321083306,
0.00554648505669144));
#26036=CARTESIAN_POINT('Ctrl Pts',(-0.195537300526605,0.015255208744483,
0.00554656298160729));
#26037=CARTESIAN_POINT('Ctrl Pts',(-0.195763672529165,0.0152561146772,0.00554663556632508));
#26038=CARTESIAN_POINT('Ctrl Pts',(-0.195990044531725,0.0152570206099169,
0.00554670815104287));
#26039=CARTESIAN_POINT('Ctrl Pts',(-0.196199777712581,0.0152578561399587,
0.00554677559870816));
#26040=CARTESIAN_POINT('Ctrl Pts',(-0.196410704370724,0.0152586930485431,
0.00554684374511567));
#26041=CARTESIAN_POINT('Ctrl Pts',(-0.19683255768701,0.0152603668657118,
0.00554698003793067));
#26042=CARTESIAN_POINT('Ctrl Pts',(-0.197259184915049,0.0152620456340052,
0.00554711874688127));
#26043=CARTESIAN_POINT('Ctrl Pts',(-0.197689893504854,0.0152637260387762,
0.00554725953304577));
#26044=CARTESIAN_POINT('Ctrl Pts',(-0.198551310684465,0.0152670868483182,
0.00554754110537476));
#26045=CARTESIAN_POINT('Ctrl Pts',(-0.199429053310939,0.0152704542694656,
0.00554783101954003));
#26046=CARTESIAN_POINT('Ctrl Pts',(-0.200323661272974,0.0152738264707178,
0.00554812786352896));
#26047=CARTESIAN_POINT('Ctrl Pts',(-0.201218269235009,0.01527719867197,
0.0055484247075179));
#26048=CARTESIAN_POINT('Ctrl Pts',(-0.2021297425327,0.0152805756302453,
0.00554872846691666));
#26049=CARTESIAN_POINT('Ctrl Pts',(-0.2030579484167,0.0152839525550071,
0.00554903797343471));
#26050=CARTESIAN_POINT('Ctrl Pts',(-0.204914360184699,0.0152907064045306,
0.00554965698647082));
#26051=CARTESIAN_POINT('Ctrl Pts',(-0.206837702298988,0.0152974601561509,
0.00555029886425079));
#26052=CARTESIAN_POINT('Ctrl Pts',(-0.208828081024599,0.0153041762029342,
0.00555096151666457));
#26053=CARTESIAN_POINT('Ctrl Pts',(-0.21081845965904,0.0153108922494098,
0.00555162416904801));
#26054=CARTESIAN_POINT('Ctrl Pts',(-0.212875874899139,0.015317570478775,
0.00555230751522824));
#26055=CARTESIAN_POINT('Ctrl Pts',(-0.215000291390286,0.0153241679289001,
0.00555302111108408));
#26056=CARTESIAN_POINT('',(-0.186146181814525,0.00833801480660534,0.00957679076147885));
#26057=CARTESIAN_POINT('Ctrl Pts',(-0.192201188668275,0.0152415940904861,
0.00554556725774743));
#26058=CARTESIAN_POINT('Ctrl Pts',(-0.191385429512063,0.0150388003056731,
0.00585256287769953));
#26059=CARTESIAN_POINT('Ctrl Pts',(-0.189924359857282,0.0144159207087289,
0.00669446943947488));
#26060=CARTESIAN_POINT('Ctrl Pts',(-0.188118588226452,0.0129535683023105,
0.0079971734865383));
#26061=CARTESIAN_POINT('Ctrl Pts',(-0.186728499480259,0.0109160101219197,
0.00909799313116123));
#26062=CARTESIAN_POINT('Ctrl Pts',(-0.186240928505495,0.00922649890739429,
0.00949868329865868));
#26063=CARTESIAN_POINT('Ctrl Pts',(-0.186146181814525,0.00833801480660534,
0.00957679076147885));
#26064=CARTESIAN_POINT('',(-0.237657867810474,0.00839975141101414,0.0107287568273012));
#26065=CARTESIAN_POINT('Ctrl Pts',(-0.186146188570675,0.00833798789827216,
0.00957649060684295));
#26066=CARTESIAN_POINT('Ctrl Pts',(-0.203316735846858,0.0083585159298715,
0.0099611404338935));
#26067=CARTESIAN_POINT('Ctrl Pts',(-0.220487282901184,0.00837917464529529,
0.0103457920140646));
#26068=CARTESIAN_POINT('Ctrl Pts',(-0.237657829826327,0.00839993762480588,
0.010730442320928));
#26069=CARTESIAN_POINT('',(-0.230843542079246,0.0161181318983597,0.00261043863931786));
#26070=CARTESIAN_POINT('Ctrl Pts',(-0.237657867810474,0.00839975141101414,
0.0107287568273012));
#26071=CARTESIAN_POINT('Ctrl Pts',(-0.237628040172413,0.00871804736541609,
0.0106932259604992));
#26072=CARTESIAN_POINT('Ctrl Pts',(-0.237583075320134,0.00903375586220757,
0.0106396630368088));
#26073=CARTESIAN_POINT('Ctrl Pts',(-0.237524354422287,0.00934381631424547,
0.0105697131231371));
#26074=CARTESIAN_POINT('Ctrl Pts',(-0.237409875404356,0.0099482930397302,
0.0104333426363938));
#26075=CARTESIAN_POINT('Ctrl Pts',(-0.237243104297146,0.0105312772939824,
0.0102346798484156));
#26076=CARTESIAN_POINT('Ctrl Pts',(-0.237034426717481,0.0110700480166096,
0.00998606499931368));
#26077=CARTESIAN_POINT('Ctrl Pts',(-0.236825749137817,0.0116088187392369,
0.00973745015021171));
#26078=CARTESIAN_POINT('Ctrl Pts',(-0.236575218375409,0.0121034354127291,
0.00943895128259336));
#26079=CARTESIAN_POINT('Ctrl Pts',(-0.236294502051235,0.0125537967820148,
0.00910454953732754));
#26080=CARTESIAN_POINT('Ctrl Pts',(-0.236015363399207,0.0130016270459575,
0.00877202718514883));
#26081=CARTESIAN_POINT('Ctrl Pts',(-0.235706378926574,0.013405701518213,
0.00840399539865004));
#26082=CARTESIAN_POINT('Ctrl Pts',(-0.235379076902145,0.0137658122240604,
0.00801408434478435));
#26083=CARTESIAN_POINT('Ctrl Pts',(-0.235377227013985,0.0137678475445937,
0.00801188059476749));
#26084=CARTESIAN_POINT('Ctrl Pts',(-0.235375376540491,0.0137698814606867,
0.00800967614545206));
#26085=CARTESIAN_POINT('Ctrl Pts',(-0.235373525482602,0.0137719139727705,
0.0080074709979345));
#26086=CARTESIAN_POINT('Ctrl Pts',(-0.234714805396164,0.0144952066067006,
0.00722274407358542));
#26087=CARTESIAN_POINT('Ctrl Pts',(-0.233982176786342,0.0150406056960837,
0.00634992635599267));
#26088=CARTESIAN_POINT('Ctrl Pts',(-0.233216594643784,0.0154272463887169,
0.00543780883209741));
#26089=CARTESIAN_POINT('Ctrl Pts',(-0.232451013528585,0.0158138865625047,
0.00452569253220128));
#26090=CARTESIAN_POINT('Ctrl Pts',(-0.231652435338367,0.0160415300380187,
0.00357419085672357));
#26091=CARTESIAN_POINT('Ctrl Pts',(-0.230843549352499,0.0161191166093656,
0.0026105069458129));
#26092=CARTESIAN_POINT('Origin',(-0.233966934007412,0.0158592789729621,
3.09238363249698E-10));
#26093=CARTESIAN_POINT('Ctrl Pts',(-0.227150244243996,0.0165409512347104,
-9.63953309535137E-15));
#26094=CARTESIAN_POINT('Ctrl Pts',(-0.237845216608682,0.0163742849350107,
-4.07145020822619E-16));
#26095=CARTESIAN_POINT('Ctrl Pts',(-0.227150244243996,0.01654095123471,
-0.000381994959333103));
#26096=CARTESIAN_POINT('Ctrl Pts',(-0.237845216608682,0.0163742849350106,
-0.000371791760088174));
#26097=CARTESIAN_POINT('Ctrl Pts',(-0.227150244243997,0.0165287121322335,
-0.00114598487798004));
#26098=CARTESIAN_POINT('Ctrl Pts',(-0.237845216608682,0.0163722325524407,
-0.00111537528026388));
#26099=CARTESIAN_POINT('Ctrl Pts',(-0.227150244243996,0.0164948323843552,
-0.00192393728847136));
#26100=CARTESIAN_POINT('Ctrl Pts',(-0.237845216608682,0.0163665512368254,
-0.00188927901278524));
#26101=CARTESIAN_POINT('Ctrl Pts',(-0.227150244243996,0.0164156764744566,
-0.00344935006783133));
#26102=CARTESIAN_POINT('Ctrl Pts',(-0.237845216608682,0.0163532775339462,
-0.0034371522067016));
#26103=CARTESIAN_POINT('Ctrl Pts',(-0.227150244243997,0.0158708078188047,
-0.00568348814190198));
#26104=CARTESIAN_POINT('Ctrl Pts',(-0.237845216608683,0.0158878089324482,
-0.00572426400319885));
#26105=CARTESIAN_POINT('Ctrl Pts',(-0.227150244243996,0.0138592003117079,
-0.00851222286772063));
#26106=CARTESIAN_POINT('Ctrl Pts',(-0.237845216608682,0.0139254525795067,
-0.00865325189315152));
#26107=CARTESIAN_POINT('Ctrl Pts',(-0.227150244243997,0.0109293641084061,
-0.0103996324725637));
#26108=CARTESIAN_POINT('Ctrl Pts',(-0.237845216608683,0.0109812780384655,
-0.0106210180177305));
#26109=CARTESIAN_POINT('Ctrl Pts',(-0.227150244243996,0.0074999999998714,
-0.0110623240930123));
#26110=CARTESIAN_POINT('Ctrl Pts',(-0.237845216608682,0.00749999999987136,
-0.01131420416039));
#26111=CARTESIAN_POINT('Ctrl Pts',(-0.227150244243997,0.00407063589135525,
-0.0103996324724683));
#26112=CARTESIAN_POINT('Ctrl Pts',(-0.237845216608683,0.00401872196129691,
-0.0106210180176321));
#26113=CARTESIAN_POINT('Ctrl Pts',(-0.227150244243996,0.00114079968810594,
-0.00851222286754358));
#26114=CARTESIAN_POINT('Ctrl Pts',(-0.237845216608682,0.00107454742031117,
-0.00865325189296982));
#26115=CARTESIAN_POINT('Ctrl Pts',(-0.227150244243997,-0.000870807818911773,
-0.00568348814166902));
#26116=CARTESIAN_POINT('Ctrl Pts',(-0.237845216608682,-0.00088780893254747,
-0.00572426400296157));
#26117=CARTESIAN_POINT('Ctrl Pts',(-0.227150244243996,-0.00141567647450146,
-0.00344935006758328));
#26118=CARTESIAN_POINT('Ctrl Pts',(-0.237845216608682,-0.00135327753398082,
-0.00343715220645101));
#26119=CARTESIAN_POINT('Ctrl Pts',(-0.227150244243996,-0.00149483238436559,
-0.00192393728824214));
#26120=CARTESIAN_POINT('Ctrl Pts',(-0.237845216608682,-0.00136655123682709,
-0.00188927901255543));
#26121=CARTESIAN_POINT('Ctrl Pts',(-0.227150244243996,-0.0015287121322383,
-0.00114598487779204));
#26122=CARTESIAN_POINT('Ctrl Pts',(-0.237845216608682,-0.00137223255244152,
-0.0011153752800763));
#26123=CARTESIAN_POINT('Ctrl Pts',(-0.227150244243997,-0.00154707078594764,
1.16062262795529E-13));
#26124=CARTESIAN_POINT('Ctrl Pts',(-0.237845216608682,-0.00137531112629545,
1.24505090562086E-13));
#26125=CARTESIAN_POINT('Ctrl Pts',(-0.227150244243996,-0.00152871213223388,
0.00114598487802365));
#26126=CARTESIAN_POINT('Ctrl Pts',(-0.237845216608682,-0.00137223255244077,
0.00111537528032471));
#26127=CARTESIAN_POINT('Ctrl Pts',(-0.227150244243996,-0.0014948323843583,
0.00192393728847254));
#26128=CARTESIAN_POINT('Ctrl Pts',(-0.237845216608682,-0.00136655123682587,
0.00188927901280252));
#26129=CARTESIAN_POINT('Ctrl Pts',(-0.227150244243996,-0.00141567647446389,
0.00344935006836688));
#26130=CARTESIAN_POINT('Ctrl Pts',(-0.237845216608682,-0.00135327753394768,
0.00343715220737864));
#26131=CARTESIAN_POINT('Ctrl Pts',(-0.227150244243997,-0.000870821762961343,
0.00568349039573915));
#26132=CARTESIAN_POINT('Ctrl Pts',(-0.237845216608682,-0.000887826039510656,
0.00572426676828764));
#26133=CARTESIAN_POINT('Ctrl Pts',(-0.227150244243997,0.00114085439618864,
0.00851222287679413));
#26134=CARTESIAN_POINT('Ctrl Pts',(-0.237845216608682,0.0010746145376654,
0.00865325190429854));
#26135=CARTESIAN_POINT('Ctrl Pts',(-0.227150244243996,0.00407062011024736,
0.0103996408584618));
#26136=CARTESIAN_POINT('Ctrl Pts',(-0.237845216608682,0.00401870260056976,
0.0106210283057897));
#26137=CARTESIAN_POINT('Ctrl Pts',(-0.227150244243997,0.00750000000000013,
0.0110623211795783));
#26138=CARTESIAN_POINT('Ctrl Pts',(-0.237845216608683,0.00749999999999948,
0.0113142005861093));
#26139=CARTESIAN_POINT('Ctrl Pts',(-0.227150244243996,0.0109293798897529,
0.0103996408584618));
#26140=CARTESIAN_POINT('Ctrl Pts',(-0.237845216608681,0.0109812973994292,
0.0106210283057901));
#26141=CARTESIAN_POINT('Ctrl Pts',(-0.227150244243997,0.0138591456038116,
0.00851222287679417));
#26142=CARTESIAN_POINT('Ctrl Pts',(-0.237845216608683,0.0139253854623337,
0.00865325190429944));
#26143=CARTESIAN_POINT('Ctrl Pts',(-0.227150244243997,0.0158708217629616,
0.00568349039573924));
#26144=CARTESIAN_POINT('Ctrl Pts',(-0.237845216608682,0.0158878260395101,
0.00572426676828895));
#26145=CARTESIAN_POINT('Ctrl Pts',(-0.227150244243996,0.0164156764744642,
0.00344935006836702));
#26146=CARTESIAN_POINT('Ctrl Pts',(-0.237845216608682,0.0163532775339475,
0.00343715220738017));
#26147=CARTESIAN_POINT('Ctrl Pts',(-0.227150244243996,0.0164740029315869,
0.00232534147293065));
#26148=CARTESIAN_POINT('Ctrl Pts',(-0.237845216608682,0.0163630583331681,
0.0022965935348158));
#26149=CARTESIAN_POINT('Ctrl Pts',(-0.227150244243996,0.0164948323843597,
0.00192393728845175));
#26150=CARTESIAN_POINT('Ctrl Pts',(-0.237845216608682,0.0163665512368261,
0.0018892790127829));
#26151=CARTESIAN_POINT('Ctrl Pts',(-0.227150244243996,0.0165287121322363,
0.00114598487796074));
#26152=CARTESIAN_POINT('Ctrl Pts',(-0.237845216608682,0.0163722325524412,
0.00111537528026272));
#26153=CARTESIAN_POINT('Ctrl Pts',(-0.227150244243996,0.0165409512347109,
0.000381994959313824));
#26154=CARTESIAN_POINT('Ctrl Pts',(-0.237845216608682,0.0163742849350108,
0.00037179176008736));
#26155=CARTESIAN_POINT('Ctrl Pts',(-0.227150244243996,0.0165409512347104,
-9.63953309535137E-15));
#26156=CARTESIAN_POINT('Ctrl Pts',(-0.237845216608682,0.0163742849350107,
-4.07145020822619E-16));
#26157=CARTESIAN_POINT('',(-0.230613689225592,0.0164370167296803,0.00231666183293797));
#26158=CARTESIAN_POINT('',(-0.228219847986792,0.016461711610013,0.00232234304728458));
#26159=CARTESIAN_POINT('Ctrl Pts',(-0.230613698506742,0.0164380746908005,
0.00231603175567153));
#26160=CARTESIAN_POINT('Ctrl Pts',(-0.228219860721099,0.0164629072347989,
0.00232246635860196));
#26161=CARTESIAN_POINT('',(-0.230845404656383,0.01641869106371,0.00262492038517608));
#26162=CARTESIAN_POINT('Ctrl Pts',(-0.230845397055334,0.0164178730318222,
0.0026248611718336));
#26163=CARTESIAN_POINT('Ctrl Pts',(-0.230763233312891,0.0164246613929725,
0.00252596184206025));
#26164=CARTESIAN_POINT('Ctrl Pts',(-0.230685933491642,0.0164310479032495,
0.0024230472437672));
#26165=CARTESIAN_POINT('Ctrl Pts',(-0.230613689225592,0.0164370167296803,
0.00231666183293795));
#26166=CARTESIAN_POINT('',(-0.230845404654042,-0.00141869264250409,0.0026249204784827));
#26167=CARTESIAN_POINT('Ctrl Pts',(-0.230845406155635,0.0164188524145726,
0.00262493206457884));
#26168=CARTESIAN_POINT('Ctrl Pts',(-0.231100300338632,0.016394135408487,
0.00293573688999021));
#26169=CARTESIAN_POINT('Ctrl Pts',(-0.231330253084667,0.0163562988156621,
0.00321637191052311));
#26170=CARTESIAN_POINT('Ctrl Pts',(-0.231531680676482,0.016314511634419,
0.00346194554495639));
#26171=CARTESIAN_POINT('Ctrl Pts',(-0.231632395191451,0.0162936178946247,
0.0035847332388272));
#26172=CARTESIAN_POINT('Ctrl Pts',(-0.231725978785969,0.0162717928171178,
0.00369876105724253));
#26173=CARTESIAN_POINT('Ctrl Pts',(-0.231816013844249,0.0162489000359078,
0.00380848773826119));
#26174=CARTESIAN_POINT('Ctrl Pts',(-0.231861031373389,0.0162374536453028,
0.00386335107877052));
#26175=CARTESIAN_POINT('Ctrl Pts',(-0.231905161506138,0.016225692875953,
0.00391713038034571));
#26176=CARTESIAN_POINT('Ctrl Pts',(-0.231943478722522,0.0162151366678332,
0.00396380508855938));
#26177=CARTESIAN_POINT('Ctrl Pts',(-0.231981795938907,0.0162045804597134,
0.00401047979677305));
#26178=CARTESIAN_POINT('Ctrl Pts',(-0.232014300953749,0.0161953870895132,
0.00405008402747138));
#26179=CARTESIAN_POINT('Ctrl Pts',(-0.232061142463723,0.0161815297542121,
0.00410721922519355));
#26180=CARTESIAN_POINT('Ctrl Pts',(-0.232107983973697,0.0161676724189111,
0.00416435442291572));
#26181=CARTESIAN_POINT('Ctrl Pts',(-0.232169160847613,0.0161488560231783,
0.00423895076719931));
#26182=CARTESIAN_POINT('Ctrl Pts',(-0.232225616581178,0.0161305642422028,
0.00430777306797529));
#26183=CARTESIAN_POINT('Ctrl Pts',(-0.232282072314744,0.0161122724612272,
0.00437659536875126));
#26184=CARTESIAN_POINT('Ctrl Pts',(-0.232333807470107,0.0160947133906112,
0.00443970018976271));
#26185=CARTESIAN_POINT('Ctrl Pts',(-0.232385377331384,0.0160765467528926,
0.00450260334417301));
#26186=CARTESIAN_POINT('Ctrl Pts',(-0.232488517053936,0.0160402134774552,
0.00462840965299361));
#26187=CARTESIAN_POINT('Ctrl Pts',(-0.232590995510011,0.0160012622260062,
0.00475334511963562));
#26188=CARTESIAN_POINT('Ctrl Pts',(-0.232690758730041,0.0159606000393275,
0.00487499945630557));
#26189=CARTESIAN_POINT('Ctrl Pts',(-0.232790521950071,0.0159199378526488,
0.00499665379297553));
#26190=CARTESIAN_POINT('Ctrl Pts',(-0.232887569522866,0.0158775169648435,
0.00511502319888208));
#26191=CARTESIAN_POINT('Ctrl Pts',(-0.232977286659695,0.0158360935819725,
0.0052243323902255));
#26192=CARTESIAN_POINT('Ctrl Pts',(-0.233067003796523,0.0157946701991014,
0.00533364158156891));
#26193=CARTESIAN_POINT('Ctrl Pts',(-0.23314939055768,0.0157546441706645,
0.00543403165986536));
#26194=CARTESIAN_POINT('Ctrl Pts',(-0.233244961120346,0.0157052982799395,
0.00555069044803048));
#26195=CARTESIAN_POINT('Ctrl Pts',(-0.233263930412106,0.0156955038770163,
0.00557384542930724));
#26196=CARTESIAN_POINT('Ctrl Pts',(-0.233283419144619,0.0156853288434712,
0.00559763514898268));
#26197=CARTESIAN_POINT('Ctrl Pts',(-0.233303270872681,0.0156748394500476,
0.00562186377880468));
#26198=CARTESIAN_POINT('Ctrl Pts',(-0.233383435573525,0.0156324814707721,
0.0057197031636423));
#26199=CARTESIAN_POINT('Ctrl Pts',(-0.23346951958345,0.0155848560910614,
0.00582464387515683));
#26200=CARTESIAN_POINT('Ctrl Pts',(-0.233551221014356,0.0155374303604521,
0.00592420294833371));
#26201=CARTESIAN_POINT('Ctrl Pts',(-0.233653154724202,0.0154782602748176,
0.00604841650940856));
#26202=CARTESIAN_POINT('Ctrl Pts',(-0.233748264657028,0.0154197330280522,
0.006164431229071));
#26203=CARTESIAN_POINT('Ctrl Pts',(-0.233842820452025,0.0153585628948797,
0.00627980759476657));
#26204=CARTESIAN_POINT('Ctrl Pts',(-0.233937376247022,0.0152973927617072,
0.00639518396046214));
#26205=CARTESIAN_POINT('Ctrl Pts',(-0.234031378989655,0.0152333870670153,
0.00650981630376789));
#26206=CARTESIAN_POINT('Ctrl Pts',(-0.234119759433353,0.0151704480417673,
0.0066174646559021));
#26207=CARTESIAN_POINT('Ctrl Pts',(-0.23420813987705,0.0151075090165192,
0.00672511300803631));
#26208=CARTESIAN_POINT('Ctrl Pts',(-0.234290895921197,0.0150459592772678,
0.00682596426023255));
#26209=CARTESIAN_POINT('Ctrl Pts',(-0.23438203795834,0.0149747376617064,
0.00693722683716703));
#26210=CARTESIAN_POINT('Ctrl Pts',(-0.234473179995482,0.014903516046145,
0.00704848941410152));
#26211=CARTESIAN_POINT('Ctrl Pts',(-0.234572712055863,0.0148221387927767,
0.0071698520102151));
#26212=CARTESIAN_POINT('Ctrl Pts',(-0.234666614521964,0.0147414320966982,
0.00728423838151296));
#26213=CARTESIAN_POINT('Ctrl Pts',(-0.234760516988065,0.0146607254006198,
0.00739862475281083));
#26214=CARTESIAN_POINT('Ctrl Pts',(-0.234848786350016,0.0145810186683803,
0.00750627424136947));
#26215=CARTESIAN_POINT('Ctrl Pts',(-0.234936248176809,0.0144983824900823,
0.00761302947121143));
#26216=CARTESIAN_POINT('Ctrl Pts',(-0.235023710003601,0.0144157463117844,
0.00771978470105339));
#26217=CARTESIAN_POINT('Ctrl Pts',(-0.23511036646589,0.0143299974330337,
0.00782550470042646));
#26218=CARTESIAN_POINT('Ctrl Pts',(-0.235190938922874,0.014247020334218,
0.00792356544252254));
#26219=CARTESIAN_POINT('Ctrl Pts',(-0.235271511379857,0.0141640432354024,
0.00802162618461862));
#26220=CARTESIAN_POINT('Ctrl Pts',(-0.235345994424314,0.0140842359024048,
0.00811235964384396));
#26221=CARTESIAN_POINT('Ctrl Pts',(-0.235430686760159,0.0139887033941303,
0.00821589281443685));
#26222=CARTESIAN_POINT('Ctrl Pts',(-0.235495095996826,0.0139160501147822,
0.00829463066504644));
#26223=CARTESIAN_POINT('Ctrl Pts',(-0.235565415763708,0.0138340266016512,
0.00838051344444797));
#26224=CARTESIAN_POINT('Ctrl Pts',(-0.235634425112979,0.0137502746078903,
0.00846458329314199));
#26225=CARTESIAN_POINT('Ctrl Pts',(-0.235656156832651,0.0137239002851413,
0.00849105771152119));
#26226=CARTESIAN_POINT('Ctrl Pts',(-0.235677758600599,0.0136973642359917,
0.00851736083439707));
#26227=CARTESIAN_POINT('Ctrl Pts',(-0.235699004913631,0.0136709329854625,
0.00854323862301745));
#26228=CARTESIAN_POINT('Ctrl Pts',(-0.235787719161043,0.0135605689662904,
0.00865129165502526));
#26229=CARTESIAN_POINT('Ctrl Pts',(-0.235870228407553,0.0134521030844415,
0.00875205385374006));
#26230=CARTESIAN_POINT('Ctrl Pts',(-0.235950605571676,0.0133411714387136,
0.00885026140620821));
#26231=CARTESIAN_POINT('Ctrl Pts',(-0.236111359899922,0.0131193081472577,
0.0090466765111445));
#26232=CARTESIAN_POINT('Ctrl Pts',(-0.236263595884827,0.0128871731417065,
0.0092323612018346));
#26233=CARTESIAN_POINT('Ctrl Pts',(-0.236403654401485,0.0126515670091865,
0.0094029129604812));
#26234=CARTESIAN_POINT('Ctrl Pts',(-0.236543712918143,0.0124159608766665,
0.0095734647191278));
#26235=CARTESIAN_POINT('Ctrl Pts',(-0.236671587059248,0.0121771237877737,
0.00972922544746999));
#26236=CARTESIAN_POINT('Ctrl Pts',(-0.236789833249587,0.0119311450822871,
0.00987356375454342));
#26237=CARTESIAN_POINT('Ctrl Pts',(-0.236848956344757,0.0118081557295438,
0.00994573290808013));
#26238=CARTESIAN_POINT('Ctrl Pts',(-0.23690567511583,0.0116833001634472,
0.0100149174696784));
#26239=CARTESIAN_POINT('Ctrl Pts',(-0.236957846430498,0.0115626181380559,
0.0100782504702421));
#26240=CARTESIAN_POINT('Ctrl Pts',(-0.237010017745166,0.0114419361126645,
0.0101415834708057));
#26241=CARTESIAN_POINT('Ctrl Pts',(-0.237057632216303,0.011325666949853,
0.0101995095969159));
#26242=CARTESIAN_POINT('Ctrl Pts',(-0.237109142115983,0.0111901477257744,
0.0102626567192974));
#26243=CARTESIAN_POINT('Ctrl Pts',(-0.237144692626639,0.0110966166249623,
0.0103062388745939));
#26244=CARTESIAN_POINT('Ctrl Pts',(-0.237182106718332,0.0109937916041834,
0.0103520374018463));
#26245=CARTESIAN_POINT('Ctrl Pts',(-0.237218322025799,0.0108890866011028,
0.0103961046392556));
#26246=CARTESIAN_POINT('Ctrl Pts',(-0.237234579856412,0.0108420822727267,
0.0104158873701364));
#26247=CARTESIAN_POINT('Ctrl Pts',(-0.23725059609541,0.010794706184345,
0.0104353353011454));
#26248=CARTESIAN_POINT('Ctrl Pts',(-0.237266093686358,0.0107476642246503,
0.010454168061085));
#26249=CARTESIAN_POINT('Ctrl Pts',(-0.237316113104637,0.0105958334358221,
0.0105149519403283));
#26250=CARTESIAN_POINT('Ctrl Pts',(-0.237360717689318,0.0104475103219917,
0.0105694881860006));
#26251=CARTESIAN_POINT('Ctrl Pts',(-0.237402188197519,0.0102972373788654,
0.010620255747033));
#26252=CARTESIAN_POINT('Ctrl Pts',(-0.237485129213922,0.0099966914926128,
0.0107217908690978));
#26253=CARTESIAN_POINT('Ctrl Pts',(-0.237555547649754,0.00968817545869758,
0.0108076341360598));
#26254=CARTESIAN_POINT('Ctrl Pts',(-0.237611806042195,0.00937864054540575,
0.0108759601364871));
#26255=CARTESIAN_POINT('Ctrl Pts',(-0.237724322827076,0.00875957071882208,
0.0110126121373416));
#26256=CARTESIAN_POINT('Ctrl Pts',(-0.237780162569082,0.00813666054908404,
0.0110808280399472));
#26257=CARTESIAN_POINT('Ctrl Pts',(-0.237780757020967,0.00751171081608989,
0.0110816784755926));
#26258=CARTESIAN_POINT('Ctrl Pts',(-0.237780760734013,0.00750780727624916,
0.011081683787555));
#26259=CARTESIAN_POINT('Ctrl Pts',(-0.237780762292029,0.00750390367038639,
0.0110816864372711));
#26260=CARTESIAN_POINT('Ctrl Pts',(-0.237780761694531,0.00749999999999945,
0.0110816864237671));
#26261=CARTESIAN_POINT('Ctrl Pts',(-0.23778066663381,0.00687893303717793,
0.0110816842753144));
#26262=CARTESIAN_POINT('Ctrl Pts',(-0.237726010708986,0.00625608202678869,
0.0110147767774946));
#26263=CARTESIAN_POINT('Ctrl Pts',(-0.237614845441578,0.00563821530166374,
0.0108796632942073));
#26264=CARTESIAN_POINT('Ctrl Pts',(-0.237558913447348,0.00532734016133628,
0.0108116819296686));
#26265=CARTESIAN_POINT('Ctrl Pts',(-0.237488683165496,0.00501775189075729,
0.0107261184353061));
#26266=CARTESIAN_POINT('Ctrl Pts',(-0.237405879976365,0.00471612119147505,
0.0106247571095187));
#26267=CARTESIAN_POINT('Ctrl Pts',(-0.2373644783818,0.00456530584183393,
0.0105740764466251));
#26268=CARTESIAN_POINT('Ctrl Pts',(-0.237319930103575,0.00441643903893137,
0.0105196014633509));
#26269=CARTESIAN_POINT('Ctrl Pts',(-0.237269894824879,0.00426394159912891,
0.0104588043597344));
#26270=CARTESIAN_POINT('Ctrl Pts',(-0.237253190953929,0.00421303156882405,
0.0104385077410399));
#26271=CARTESIAN_POINT('Ctrl Pts',(-0.237235876931987,0.00416172022874334,
0.0104174873363778));
#26272=CARTESIAN_POINT('Ctrl Pts',(-0.237218307823531,0.00411091345951884,
0.0103961043563028));
#26273=CARTESIAN_POINT('Ctrl Pts',(-0.237183249894779,0.00400953210029451,
0.0103534361131266));
#26274=CARTESIAN_POINT('Ctrl Pts',(-0.237147176277473,0.00391018939539668,
0.0103092664206609));
#26275=CARTESIAN_POINT('Ctrl Pts',(-0.237112908060806,0.00381972380657039,
0.0102672494712808));
#26276=CARTESIAN_POINT('Ctrl Pts',(-0.237061466496008,0.00368392183313235,
0.0102041759345063));
#26277=CARTESIAN_POINT('Ctrl Pts',(-0.237014075859274,0.00356786256094538,
0.0101465240645061));
#26278=CARTESIAN_POINT('Ctrl Pts',(-0.236962091075866,0.00344725418310079,
0.0100834231132401));
#26279=CARTESIAN_POINT('Ctrl Pts',(-0.236910106292458,0.00332664580525621,
0.0100203221619742));
#26280=CARTESIAN_POINT('Ctrl Pts',(-0.236853536995318,0.003201733163161,
0.00995131596519577));
#26281=CARTESIAN_POINT('Ctrl Pts',(-0.236794570856648,0.0030787040364747,
0.00987933488154406));
#26282=CARTESIAN_POINT('Ctrl Pts',(-0.236676638579308,0.00283264578310208,
0.00973537271424062));
#26283=CARTESIAN_POINT('Ctrl Pts',(-0.236549108070154,0.00259379182280089,
0.0095800372046828));
#26284=CARTESIAN_POINT('Ctrl Pts',(-0.23640942071538,0.00235815034729726,
0.00940993731667735));
#26285=CARTESIAN_POINT('Ctrl Pts',(-0.236269733360606,0.00212250887179363,
0.0092398374286719));
#26286=CARTESIAN_POINT('Ctrl Pts',(-0.236117896002483,0.00189031920890611,
0.00905463410525447));
#26287=CARTESIAN_POINT('Ctrl Pts',(-0.235957457637001,0.00166827584739166,
0.00885861358605071));
#26288=CARTESIAN_POINT('Ctrl Pts',(-0.23587723845426,0.00155725416663443,
0.00876060332644883));
#26289=CARTESIAN_POINT('Ctrl Pts',(-0.235794866603536,0.00144867026152674,
0.00866001258255653));
#26290=CARTESIAN_POINT('Ctrl Pts',(-0.235706421246396,0.00133831736827609,
0.00855228205242222));
#26291=CARTESIAN_POINT('Ctrl Pts',(-0.235682754877842,0.00130878894160599,
0.00852345532241545));
#26292=CARTESIAN_POINT('Ctrl Pts',(-0.235658654177629,0.00127913904841267,
0.0084941084536834));
#26293=CARTESIAN_POINT('Ctrl Pts',(-0.235634421754154,0.00124972540958528,
0.00846458324989155));
#26294=CARTESIAN_POINT('Ctrl Pts',(-0.235568093374281,0.00116921513739988,
0.00838376760489224));
#26295=CARTESIAN_POINT('Ctrl Pts',(-0.235500778107123,0.00109055246370788,
0.00830154828174661));
#26296=CARTESIAN_POINT('Ctrl Pts',(-0.235438681621512,0.00102030581655116,
0.00822564249980966));
#26297=CARTESIAN_POINT('Ctrl Pts',(-0.235353898793518,0.000924395245373119,
0.00812200528442701));
#26298=CARTESIAN_POINT('Ctrl Pts',(-0.235278834910607,0.000843726368531342,
0.00803055897729168));
#26299=CARTESIAN_POINT('Ctrl Pts',(-0.235197751777394,0.000760017919507905,
0.00793187284909972));
#26300=CARTESIAN_POINT('Ctrl Pts',(-0.235116668644181,0.000676309470484467,
0.00783318672090776));
#26301=CARTESIAN_POINT('Ctrl Pts',(-0.235029571572779,0.000589949806240253,
0.00772693550362108));
#26302=CARTESIAN_POINT('Ctrl Pts',(-0.234941674231112,0.000506744595351982,
0.00761964685648566));
#26303=CARTESIAN_POINT('Ctrl Pts',(-0.234853776889444,0.000423539384463711,
0.00751235820935023));
#26304=CARTESIAN_POINT('Ctrl Pts',(-0.234765077020754,0.000343301382149936,
0.00740417759734143));
#26305=CARTESIAN_POINT('Ctrl Pts',(-0.234670448982667,0.000261869893349022,
0.00728891518395673));
#26306=CARTESIAN_POINT('Ctrl Pts',(-0.234575820944579,0.000180438404548108,
0.00717365277057203));
#26307=CARTESIAN_POINT('Ctrl Pts',(-0.23447526857943,9.81717754813013E-5,
0.00705104731107811));
#26308=CARTESIAN_POINT('Ctrl Pts',(-0.234384076032058,2.68535732625788E-5,
0.00693971183174857));
#26309=CARTESIAN_POINT('Ctrl Pts',(-0.234292883484686,-4.44646289561437E-5,
0.00682837635241903));
#26310=CARTESIAN_POINT('Ctrl Pts',(-0.234211046367837,-0.000105360993591713,
0.00672864972887943));
#26311=CARTESIAN_POINT('Ctrl Pts',(-0.23412337118657,-0.00016787228663261,
0.00662186731835593));
#26312=CARTESIAN_POINT('Ctrl Pts',(-0.234035696005303,-0.000230383579673508,
0.00651508490783243));
#26313=CARTESIAN_POINT('Ctrl Pts',(-0.233942184999647,-0.000294164288529817,
0.00640104689092552));
#26314=CARTESIAN_POINT('Ctrl Pts',(-0.233848164561004,-0.000355105177677982,
0.00628632317533926));
#26315=CARTESIAN_POINT('Ctrl Pts',(-0.233754144122361,-0.000416046066826147,
0.00617159945975299));
#26316=CARTESIAN_POINT('Ctrl Pts',(-0.233659613180542,-0.000474341316365998,
0.00605629571904232));
#26317=CARTESIAN_POINT('Ctrl Pts',(-0.233558456155359,-0.000533221594720501,
0.00593302620228869));
#26318=CARTESIAN_POINT('Ctrl Pts',(-0.233474310049849,-0.000582200359229365,
0.00583048611924345));
#26319=CARTESIAN_POINT('Ctrl Pts',(-0.233385580249099,-0.000631352225649045,
0.00572231156613564));
#26320=CARTESIAN_POINT('Ctrl Pts',(-0.233303279983003,-0.000674839454613146,
0.00562186381649031));
#26321=CARTESIAN_POINT('Ctrl Pts',(-0.233286642216975,-0.00068363080335406,
0.0056015573674843));
#26322=CARTESIAN_POINT('Ctrl Pts',(-0.233270267215688,-0.000692197111540543,
0.00558156925020403));
#26323=CARTESIAN_POINT('Ctrl Pts',(-0.233254245969635,-0.000700499830582056,
0.00556201347580956));
#26324=CARTESIAN_POINT('Ctrl Pts',(-0.233158974131218,-0.000749872726069023,
0.00544572323396024));
#26325=CARTESIAN_POINT('Ctrl Pts',(-0.233076210545331,-0.000790248603855624,
0.0053448711035504));
#26326=CARTESIAN_POINT('Ctrl Pts',(-0.232986293433231,-0.00083192370727539,
0.00523531504586229));
#26327=CARTESIAN_POINT('Ctrl Pts',(-0.232896376321131,-0.000873598810695155,
0.00512575898817417));
#26328=CARTESIAN_POINT('Ctrl Pts',(-0.232799305640179,-0.000916189568014474,
0.00500736315149536));
#26329=CARTESIAN_POINT('Ctrl Pts',(-0.232699475480134,-0.000957040429939678,
0.00488562808656381));
#26330=CARTESIAN_POINT('Ctrl Pts',(-0.23259964532009,-0.000997891291864883,
0.00476389302163227));
#26331=CARTESIAN_POINT('Ctrl Pts',(-0.232497056076894,-0.0010370458356378,
0.00463882151690649));
#26332=CARTESIAN_POINT('Ctrl Pts',(-0.232393792110345,-0.00107357729545367,
0.00451286349182803));
#26333=CARTESIAN_POINT('Ctrl Pts',(-0.232342160127071,-0.0010918430253616,
0.0044498844792888));
#26334=CARTESIAN_POINT('Ctrl Pts',(-0.232290359484728,-0.00110949976706081,
0.00438669985428264));
#26335=CARTESIAN_POINT('Ctrl Pts',(-0.23223387589419,-0.00112788179208304,
0.00431784339824848));
#26336=CARTESIAN_POINT('Ctrl Pts',(-0.232177392303652,-0.00114626381710528,
0.00424898694221432));
#26337=CARTESIAN_POINT('Ctrl Pts',(-0.232116225215548,-0.00116516478536523,
0.00417440231650458));
#26338=CARTESIAN_POINT('Ctrl Pts',(-0.232069243323862,-0.00117912866891544,
0.00411709598246582));
#26339=CARTESIAN_POINT('Ctrl Pts',(-0.232022261432176,-0.00119309255246565,
0.00405978964842705));
#26340=CARTESIAN_POINT('Ctrl Pts',(-0.231989465850055,-0.00120241270487414,
0.00401983136596938));
#26341=CARTESIAN_POINT('Ctrl Pts',(-0.231950878638839,-0.00121309140983481,
0.00397282798321303));
#26342=CARTESIAN_POINT('Ctrl Pts',(-0.231912291427624,-0.00122377011479549,
0.00392582460045668));
#26343=CARTESIAN_POINT('Ctrl Pts',(-0.231867911879468,-0.00123564945038949,
0.00387174191318196));
#26344=CARTESIAN_POINT('Ctrl Pts',(-0.231822623769973,-0.00124721447752194,
0.00381654936798492));
#26345=CARTESIAN_POINT('Ctrl Pts',(-0.231732047550984,-0.00127034453178683,
0.00370616427759082));
#26346=CARTESIAN_POINT('Ctrl Pts',(-0.231637838129472,-0.00129240691549724,
0.00359137488292652));
#26347=CARTESIAN_POINT('Ctrl Pts',(-0.231536443480711,-0.00131352075345898,
0.00346775798194196));
#26348=CARTESIAN_POINT('Ctrl Pts',(-0.231333655616239,-0.00135574813097255,
0.00322052592709761));
#26349=CARTESIAN_POINT('Ctrl Pts',(-0.231102125386862,-0.00139395843488747,
0.00293796225972129));
#26350=CARTESIAN_POINT('Ctrl Pts',(-0.23084540613858,-0.0014188524162263,
0.00262493204378136));
#26351=CARTESIAN_POINT('',(-0.230845404651119,-0.00141869028668481,-0.00262492044785718));
#26352=CARTESIAN_POINT('Ctrl Pts',(-0.23084539705679,-0.00141787297644972,
-0.00262486128582299));
#26353=CARTESIAN_POINT('Ctrl Pts',(-0.230239453773023,-0.00146793597280632,
-0.00189549595714672));
#26354=CARTESIAN_POINT('Ctrl Pts',(-0.229556645639841,-0.00152435019813871,
-2.99121385213125E-11));
#26355=CARTESIAN_POINT('Ctrl Pts',(-0.230239453775278,-0.00146793830190954,
0.00189549598038732));
#26356=CARTESIAN_POINT('Ctrl Pts',(-0.230845397068071,-0.00141787620064688,
0.00262486137994144));
#26357=CARTESIAN_POINT('',(-0.230845404648896,0.0164186918782877,-0.00262492054209142));
#26358=CARTESIAN_POINT('Ctrl Pts',(-0.230845406155915,-0.0014188522345682,
-0.00262493217065937));
#26359=CARTESIAN_POINT('Ctrl Pts',(-0.231100299441669,-0.00139413497480491,
-0.00293573599126679));
#26360=CARTESIAN_POINT('Ctrl Pts',(-0.231330251778893,-0.00135629782996439,
-0.00321637052807434));
#26361=CARTESIAN_POINT('Ctrl Pts',(-0.231531679491658,-0.0013145100902101,
-0.0034619443061207));
#26362=CARTESIAN_POINT('Ctrl Pts',(-0.231632394067082,-0.00129361607116236,
-0.00358473207177392));
#26363=CARTESIAN_POINT('Ctrl Pts',(-0.231725977854448,-0.00127179070475759,
-0.00369876011773195));
#26364=CARTESIAN_POINT('Ctrl Pts',(-0.231816013196795,-0.00124889763374325,
-0.00380848713108777));
#26365=CARTESIAN_POINT('Ctrl Pts',(-0.231861030867968,-0.00123745109823607,
-0.00386335063776568));
#26366=CARTESIAN_POINT('Ctrl Pts',(-0.231905161165557,-0.00122569018461765,
-0.00391713013177141));
#26367=CARTESIAN_POINT('Ctrl Pts',(-0.231943478626256,-0.00121513382583439,
-0.00396380513001859));
#26368=CARTESIAN_POINT('Ctrl Pts',(-0.231981796086954,-0.00120457746705113,
-0.00401048012826578));
#26369=CARTESIAN_POINT('Ctrl Pts',(-0.232014301425573,-0.00119538393551268,
-0.00405008474598364));
#26370=CARTESIAN_POINT('Ctrl Pts',(-0.232061143106978,-0.00118152646221356,
-0.00410722013721966));
#26371=CARTESIAN_POINT('Ctrl Pts',(-0.232107984788383,-0.00116766898891443,
-0.00416435552845569));
#26372=CARTESIAN_POINT('Ctrl Pts',(-0.232169161681404,-0.0011488524875137,
-0.00423895187437171));
#26373=CARTESIAN_POINT('Ctrl Pts',(-0.232225617477761,-0.00113056062213835,
-0.00430777422986251));
#26374=CARTESIAN_POINT('Ctrl Pts',(-0.232282073274118,-0.00111226875676299,
-0.00437659658535332));
#26375=CARTESIAN_POINT('Ctrl Pts',(-0.232333808535951,-0.00109470961568399,
-0.00443970151234894));
#26376=CARTESIAN_POINT('Ctrl Pts',(-0.232385378497271,-0.00107654293258796,
-0.00450260476284944));
#26377=CARTESIAN_POINT('Ctrl Pts',(-0.232488518419909,-0.0010402095663959,
-0.00462841126385043));
#26378=CARTESIAN_POINT('Ctrl Pts',(-0.232590997050356,-0.00100125833324369,
-0.00475334688627594));
#26379=CARTESIAN_POINT('Ctrl Pts',(-0.232690760482472,-0.000960596280089447,
-0.00487500141782347));
#26380=CARTESIAN_POINT('Ctrl Pts',(-0.232790523914588,-0.000919934226935205,
-0.004996655949371));
#26381=CARTESIAN_POINT('Ctrl Pts',(-0.232887571737198,-0.000877513589272111,
-0.00511502558860545));
#26382=CARTESIAN_POINT('Ctrl Pts',(-0.232977289062584,-0.000836090591733953,
-0.00522433494448881));
#26383=CARTESIAN_POINT('Ctrl Pts',(-0.23306700638797,-0.000794667594195795,
-0.00533364430037216));
#26384=CARTESIAN_POINT('Ctrl Pts',(-0.233149393276443,-0.000754642065908336,
-0.00543403446638583));
#26385=CARTESIAN_POINT('Ctrl Pts',(-0.233244964237605,-0.000705296829430848,
-0.00555069365387462));
#26386=CARTESIAN_POINT('Ctrl Pts',(-0.233263932311264,-0.000695503226134894,
-0.00557384713098106));
#26387=CARTESIAN_POINT('Ctrl Pts',(-0.233283419765313,-0.000685329050860441,
-0.0055976352729477));
#26388=CARTESIAN_POINT('Ctrl Pts',(-0.233303270183162,-0.000674840562095146,
-0.00562186228754064));
#26389=CARTESIAN_POINT('Ctrl Pts',(-0.233383436432652,-0.000632482622148265,
-0.00571970349728819));
#26390=CARTESIAN_POINT('Ctrl Pts',(-0.233469522483554,-0.000584857161359883,
-0.00582464663831474));
#26391=CARTESIAN_POINT('Ctrl Pts',(-0.233551225695154,-0.000537431472865814,
-0.0059242078377752));
#26392=CARTESIAN_POINT('Ctrl Pts',(-0.233653159900472,-0.000478262441763955,
-0.00604842194819661));
#26393=CARTESIAN_POINT('Ctrl Pts',(-0.233748270154742,-0.000419736430952795,
-0.00616443701620916));
#26394=CARTESIAN_POINT('Ctrl Pts',(-0.233842826257912,-0.000358567629232587,
-0.006279813729117));
#26395=CARTESIAN_POINT('Ctrl Pts',(-0.233937382361082,-0.000297398827512379,
-0.00639519044202484));
#26396=CARTESIAN_POINT('Ctrl Pts',(-0.23403138539862,-0.000233394558382435,
-0.00650982313433746));
#26397=CARTESIAN_POINT('Ctrl Pts',(-0.234119765925877,-0.000170457051937254,
-0.00661747158556569));
#26398=CARTESIAN_POINT('Ctrl Pts',(-0.234208146453135,-0.000107519545492074,
-0.00672512003679392));
#26399=CARTESIAN_POINT('Ctrl Pts',(-0.234290902369359,-4.59714339226739E-5,
-0.00682597114194729));
#26400=CARTESIAN_POINT('Ctrl Pts',(-0.234382044699051,2.52487478127625E-5,
-0.0069372341098404));
#26401=CARTESIAN_POINT('Ctrl Pts',(-0.234473187028743,9.64689295481989E-5,
-0.00704849707773351));
#26402=CARTESIAN_POINT('Ctrl Pts',(-0.234572719802503,0.000177844972312555,
-0.0071698605915413));
#26403=CARTESIAN_POINT('Ctrl Pts',(-0.234666622816077,0.00025855057469694,
-0.00728424768332998));
#26404=CARTESIAN_POINT('Ctrl Pts',(-0.234760525829651,0.000339256177081325,
-0.00739863477511866));
#26405=CARTESIAN_POINT('Ctrl Pts',(-0.234848795572813,0.000418961911282749,
-0.00750628479796341));
#26406=CARTESIAN_POINT('Ctrl Pts',(-0.234936257673823,0.000501597197614576,
-0.00761304043838177));
#26407=CARTESIAN_POINT('Ctrl Pts',(-0.235023719774834,0.000584232483946402,
-0.00771979607880013));
#26408=CARTESIAN_POINT('Ctrl Pts',(-0.235110376404512,0.000669980582370447,
-0.00782551636256507));
#26409=CARTESIAN_POINT('Ctrl Pts',(-0.235190949272289,0.000752957489623783,
-0.00792357768997112));
#26410=CARTESIAN_POINT('Ctrl Pts',(-0.235271522140065,0.000835934396877121,
-0.00802163901737717));
#26411=CARTESIAN_POINT('Ctrl Pts',(-0.235346005838469,0.00091574212505546,
-0.00811237336127969));
#26412=CARTESIAN_POINT('Ctrl Pts',(-0.235430697611473,0.00101127399908969,
-0.00821590594222279));
#26413=CARTESIAN_POINT('Ctrl Pts',(-0.235495103302302,0.00108392327923873,
-0.00829463953301149));
#26414=CARTESIAN_POINT('Ctrl Pts',(-0.23556541824769,0.00116594127053609,
-0.00838051651305141));
#26415=CARTESIAN_POINT('Ctrl Pts',(-0.235634423268975,0.00124968821256174,
-0.00846458116969803));
#26416=CARTESIAN_POINT('Ctrl Pts',(-0.2356561580181,0.0012760662752152,
-0.00849105930401949));
#26417=CARTESIAN_POINT('Ctrl Pts',(-0.23567776281192,0.00130260617834922,
-0.00851736613094175));
#26418=CARTESIAN_POINT('Ctrl Pts',(-0.235699012065757,0.00132904129744443,
-0.00854324751893055));
#26419=CARTESIAN_POINT('Ctrl Pts',(-0.235787724956046,0.00143940450539861,
-0.00865129897103351));
#26420=CARTESIAN_POINT('Ctrl Pts',(-0.235870233267096,0.00154787042356857,
-0.00875206008310034));
#26421=CARTESIAN_POINT('Ctrl Pts',(-0.235950609516249,0.00165880240566226,
-0.00885026655961241));
#26422=CARTESIAN_POINT('Ctrl Pts',(-0.236111362014556,0.00188066636984964,
-0.00904667951263656));
#26423=CARTESIAN_POINT('Ctrl Pts',(-0.236263596251478,0.00211280322822169,
-0.00923236210459433));
#26424=CARTESIAN_POINT('Ctrl Pts',(-0.236403653405857,0.00234841200251143,
-0.00940291221444271));
#26425=CARTESIAN_POINT('Ctrl Pts',(-0.236543710560236,0.00258402077680117,
-0.00957346232429108));
#26426=CARTESIAN_POINT('Ctrl Pts',(-0.236671583724811,0.00282286130642932,
-0.00972922184899156));
#26427=CARTESIAN_POINT('Ctrl Pts',(-0.236789829280297,0.00306884369932654,
-0.00987355935155708));
#26428=CARTESIAN_POINT('Ctrl Pts',(-0.236848952058039,0.00319183489577516,
-0.00994572810283985));
#26429=CARTESIAN_POINT('Ctrl Pts',(-0.236905670597119,0.00331669236566743,
-0.0100149123613222));
#26430=CARTESIAN_POINT('Ctrl Pts',(-0.236957841711828,0.00343737605699863,
-0.0100782450944094));
#26431=CARTESIAN_POINT('Ctrl Pts',(-0.237010012826538,0.00355805974832983,
-0.0101415778274966));
#26432=CARTESIAN_POINT('Ctrl Pts',(-0.237057627129816,0.00367433034474948,
-0.0101995037203407));
#26433=CARTESIAN_POINT('Ctrl Pts',(-0.237109137139568,0.00380985165238374,
-0.0102626509316129));
#26434=CARTESIAN_POINT('Ctrl Pts',(-0.237144687449298,0.0039033834626968,
-0.0103062328088071));
#26435=CARTESIAN_POINT('Ctrl Pts',(-0.237182101443326,0.00400620936376822,
-0.010352031182122));
#26436=CARTESIAN_POINT('Ctrl Pts',(-0.23721831670714,0.00411091512385162,
-0.010396098336241));
#26437=CARTESIAN_POINT('Ctrl Pts',(-0.23723457492686,0.00415792097370976,
-0.0104158815270468));
#26438=CARTESIAN_POINT('Ctrl Pts',(-0.237250591553704,0.00420529857814582,
-0.0104353299151331));
#26439=CARTESIAN_POINT('Ctrl Pts',(-0.237266089505886,0.00425234197839895,
-0.0104541631023438));
#26440=CARTESIAN_POINT('Ctrl Pts',(-0.237316109222227,0.00440417478242368,
-0.0105149473060269));
#26441=CARTESIAN_POINT('Ctrl Pts',(-0.237360714015525,0.00455249920513233,
-0.0105694837750095));
#26442=CARTESIAN_POINT('Ctrl Pts',(-0.237402184731641,0.00470277313262922,
-0.0106202515747131));
#26443=CARTESIAN_POINT('Ctrl Pts',(-0.237485126163871,0.005003320987623,
-0.0107217871741204));
#26444=CARTESIAN_POINT('Ctrl Pts',(-0.237555545013006,0.00531183770396397,
-0.0108076309622602));
#26445=CARTESIAN_POINT('Ctrl Pts',(-0.237611803761463,0.00562137180228855,
-0.0108759573592423));
#26446=CARTESIAN_POINT('Ctrl Pts',(-0.237724321258377,0.0062404399989377,
-0.0110126101532065));
#26447=CARTESIAN_POINT('Ctrl Pts',(-0.23778016147638,0.00686334246713551,
-0.0110808266634648));
#26448=CARTESIAN_POINT('Ctrl Pts',(-0.237780756134355,0.00748828520611799,
-0.0110816774046328));
#26449=CARTESIAN_POINT('Ctrl Pts',(-0.23778075984999,0.00749219007177514,
-0.0110816827203678));
#26450=CARTESIAN_POINT('Ctrl Pts',(-0.237780761409074,0.00749609500352675,
-0.0110816853719659));
#26451=CARTESIAN_POINT('Ctrl Pts',(-0.237780760811121,0.00749999999987464,
-0.0110816853584517));
#26452=CARTESIAN_POINT('Ctrl Pts',(-0.237780665711467,0.0081210586585245,
-0.0110816832091296));
#26453=CARTESIAN_POINT('Ctrl Pts',(-0.237726009720084,0.00874390205312341,
-0.0110147755481997));
#26454=CARTESIAN_POINT('Ctrl Pts',(-0.237614844192197,0.0093617667327187,
-0.0108796617768425));
#26455=CARTESIAN_POINT('Ctrl Pts',(-0.237558911943567,0.00967264152938713,
-0.0108116801174518));
#26456=CARTESIAN_POINT('Ctrl Pts',(-0.237488681296103,0.00998223085392503,
-0.0107261161776055));
#26457=CARTESIAN_POINT('Ctrl Pts',(-0.237405877712267,0.0102838639138477,
-0.0106247544023578));
#26458=CARTESIAN_POINT('Ctrl Pts',(-0.237364475920348,0.0104346804438091,
-0.0105740735147339));
#26459=CARTESIAN_POINT('Ctrl Pts',(-0.237319927437426,0.0105835487558483,
-0.0105195983099089));
#26460=CARTESIAN_POINT('Ctrl Pts',(-0.237269891845089,0.0107360484391602,
-0.0104588008630779));
#26461=CARTESIAN_POINT('Ctrl Pts',(-0.237253187233269,0.0107869611573549,
-0.0104385033568127));
#26462=CARTESIAN_POINT('Ctrl Pts',(-0.237235872411813,0.0108382752930308,
-0.0104174819969918));
#26463=CARTESIAN_POINT('Ctrl Pts',(-0.237218302501169,0.0108890848152787,
-0.0103960980533122));
#26464=CARTESIAN_POINT('Ctrl Pts',(-0.237183244975997,0.0109904658718642,
-0.0103534303267071));
#26465=CARTESIAN_POINT('Ctrl Pts',(-0.237147171867749,0.0110898083390762,
-0.0103092612874042));
#26466=CARTESIAN_POINT('Ctrl Pts',(-0.237112904226435,0.0111802736864231,
-0.0102672450731564));
#26467=CARTESIAN_POINT('Ctrl Pts',(-0.237061462543517,0.0113160778893066,
-0.0102041714361071));
#26468=CARTESIAN_POINT('Ctrl Pts',(-0.237014072093481,0.0114321386325685,
-0.0101465198227962));
#26469=CARTESIAN_POINT('Ctrl Pts',(-0.236962087516987,0.0115527487461073,
-0.0100834191489188));
#26470=CARTESIAN_POINT('Ctrl Pts',(-0.236910102940493,0.0116733588596461,
-0.0100203184750413));
#26471=CARTESIAN_POINT('Ctrl Pts',(-0.236853533870469,0.0117982735066382,
-0.00995131257547577));
#26472=CARTESIAN_POINT('Ctrl Pts',(-0.236794568042232,0.0119213045748546,
-0.00987933188546306));
#26473=CARTESIAN_POINT('Ctrl Pts',(-0.236676636385759,0.0121673667112875,
-0.00973537050543764));
#26474=CARTESIAN_POINT('Ctrl Pts',(-0.236549106830628,0.012406224296211,
-0.00958003617413828));
#26475=CARTESIAN_POINT('Ctrl Pts',(-0.236409420796806,0.0126418686144187,
-0.00940993788674596));
#26476=CARTESIAN_POINT('Ctrl Pts',(-0.236269734762985,0.0128775129326265,
-0.00923983959935364));
#26477=CARTESIAN_POINT('Ctrl Pts',(-0.236117899092723,0.0131097046653902,
-0.0090546383024288));
#26478=CARTESIAN_POINT('Ctrl Pts',(-0.235957462490158,0.013331748912476,
-0.00885861985415937));
#26479=CARTESIAN_POINT('Ctrl Pts',(-0.235877244188876,0.0134427710360188,
-0.00876061063002465));
#26480=CARTESIAN_POINT('Ctrl Pts',(-0.235794873238375,0.0135513550829385,
-0.0086600209302118));
#26481=CARTESIAN_POINT('Ctrl Pts',(-0.235706429188876,0.0136617072842212,
-0.00855229192071309));
#26482=CARTESIAN_POINT('Ctrl Pts',(-0.235682759623755,0.0136912399506845,
-0.00852346127783545));
#26483=CARTESIAN_POINT('Ctrl Pts',(-0.235658655626003,0.013720894062547,
-0.00849411037167573));
#26484=CARTESIAN_POINT('Ctrl Pts',(-0.235634419909639,0.0137503117697787,
-0.008464581126618));
#26485=CARTESIAN_POINT('Ctrl Pts',(-0.235568096087339,0.0138308167054532,
-0.00838377095486792));
#26486=CARTESIAN_POINT('Ctrl Pts',(-0.235500785816309,0.0139094736614859,
-0.00830155764904172));
#26487=CARTESIAN_POINT('Ctrl Pts',(-0.235438693122288,0.0139797160557346,
-0.0082256564292159));
#26488=CARTESIAN_POINT('Ctrl Pts',(-0.235353910829442,0.0140756260711292,
-0.00812201976876574));
#26489=CARTESIAN_POINT('Ctrl Pts',(-0.235278846300897,0.0141562953693376,
-0.00803057258615523));
#26490=CARTESIAN_POINT('Ctrl Pts',(-0.23519776275404,0.0142400036595105,
-0.00793188586844095));
#26491=CARTESIAN_POINT('Ctrl Pts',(-0.235116679207183,0.0143237119496834,
-0.00783319915072666));
#26492=CARTESIAN_POINT('Ctrl Pts',(-0.23502958195438,0.0144100708725911,
-0.00772694763099746));
#26493=CARTESIAN_POINT('Ctrl Pts',(-0.23494168432416,0.0144932752247202,
-0.00761965855480392));
#26494=CARTESIAN_POINT('Ctrl Pts',(-0.23485378669394,0.0145764795768493,
-0.00751236947861039));
#26495=CARTESIAN_POINT('Ctrl Pts',(-0.234765086429372,0.0146567166088885,
-0.00740418831371886));
#26496=CARTESIAN_POINT('Ctrl Pts',(-0.23467045783265,0.0147381470204307,
-0.00728892516558668));
#26497=CARTESIAN_POINT('Ctrl Pts',(-0.234575829235928,0.0148195774319729,
-0.00717366201745451));
#26498=CARTESIAN_POINT('Ctrl Pts',(-0.234475276149762,0.0149018428550239,
-0.00705105563029274));
#26499=CARTESIAN_POINT('Ctrl Pts',(-0.234384083279509,0.014973159658642,
-0.0069397197229418));
#26500=CARTESIAN_POINT('Ctrl Pts',(-0.234292890409256,0.0150444764622601,
-0.00682838381559085));
#26501=CARTESIAN_POINT('Ctrl Pts',(-0.234211053367293,0.0151053712651558,
-0.00672865727439112));
#26502=CARTESIAN_POINT('Ctrl Pts',(-0.234123378056485,0.015167881091967,
-0.00662187470813778));
#26503=CARTESIAN_POINT('Ctrl Pts',(-0.234035702745677,0.0152303909187781,
-0.00651509214188445));
#26504=CARTESIAN_POINT('Ctrl Pts',(-0.233942191406194,0.015294170241559,
-0.006401053727849));
#26505=CARTESIAN_POINT('Ctrl Pts',(-0.233848170620294,0.0153551098348782,
-0.00628632961631849));
#26506=CARTESIAN_POINT('Ctrl Pts',(-0.233754149834394,0.0154160494281974,
-0.00617160550478799));
#26507=CARTESIAN_POINT('Ctrl Pts',(-0.233659618531884,0.0154743434736159,
-0.00605630136650607));
#26508=CARTESIAN_POINT('Ctrl Pts',(-0.233558460970936,0.0155332227250349,
-0.00593303125073153));
#26509=CARTESIAN_POINT('Ctrl Pts',(-0.23347431303379,0.0155822014420113,
-0.00583048898046401));
#26510=CARTESIAN_POINT('Ctrl Pts',(-0.233385581129215,0.0156313533891151,
-0.00572231192292485));
#26511=CARTESIAN_POINT('Ctrl Pts',(-0.233303279293739,0.0156748405665605,
-0.00562186232545755));
#26512=CARTESIAN_POINT('Ctrl Pts',(-0.233286642840047,0.0156836310438269,
-0.00560155749183029));
#26513=CARTESIAN_POINT('Ctrl Pts',(-0.233270269121464,0.0156921965193002,
-0.00558157095462027));
#26514=CARTESIAN_POINT('Ctrl Pts',(-0.233254249108412,0.0157004984529706,
-0.00556201669971721));
#26515=CARTESIAN_POINT('Ctrl Pts',(-0.23315897683986,0.0157498707007693,
-0.00544572601890478));
#26516=CARTESIAN_POINT('Ctrl Pts',(-0.233076213104704,0.0157902460744741,
-0.0053448737747612));
#26517=CARTESIAN_POINT('Ctrl Pts',(-0.232986295777531,0.0158319207926876,
-0.00523531752081867));
#26518=CARTESIAN_POINT('Ctrl Pts',(-0.232896378450358,0.0158735955109011,
-0.00512576126687615));
#26519=CARTESIAN_POINT('Ctrl Pts',(-0.232799307488513,0.0159161860208843,
-0.00500736515900809));
#26520=CARTESIAN_POINT('Ctrl Pts',(-0.232699477083465,0.0159570367517272,
-0.00488562985940448));
#26521=CARTESIAN_POINT('Ctrl Pts',(-0.232599646678417,0.0159978874825702,
-0.00476389455980087));
#26522=CARTESIAN_POINT('Ctrl Pts',(-0.232497057226093,0.0160370420103787,
-0.00463882285759716));
#26523=CARTESIAN_POINT('Ctrl Pts',(-0.232393793026214,0.0160735735624176,
-0.00451286460048705));
#26524=CARTESIAN_POINT('Ctrl Pts',(-0.232342160926274,0.0160918393384371,
-0.00444988547193199));
#26525=CARTESIAN_POINT('Ctrl Pts',(-0.232290360161217,0.0161094961511758,
-0.00438670072149367));
#26526=CARTESIAN_POINT('Ctrl Pts',(-0.232233876486394,0.0161278782621135,
-0.00431784418501812));
#26527=CARTESIAN_POINT('Ctrl Pts',(-0.232177392811571,0.0161462603730512,
-0.00424898764854258));
#26528=CARTESIAN_POINT('Ctrl Pts',(-0.232116225677619,0.0161651614491445,
-0.0041744029891438));
#26529=CARTESIAN_POINT('Ctrl Pts',(-0.232069243605778,0.0161791254692766,
-0.00411709645137768));
#26530=CARTESIAN_POINT('Ctrl Pts',(-0.232022261533936,0.0161930894894088,
-0.00405978991361156));
#26531=CARTESIAN_POINT('Ctrl Pts',(-0.231989465637333,0.0162024097984568,
-0.00401983125579712));
#26532=CARTESIAN_POINT('Ctrl Pts',(-0.231950878188651,0.0162130886498548,
-0.00397282759162673));
#26533=CARTESIAN_POINT('Ctrl Pts',(-0.231912290739969,0.0162237675012527,
-0.00392582392745635));
#26534=CARTESIAN_POINT('Ctrl Pts',(-0.231867911031374,0.0162356469772777,
-0.0038717410533253));
#26535=CARTESIAN_POINT('Ctrl Pts',(-0.231822622786801,0.0162472121451573,
-0.00381654835060898));
#26536=CARTESIAN_POINT('Ctrl Pts',(-0.231732046297657,0.0162703424809165,
-0.00370616294517634));
#26537=CARTESIAN_POINT('Ctrl Pts',(-0.231637836707432,0.0162924051440427,
-0.00359137335257152));
#26538=CARTESIAN_POINT('Ctrl Pts',(-0.231536442028934,0.016313519252232,
-0.00346775641743787));
#26539=CARTESIAN_POINT('Ctrl Pts',(-0.231333654104948,0.0163557471702052,
-0.00322052429424714));
#26540=CARTESIAN_POINT('Ctrl Pts',(-0.231102124372152,0.0163939580101801,
-0.00293796121806425));
#26541=CARTESIAN_POINT('Ctrl Pts',(-0.230845406138858,0.0164188522362164,
-0.00262493214986059));
#26542=CARTESIAN_POINT('',(-0.22989804971791,0.016496143666697,2.94875754215381E-7));
#26543=CARTESIAN_POINT('Ctrl Pts',(-0.22989804971791,0.016496143666697,
2.94875754180074E-7));
#26544=CARTESIAN_POINT('Ctrl Pts',(-0.229898014287119,0.0164961471566313,
-0.000947649746562464));
#26545=CARTESIAN_POINT('Ctrl Pts',(-0.230239453768766,0.0164679382629039,
-0.00189549608053806));
#26546=CARTESIAN_POINT('Ctrl Pts',(-0.230845397069526,0.0164178761451466,
-0.00262486149392285));
#26547=CARTESIAN_POINT('',(-0.22721365317106,0.0165399630933673,2.96878969865867E-7));
#26548=CARTESIAN_POINT('Ctrl Pts',(-0.229898080672427,0.0164981300169968,
2.94888303551387E-7));
#26549=CARTESIAN_POINT('Ctrl Pts',(-0.22721365317106,0.0165399630933672,
2.96878969865846E-7));
#26550=CARTESIAN_POINT('',(-0.234192388872042,0.0132952027870384,-0.00885670411852692));
#26551=CARTESIAN_POINT('Ctrl Pts',(-0.22721365317106,0.0165399630933673,
2.96878969865867E-7));
#26552=CARTESIAN_POINT('Ctrl Pts',(-0.227256908958651,0.0165392899807157,
-0.000116960173666361));
#26553=CARTESIAN_POINT('Ctrl Pts',(-0.227339124107497,0.0165367236578279,
-0.00033776437467711));
#26554=CARTESIAN_POINT('Ctrl Pts',(-0.227420071905186,0.0165329358482603,
-0.000553615272546889));
#26555=CARTESIAN_POINT('Ctrl Pts',(-0.227547101717011,0.0165249913814539,
-0.000878058900339982));
#26556=CARTESIAN_POINT('Ctrl Pts',(-0.22768815065478,0.0165141789319858,
-0.00121703749323916));
#26557=CARTESIAN_POINT('Ctrl Pts',(-0.227909366795336,0.0164944334295571,
-0.00169626548164348));
#26558=CARTESIAN_POINT('Ctrl Pts',(-0.228192601673969,0.0164694168554863,
-0.00221811204306224));
#26559=CARTESIAN_POINT('Ctrl Pts',(-0.228511119230705,0.0164359317145672,
-0.00274316378074596));
#26560=CARTESIAN_POINT('Ctrl Pts',(-0.228965207170631,0.0163483003756339,
-0.00341891990378775));
#26561=CARTESIAN_POINT('Ctrl Pts',(-0.229483054805567,0.0162096171069562,
-0.00406485955552118));
#26562=CARTESIAN_POINT('Ctrl Pts',(-0.229924175135309,0.0160759507361103,
-0.00452880943524848));
#26563=CARTESIAN_POINT('Ctrl Pts',(-0.230206707176665,0.0159866029159255,
-0.00480698677163651));
#26564=CARTESIAN_POINT('Ctrl Pts',(-0.230453694447789,0.015905557072168,
-0.00503765884127183));
#26565=CARTESIAN_POINT('Ctrl Pts',(-0.230627130821605,0.0158469989122931,
-0.00519355104939717));
#26566=CARTESIAN_POINT('Ctrl Pts',(-0.230845400469471,0.0157712591827807,
-0.00538515294067697));
#26567=CARTESIAN_POINT('Ctrl Pts',(-0.231034958715161,0.0157030686492419,
-0.00554683158695247));
#26568=CARTESIAN_POINT('Ctrl Pts',(-0.231182239317623,0.0156484588841278,
-0.00567000124877424));
#26569=CARTESIAN_POINT('Ctrl Pts',(-0.23126064767078,0.0156190133729797,
-0.00573503100777596));
#26570=CARTESIAN_POINT('Ctrl Pts',(-0.231343320990274,0.0155875483379559,
-0.00580304400235552));
#26571=CARTESIAN_POINT('Ctrl Pts',(-0.23134058848968,0.0155885738204978,
-0.00580073392463057));
#26572=CARTESIAN_POINT('Ctrl Pts',(-0.231385286047413,0.0155715171280465,
-0.00583726350714204));
#26573=CARTESIAN_POINT('Ctrl Pts',(-0.231459731254797,0.0155427769176357,
-0.00589778478912086));
#26574=CARTESIAN_POINT('Ctrl Pts',(-0.231588540995542,0.015492298062324,
-0.00600217942498043));
#26575=CARTESIAN_POINT('Ctrl Pts',(-0.231797916190688,0.0154069459195584,
-0.00617020369122395));
#26576=CARTESIAN_POINT('Ctrl Pts',(-0.231913738714637,0.015357925109019,
-0.00626257469253834));
#26577=CARTESIAN_POINT('Ctrl Pts',(-0.232036361551522,0.0153050086703646,
-0.00636048115638375));
#26578=CARTESIAN_POINT('Ctrl Pts',(-0.23214529893423,0.0152564410924344,
-0.00644752873286008));
#26579=CARTESIAN_POINT('Ctrl Pts',(-0.232222140947088,0.0152216138188694,
-0.00650905373166038));
#26580=CARTESIAN_POINT('Ctrl Pts',(-0.232361013019894,0.0151566147032964,
-0.00662098807208995));
#26581=CARTESIAN_POINT('Ctrl Pts',(-0.232511179434643,0.0150830306094505,
-0.00674346122390688));
#26582=CARTESIAN_POINT('Ctrl Pts',(-0.232661263135366,0.0150065039878354,
-0.00686741025236411));
#26583=CARTESIAN_POINT('Ctrl Pts',(-0.232900428682406,0.0148719157351182,
-0.00707399253491582));
#26584=CARTESIAN_POINT('Ctrl Pts',(-0.233081122635965,0.014759363715995,
-0.00723794642342912));
#26585=CARTESIAN_POINT('Ctrl Pts',(-0.233292763592228,0.014610902022631,
-0.0074435244792244));
#26586=CARTESIAN_POINT('Ctrl Pts',(-0.233522503099131,0.014424811635409,
-0.00768695917044636));
#26587=CARTESIAN_POINT('Ctrl Pts',(-0.233917538413758,0.0140205182082748,
-0.00817494331998796));
#26588=CARTESIAN_POINT('Ctrl Pts',(-0.234124037654978,0.0136070371323653,
-0.0085899342809721));
#26589=CARTESIAN_POINT('Ctrl Pts',(-0.234192388872042,0.0132952027870384,
-0.00885670411852691));
#26590=CARTESIAN_POINT('',(-0.230846395327677,0.00748914570500684,-0.0109249562858334));
#26591=CARTESIAN_POINT('Ctrl Pts',(-0.234192388872042,0.0132952027870384,
-0.00885670411852691));
#26592=CARTESIAN_POINT('Ctrl Pts',(-0.234260740089107,0.0129833684417114,
-0.00912347395608173));
#26593=CARTESIAN_POINT('Ctrl Pts',(-0.23425929449908,0.0124613464816401,
-0.00950879250776204));
#26594=CARTESIAN_POINT('Ctrl Pts',(-0.234077282934937,0.0118177007721254,
-0.0098888395261885));
#26595=CARTESIAN_POINT('Ctrl Pts',(-0.233826670793196,0.0112512047590739,
-0.0101709376840775));
#26596=CARTESIAN_POINT('Ctrl Pts',(-0.233610338176317,0.0108796222191891,
-0.0103246296716289));
#26597=CARTESIAN_POINT('Ctrl Pts',(-0.233394114013919,0.0105446557132715,
-0.010448281869205));
#26598=CARTESIAN_POINT('Ctrl Pts',(-0.233195095532645,0.01026174721601,
-0.0105405956701664));
#26599=CARTESIAN_POINT('Ctrl Pts',(-0.233051178813437,0.0100683811397472,
-0.0105975374989383));
#26600=CARTESIAN_POINT('Ctrl Pts',(-0.232868465840991,0.00983137860329251,
-0.0106613388492261));
#26601=CARTESIAN_POINT('Ctrl Pts',(-0.232679944650818,0.00959553063661281,
-0.0107177886081924));
#26602=CARTESIAN_POINT('Ctrl Pts',(-0.232447561116175,0.00931433765584752,
-0.0107753562428179));
#26603=CARTESIAN_POINT('Ctrl Pts',(-0.232290543708524,0.00912877171699688,
-0.0108078703367909));
#26604=CARTESIAN_POINT('Ctrl Pts',(-0.232095278994658,0.00890055703141569,
-0.0108433208555711));
#26605=CARTESIAN_POINT('Ctrl Pts',(-0.231920471854683,0.00869940054062883,
-0.0108683999653081));
#26606=CARTESIAN_POINT('Ctrl Pts',(-0.231782694028032,0.00854205404621492,
-0.0108851588016013));
#26607=CARTESIAN_POINT('Ctrl Pts',(-0.23164586132212,0.00838689206622596,
-0.0108987817482543));
#26608=CARTESIAN_POINT('Ctrl Pts',(-0.231618960279246,0.00835662431924158,
-0.0109009619444762));
#26609=CARTESIAN_POINT('Ctrl Pts',(-0.231521063942898,0.00824631142819562,
-0.0109091055405001));
#26610=CARTESIAN_POINT('Ctrl Pts',(-0.23132077524562,0.00802129497745352,
-0.010922259755925));
#26611=CARTESIAN_POINT('Ctrl Pts',(-0.23105771540997,0.00772600187303795,
-0.0109300225734977));
#26612=CARTESIAN_POINT('Ctrl Pts',(-0.230846362800463,0.00748918187660458,
-0.0109249555950961));
#26613=CARTESIAN_POINT('',(-0.227214261715267,-0.00153995361067246,2.08417333140297E-7));
#26614=CARTESIAN_POINT('Ctrl Pts',(-0.230846395327677,0.00748914570500684,
-0.0109249562858334));
#26615=CARTESIAN_POINT('Ctrl Pts',(-0.231037606532753,0.00727651095947488,
-0.0109290163499947));
#26616=CARTESIAN_POINT('Ctrl Pts',(-0.231284925260294,0.00700085820481965,
-0.0109227670625044));
#26617=CARTESIAN_POINT('Ctrl Pts',(-0.231493557178275,0.00676788077232978,
-0.0109097315243095));
#26618=CARTESIAN_POINT('Ctrl Pts',(-0.231602263022381,0.0066461470035044,
-0.0109008810664884));
#26619=CARTESIAN_POINT('Ctrl Pts',(-0.231644664597747,0.00659866149517143,
-0.0108973277547739));
#26620=CARTESIAN_POINT('Ctrl Pts',(-0.231786496142884,0.00643900367334659,
-0.0108830165106154));
#26621=CARTESIAN_POINT('Ctrl Pts',(-0.231931242135863,0.00627498686834051,
-0.0108651664231131));
#26622=CARTESIAN_POINT('Ctrl Pts',(-0.232108355058939,0.006072781544978,
-0.0108393204957513));
#26623=CARTESIAN_POINT('Ctrl Pts',(-0.232300210417243,0.00584995171828157,
-0.0108039990190336));
#26624=CARTESIAN_POINT('Ctrl Pts',(-0.232440153445732,0.00568521883709722,
-0.0107749745621213));
#26625=CARTESIAN_POINT('Ctrl Pts',(-0.232667681706468,0.00540944023166544,
-0.0107186770907011));
#26626=CARTESIAN_POINT('Ctrl Pts',(-0.232852296030784,0.00517740019893589,
-0.0106633253293673));
#26627=CARTESIAN_POINT('Ctrl Pts',(-0.233034515083928,0.00493973862584453,
-0.0105996345989168));
#26628=CARTESIAN_POINT('Ctrl Pts',(-0.233182763373576,0.0047393646700024,
-0.0105407789701458));
#26629=CARTESIAN_POINT('Ctrl Pts',(-0.233382824203779,0.00445405678985819,
-0.0104474408102256));
#26630=CARTESIAN_POINT('Ctrl Pts',(-0.233543139477693,0.00420824923383913,
-0.0103572130276457));
#26631=CARTESIAN_POINT('Ctrl Pts',(-0.233691663906295,0.00396150500429967,
-0.0102577963056457));
#26632=CARTESIAN_POINT('Ctrl Pts',(-0.233808136742523,0.00375087363724476,
-0.0101661685139463));
#26633=CARTESIAN_POINT('Ctrl Pts',(-0.233945646263649,0.00346795331697028,
-0.0100321308653909));
#26634=CARTESIAN_POINT('Ctrl Pts',(-0.234083992220015,0.00312423902231311,
-0.00985264023662205));
#26635=CARTESIAN_POINT('Ctrl Pts',(-0.234256483655326,0.00254094086020491,
-0.00951179687589967));
#26636=CARTESIAN_POINT('Ctrl Pts',(-0.234262850553755,0.00186094978727132,
-0.00900885554389722));
#26637=CARTESIAN_POINT('Ctrl Pts',(-0.234068396622431,0.00128735914064042,
-0.00848231918710256));
#26638=CARTESIAN_POINT('Ctrl Pts',(-0.233817874309389,0.000881927623917763,
-0.00805541563716329));
#26639=CARTESIAN_POINT('Ctrl Pts',(-0.2335704994029,0.000620516072173728,
-0.00774327437066843));
#26640=CARTESIAN_POINT('Ctrl Pts',(-0.233329249078638,0.000415582269566412,
-0.00747932099276584));
#26641=CARTESIAN_POINT('Ctrl Pts',(-0.233112960961304,0.000260399852082621,
-0.00726601341584551));
#26642=CARTESIAN_POINT('Ctrl Pts',(-0.23293403930091,0.000146997261486484,
-0.00710214095492278));
#26643=CARTESIAN_POINT('Ctrl Pts',(-0.232690819740965,8.6463822485961E-6,
-0.00689139571371004));
#26644=CARTESIAN_POINT('Ctrl Pts',(-0.232534580033651,-7.16401286118548E-5,
-0.00676206118639177));
#26645=CARTESIAN_POINT('Ctrl Pts',(-0.232384733682554,-0.00014564407532251,
-0.00663951871985647));
#26646=CARTESIAN_POINT('Ctrl Pts',(-0.232246570420582,-0.000210741619390237,
-0.00652795918919056));
#26647=CARTESIAN_POINT('Ctrl Pts',(-0.2321756309133,-0.00024311721387142,
-0.00647117665620728));
#26648=CARTESIAN_POINT('Ctrl Pts',(-0.232027018331408,-0.000309581030025878,
-0.00635248279855617));
#26649=CARTESIAN_POINT('Ctrl Pts',(-0.231873513645315,-0.000375942995292352,
-0.00623044356967292));
#26650=CARTESIAN_POINT('Ctrl Pts',(-0.231629252180028,-0.000476033427381937,
-0.00603466477165482));
#26651=CARTESIAN_POINT('Ctrl Pts',(-0.231501652837513,-0.000526562181469526,
-0.00593145040725404));
#26652=CARTESIAN_POINT('Ctrl Pts',(-0.231423161461155,-0.000557113181751774,
-0.00586770399101785));
#26653=CARTESIAN_POINT('Ctrl Pts',(-0.231370959763619,-0.000577174803723653,
-0.00582510216694446));
#26654=CARTESIAN_POINT('Ctrl Pts',(-0.23136223630703,-0.000580549023227225,
-0.00581801997224131));
#26655=CARTESIAN_POINT('Ctrl Pts',(-0.231279110464189,-0.000612251054423109,
-0.00574980208365006));
#26656=CARTESIAN_POINT('Ctrl Pts',(-0.231196728277073,-0.000643235046653219,
-0.0056816723984767));
#26657=CARTESIAN_POINT('Ctrl Pts',(-0.231045192907986,-0.000699432810574991,
-0.00555531580229769));
#26658=CARTESIAN_POINT('Ctrl Pts',(-0.230851532314107,-0.000768988555986341,
-0.00539073770637673));
#26659=CARTESIAN_POINT('Ctrl Pts',(-0.230632644958823,-0.000844755027883067,
-0.00519931949444886));
#26660=CARTESIAN_POINT('Ctrl Pts',(-0.230464821727732,-0.000901324892749503,
-0.00504914540426946));
#26661=CARTESIAN_POINT('Ctrl Pts',(-0.230220831803887,-0.000981615469461095,
-0.00482173766606306));
#26662=CARTESIAN_POINT('Ctrl Pts',(-0.229938496083015,-0.00107153756204175,
-0.00454364289308824));
#26663=CARTESIAN_POINT('Ctrl Pts',(-0.22947806967778,-0.00121182703178667,
-0.00405820411123181));
#26664=CARTESIAN_POINT('Ctrl Pts',(-0.228966516318197,-0.00134816943216903,
-0.0034170007972907));
#26665=CARTESIAN_POINT('Ctrl Pts',(-0.228579626600758,-0.00142248587384968,
-0.00284576218835118));
#26666=CARTESIAN_POINT('Ctrl Pts',(-0.228348114652924,-0.00145443014710487,
-0.00247619241680766));
#26667=CARTESIAN_POINT('Ctrl Pts',(-0.228153271627853,-0.00147191766978348,
-0.00214698541707847));
#26668=CARTESIAN_POINT('Ctrl Pts',(-0.227950831685064,-0.00149080064913227,
-0.00177093667718264));
#26669=CARTESIAN_POINT('Ctrl Pts',(-0.227785980543934,-0.00150568050665454,
-0.0014278840996034));
#26670=CARTESIAN_POINT('Ctrl Pts',(-0.227652169250544,-0.00151706650701674,
-0.0011265269211914));
#26671=CARTESIAN_POINT('Ctrl Pts',(-0.227566987533402,-0.00152351882163508,
-0.000920126530996759));
#26672=CARTESIAN_POINT('Ctrl Pts',(-0.227491225966645,-0.00152867067867476,
-0.000731050631136379));
#26673=CARTESIAN_POINT('Ctrl Pts',(-0.22742256682371,-0.00153264846383891,
-0.000554599488887733));
#26674=CARTESIAN_POINT('Ctrl Pts',(-0.227392474361708,-0.00153416030791209,
-0.000475545942274294));
#26675=CARTESIAN_POINT('Ctrl Pts',(-0.227323585473763,-0.00153729398439594,
-0.000293428211194043));
#26676=CARTESIAN_POINT('Ctrl Pts',(-0.227262110333096,-0.00153920870389092,
-0.00012867603536092));
#26677=CARTESIAN_POINT('Ctrl Pts',(-0.227214261715267,-0.00153995361067246,
2.08417333140297E-7));
#26678=CARTESIAN_POINT('',(-0.228146745678798,-0.00146986864564724,0.00219071825850764));
#26679=CARTESIAN_POINT('Ctrl Pts',(-0.227214261703447,-0.00153995361085648,
2.08449182843721E-7));
#26680=CARTESIAN_POINT('Ctrl Pts',(-0.227260878765733,-0.00153922641144584,
0.000127297385581003));
#26681=CARTESIAN_POINT('Ctrl Pts',(-0.227320680330025,-0.00153736227316047,
0.000289652208553862));
#26682=CARTESIAN_POINT('Ctrl Pts',(-0.227387409157731,-0.00153432194063922,
0.000468825060106595));
#26683=CARTESIAN_POINT('Ctrl Pts',(-0.227416469548984,-0.00153285820742312,
0.000546456828516538));
#26684=CARTESIAN_POINT('Ctrl Pts',(-0.227482475446119,-0.00152901542348585,
0.00071963165722293));
#26685=CARTESIAN_POINT('Ctrl Pts',(-0.22755518908399,-0.00152402406154442,
0.000905839279240665));
#26686=CARTESIAN_POINT('Ctrl Pts',(-0.227636477856155,-0.00151777931669379,
0.00110910239215292));
#26687=CARTESIAN_POINT('Ctrl Pts',(-0.227764726003692,-0.0015065682063797,
0.00141079945586991));
#26688=CARTESIAN_POINT('Ctrl Pts',(-0.227915639874086,-0.00149228529545111,
0.0017430864187612));
#26689=CARTESIAN_POINT('Ctrl Pts',(-0.228055314183631,-0.0014789629619799,
0.00201933604813241));
#26690=CARTESIAN_POINT('Ctrl Pts',(-0.228146745678798,-0.00146986864564724,
0.00219071825850764));
#26691=CARTESIAN_POINT('',(-0.233559158081792,0.00387416783145173,0.0102155391996269));
#26692=CARTESIAN_POINT('Ctrl Pts',(-0.228146745678798,-0.00146986864564724,
0.00219071825850764));
#26693=CARTESIAN_POINT('Ctrl Pts',(-0.228147602077471,-0.00146978346317885,
0.0021923235204298));
#26694=CARTESIAN_POINT('Ctrl Pts',(-0.22824073305991,-0.0014605164879658,
0.00236679973700088));
#26695=CARTESIAN_POINT('Ctrl Pts',(-0.228423001865608,-0.00144158884393021,
0.00268844823641635));
#26696=CARTESIAN_POINT('Ctrl Pts',(-0.228762913960931,-0.00137415185924898,
0.00323117458741793));
#26697=CARTESIAN_POINT('Ctrl Pts',(-0.229113014450919,-0.00128145526964443,
0.00373771571845669));
#26698=CARTESIAN_POINT('Ctrl Pts',(-0.229472512500946,-0.00117031797297195,
0.00420354730297736));
#26699=CARTESIAN_POINT('Ctrl Pts',(-0.229771684855995,-0.00106991162198901,
0.00455062609318909));
#26700=CARTESIAN_POINT('Ctrl Pts',(-0.230037581767111,-0.000975694344253686,
0.00484005819884158));
#26701=CARTESIAN_POINT('Ctrl Pts',(-0.230268198085539,-0.000890512288748131,
0.00507885332770519));
#26702=CARTESIAN_POINT('Ctrl Pts',(-0.230434510419619,-0.000827067762574278,
0.00524460327337801));
#26703=CARTESIAN_POINT('Ctrl Pts',(-0.230638435249322,-0.000747124311760387,
0.00544285167783606));
#26704=CARTESIAN_POINT('Ctrl Pts',(-0.230820428072529,-0.00067292550390027,
0.00561426715448736));
#26705=CARTESIAN_POINT('Ctrl Pts',(-0.230968589245136,-0.00061090734263518,
0.0057512581323597));
#26706=CARTESIAN_POINT('Ctrl Pts',(-0.231102505812003,-0.000553517619805691,
0.00587311727066912));
#26707=CARTESIAN_POINT('Ctrl Pts',(-0.231169109311276,-0.000524526572001451,
0.00593304385290676));
#26708=CARTESIAN_POINT('Ctrl Pts',(-0.231310613527498,-0.000461990851617312,
0.00605961198957369));
#26709=CARTESIAN_POINT('Ctrl Pts',(-0.231447457908593,-0.000400412033682357,
0.00618086667324984));
#26710=CARTESIAN_POINT('Ctrl Pts',(-0.231691440631806,-0.000284675731091188,
0.00639373778767496));
#26711=CARTESIAN_POINT('Ctrl Pts',(-0.231813023978218,-0.00022486405856557,
0.00649884984694274));
#26712=CARTESIAN_POINT('Ctrl Pts',(-0.231884446809911,-0.000189209465118761,
0.00656034920502148));
#26713=CARTESIAN_POINT('Ctrl Pts',(-0.231930078039368,-0.000166097177273578,
0.00659958595864139));
#26714=CARTESIAN_POINT('Ctrl Pts',(-0.231931289957848,-0.000165561101604138,
0.00660060687576811));
#26715=CARTESIAN_POINT('Ctrl Pts',(-0.232013321018402,-0.000123494859710195,
0.00667129148969066));
#26716=CARTESIAN_POINT('Ctrl Pts',(-0.232089020337746,-8.38348221208054E-5,
0.00673658587661242));
#26717=CARTESIAN_POINT('Ctrl Pts',(-0.232184758140682,-3.26941779414291E-5,
0.00681932067970241));
#26718=CARTESIAN_POINT('Ctrl Pts',(-0.232285526066454,2.31781819879938E-5,
0.006907053513387));
#26719=CARTESIAN_POINT('Ctrl Pts',(-0.232387404877587,8.09008443525465E-5,
0.00699635079756444));
#26720=CARTESIAN_POINT('Ctrl Pts',(-0.232596018354059,0.000207336010577208,
0.00718429347931461));
#26721=CARTESIAN_POINT('Ctrl Pts',(-0.232761955293696,0.00031852348252791,
0.00734069697033025));
#26722=CARTESIAN_POINT('Ctrl Pts',(-0.232977684545184,0.000479357868993146,
0.00755646663238428));
#26723=CARTESIAN_POINT('Ctrl Pts',(-0.233216413918051,0.000686789932042174,
0.00781703214787861));
#26724=CARTESIAN_POINT('Ctrl Pts',(-0.233465871951339,0.000950568046321459,
0.0081241062900768));
#26725=CARTESIAN_POINT('Ctrl Pts',(-0.233724009566518,0.00134408173329303,
0.00853029830649302));
#26726=CARTESIAN_POINT('Ctrl Pts',(-0.233947136086876,0.00191722301985356,
0.00904721293907608));
#26727=CARTESIAN_POINT('Ctrl Pts',(-0.233978600563923,0.0025686995100556,
0.00952461220572329));
#26728=CARTESIAN_POINT('Ctrl Pts',(-0.233824605334425,0.00326097954767997,
0.00992663531592156));
#26729=CARTESIAN_POINT('Ctrl Pts',(-0.233668400615857,0.00364781188257956,
0.0101152447960562));
#26730=CARTESIAN_POINT('Ctrl Pts',(-0.23357525881827,0.0038415964420142,
0.0102013285012318));
#26731=CARTESIAN_POINT('Ctrl Pts',(-0.233559158081792,0.00387416783145173,
0.0102155391996269));
#26732=CARTESIAN_POINT('',(-0.230731189036971,0.00749156929015138,0.0109223560943954));
#26733=CARTESIAN_POINT('Ctrl Pts',(-0.233559158081792,0.00387416783145173,
0.0102155391996269));
#26734=CARTESIAN_POINT('Ctrl Pts',(-0.23349648849709,0.00400094684258756,
0.0102708521083235));
#26735=CARTESIAN_POINT('Ctrl Pts',(-0.233387193213595,0.00419960150239789,
0.0103510897124964));
#26736=CARTESIAN_POINT('Ctrl Pts',(-0.233204445962594,0.00449845474264293,
0.0104595791887194));
#26737=CARTESIAN_POINT('Ctrl Pts',(-0.233016552168204,0.00477901086038231,
0.0105498350650121));
#26738=CARTESIAN_POINT('Ctrl Pts',(-0.232874853074723,0.00497762326969598,
0.0106073454722064));
#26739=CARTESIAN_POINT('Ctrl Pts',(-0.232699278541195,0.00521304060449747,
0.0106694214007349));
#26740=CARTESIAN_POINT('Ctrl Pts',(-0.232519935104301,0.00544312585676357,
0.0107234137638662));
#26741=CARTESIAN_POINT('Ctrl Pts',(-0.232296466758271,0.0057176608256759,
0.0107784200472414));
#26742=CARTESIAN_POINT('Ctrl Pts',(-0.2321601909895,0.005879437380212,0.0108063414559013));
#26743=CARTESIAN_POINT('Ctrl Pts',(-0.231972161329767,0.00609921295264491,
0.0108404751193834));
#26744=CARTESIAN_POINT('Ctrl Pts',(-0.231798532022978,0.00629809753013036,
0.0108653480625757));
#26745=CARTESIAN_POINT('Ctrl Pts',(-0.231656082292353,0.00645982495895992,
0.0108825388725517));
#26746=CARTESIAN_POINT('Ctrl Pts',(-0.231517490918546,0.00661596135611126,
0.0108962031604773));
#26747=CARTESIAN_POINT('Ctrl Pts',(-0.23147265186694,0.0066661781042074,
0.0108998770348921));
#26748=CARTESIAN_POINT('Ctrl Pts',(-0.231363974605798,0.00678783230812327,
0.0109084325591462));
#26749=CARTESIAN_POINT('Ctrl Pts',(-0.231157030865224,0.00701863801538526,
0.0109208112149785));
#26750=CARTESIAN_POINT('Ctrl Pts',(-0.230916142610404,0.00728648998098758,
0.0109263403628976));
#26751=CARTESIAN_POINT('Ctrl Pts',(-0.230731189036971,0.00749156929015138,
0.0109223560943954));
#26752=CARTESIAN_POINT('Ctrl Pts',(-0.230731256923034,0.00749164497516978,
0.0109223577006114));
#26753=CARTESIAN_POINT('Ctrl Pts',(-0.230865473404667,0.00764128056035402,
0.0109255326522603));
#26754=CARTESIAN_POINT('Ctrl Pts',(-0.231137213619827,0.007943171205309,
0.0109239758885947));
#26755=CARTESIAN_POINT('Ctrl Pts',(-0.231527434485224,0.00837845914315948,
0.0109008726614748));
#26756=CARTESIAN_POINT('Ctrl Pts',(-0.231887509950401,0.00879119523216391,
0.0108567873229259));
#26757=CARTESIAN_POINT('Ctrl Pts',(-0.232140469910439,0.00909048844268248,
0.010811556341717));
#26758=CARTESIAN_POINT('Ctrl Pts',(-0.232300596136593,0.00928297039316321,
0.0107785093165595));
#26759=CARTESIAN_POINT('Ctrl Pts',(-0.232520666812517,0.00955532757019838,
0.0107237698902202));
#26760=CARTESIAN_POINT('Ctrl Pts',(-0.232703137061035,0.00979022573944132,
0.0106686900691618));
#26761=CARTESIAN_POINT('Ctrl Pts',(-0.232879255800725,0.01002672215703,
0.0106061668367168));
#26762=CARTESIAN_POINT('Ctrl Pts',(-0.233021572234454,0.0102258389513203,
0.0105483766090537));
#26763=CARTESIAN_POINT('Ctrl Pts',(-0.233208640632173,0.0105045789283705,
0.0104586041345504));
#26764=CARTESIAN_POINT('Ctrl Pts',(-0.233412050346818,0.0108382118461368,
0.0103371779477693));
#26765=CARTESIAN_POINT('Ctrl Pts',(-0.233613248968386,0.0112102121412998,
0.0101851544377368));
#26766=CARTESIAN_POINT('Ctrl Pts',(-0.233834860767148,0.0117711747306955,
0.00990917052441051));
#26767=CARTESIAN_POINT('Ctrl Pts',(-0.233983453677809,0.0124159974365663,
0.00953355738971462));
#26768=CARTESIAN_POINT('Ctrl Pts',(-0.233945755044452,0.0131099715084786,
0.00902520045927226));
#26769=CARTESIAN_POINT('Ctrl Pts',(-0.233729334532907,0.0136536630448554,
0.00853186537754338));
#26770=CARTESIAN_POINT('Ctrl Pts',(-0.233466543057227,0.0140565862100828,
0.00811722384353614));
#26771=CARTESIAN_POINT('Ctrl Pts',(-0.233203818000884,0.0143303903479438,
0.00779638666024062));
#26772=CARTESIAN_POINT('Ctrl Pts',(-0.232969475121551,0.0145316536102632,
0.00754200761475823));
#26773=CARTESIAN_POINT('Ctrl Pts',(-0.232762493362533,0.0146856837232449,
0.00733514778261602));
#26774=CARTESIAN_POINT('Ctrl Pts',(-0.232616233535089,0.0147821994045361,
0.00719838339891441));
#26775=CARTESIAN_POINT('Ctrl Pts',(-0.232480708209145,0.0148666127866986,
0.00707499743246925));
#26776=CARTESIAN_POINT('Ctrl Pts',(-0.232356994919711,0.0149394474803228,
0.00696495782458427));
#26777=CARTESIAN_POINT('Ctrl Pts',(-0.232289559739574,0.014977518626712,
0.00690602252937239));
#26778=CARTESIAN_POINT('Ctrl Pts',(-0.23218861866623,0.0150333261724313,
0.00681837562717864));
#26779=CARTESIAN_POINT('Ctrl Pts',(-0.23209277942457,0.0150844247157454,
0.00673569208947289));
#26780=CARTESIAN_POINT('Ctrl Pts',(-0.232015087271052,0.0151250700285569,
0.00666873519572026));
#26781=CARTESIAN_POINT('Ctrl Pts',(-0.23193248413974,0.0151673972827789,
0.00659755450821913));
#26782=CARTESIAN_POINT('Ctrl Pts',(-0.23192477458317,0.0151712366444997,
0.00659092566948877));
#26783=CARTESIAN_POINT('Ctrl Pts',(-0.231874843378034,0.0151964734507034,
0.00654794895099817));
#26784=CARTESIAN_POINT('Ctrl Pts',(-0.231801186064193,0.0152331557486462,
0.00648446076737892));
#26785=CARTESIAN_POINT('Ctrl Pts',(-0.231680565445703,0.0152922140924725,
0.0063800594780042));
#26786=CARTESIAN_POINT('Ctrl Pts',(-0.231456644767689,0.0153983363574462,
0.00618473126690153));
#26787=CARTESIAN_POINT('Ctrl Pts',(-0.231287273794767,0.0154745756686466,
0.00603488776572405));
#26788=CARTESIAN_POINT('Ctrl Pts',(-0.231151897129242,0.0155338645319709,
0.00591370665668096));
#26789=CARTESIAN_POINT('Ctrl Pts',(-0.231105123945984,0.0155541968768278,
0.00587172310084077));
#26790=CARTESIAN_POINT('Ctrl Pts',(-0.230963177640927,0.0156149638966239,
0.00574254549492409));
#26791=CARTESIAN_POINT('Ctrl Pts',(-0.230814830287228,0.0156768473199735,
0.00560537069730955));
#26792=CARTESIAN_POINT('Ctrl Pts',(-0.230630359191633,0.0157517758844927,
0.00543176645051644));
#26793=CARTESIAN_POINT('Ctrl Pts',(-0.230426865261854,0.0158311425106513,
0.00523416260499648));
#26794=CARTESIAN_POINT('Ctrl Pts',(-0.230262165941671,0.0158936258990308,
0.00507035518297227));
#26795=CARTESIAN_POINT('Ctrl Pts',(-0.230036237901951,0.0159768319316395,
0.00483654815190377));
#26796=CARTESIAN_POINT('Ctrl Pts',(-0.229773023242685,0.0160702611120349,
0.00454967053487877));
#26797=CARTESIAN_POINT('Ctrl Pts',(-0.229347345537255,0.0162132627607145,
0.00405272807923008));
#26798=CARTESIAN_POINT('Ctrl Pts',(-0.228795080335764,0.0163782893771517,
0.00329870162389577));
#26799=CARTESIAN_POINT('Ctrl Pts',(-0.228391997949756,0.0164411429389733,
0.00263302315211825));
#26800=CARTESIAN_POINT('Ctrl Pts',(-0.228219847986792,0.016461711610013,
0.00232234304728456));
#26801=CARTESIAN_POINT('Ctrl Pts',(-0.185723055456904,0.00596900147723498,
0.00978267384703966));
#26802=CARTESIAN_POINT('Ctrl Pts',(-0.23232670433304,0.00586421401192308,
0.0108066948117815));
#26803=CARTESIAN_POINT('Ctrl Pts',(-0.185723055456904,0.00647508645933998,
0.00986397141884284));
#26804=CARTESIAN_POINT('Ctrl Pts',(-0.23232670433304,0.00640326228709296,
0.0109072089909106));
#26805=CARTESIAN_POINT('Ctrl Pts',(-0.185723055456904,0.00806363535647837,
0.00999158316816427));
#26806=CARTESIAN_POINT('Ctrl Pts',(-0.23232670433304,0.00810313394959613,
0.011065956770795));
#26807=CARTESIAN_POINT('Ctrl Pts',(-0.185723055456904,0.0107282763804236,
0.00954209216522276));
#26808=CARTESIAN_POINT('Ctrl Pts',(-0.232326704333039,0.010954508418149,
0.0105067943176979));
#26809=CARTESIAN_POINT('Ctrl Pts',(-0.185723055456904,0.0136025641905403,
0.00796594412564821));
#26810=CARTESIAN_POINT('Ctrl Pts',(-0.23232670433304,0.0138912062742137,
0.00858048215857484));
#26811=CARTESIAN_POINT('Ctrl Pts',(-0.185723055456904,0.0158049553585666,
0.0055255423033021));
#26812=CARTESIAN_POINT('Ctrl Pts',(-0.232326704333039,0.0158790519814133,
0.00570322651640249));
#26813=CARTESIAN_POINT('Ctrl Pts',(-0.185723055456903,0.0166573800152265,
0.00349659872621015));
#26814=CARTESIAN_POINT('Ctrl Pts',(-0.232326704333039,0.0163854748419429,
0.00344344619705094));
#26815=CARTESIAN_POINT('Ctrl Pts',(-0.185723055456903,0.0169037490465727,
0.00243669718465325));
#26816=CARTESIAN_POINT('Ctrl Pts',(-0.232326704333039,0.0164203047763951,
0.00231142721965168));
#26817=CARTESIAN_POINT('Ctrl Pts',(-0.185723055456903,0.0169917319681535,
0.0020581868105832));
#26818=CARTESIAN_POINT('Ctrl Pts',(-0.232326704333039,0.0164327431878904,
0.00190716238014556));
#26819=CARTESIAN_POINT('Ctrl Pts',(-0.185723055456904,0.0171348389058692,
0.00126455176521327));
#26820=CARTESIAN_POINT('Ctrl Pts',(-0.232326704333039,0.0164529746481233,
0.00113116956517427));
#26821=CARTESIAN_POINT('Ctrl Pts',(-0.185723055456903,0.0172123852537007,
-4.57104323127425E-14));
#26822=CARTESIAN_POINT('Ctrl Pts',(-0.232326704333039,0.0164639376096499,
-5.12643732643055E-15));
#26823=CARTESIAN_POINT('Ctrl Pts',(-0.185723055456904,0.0171348389058572,
-0.00126455176530287));
#26824=CARTESIAN_POINT('Ctrl Pts',(-0.232326704333039,0.0164529746481216,
-0.00113116956518479));
#26825=CARTESIAN_POINT('Ctrl Pts',(-0.185723055456903,0.0169917319681347,
-0.00205818681066974));
#26826=CARTESIAN_POINT('Ctrl Pts',(-0.232326704333039,0.0164327431878878,
-0.00190716238015681));
#26827=CARTESIAN_POINT('Ctrl Pts',(-0.185723055456903,0.0166573800151943,
-0.00349659872622789));
#26828=CARTESIAN_POINT('Ctrl Pts',(-0.232326704333039,0.0163854748419384,
-0.00344344619644609));
#26829=CARTESIAN_POINT('Ctrl Pts',(-0.185723055456904,0.0158049536659853,
-0.00552554202981291));
#26830=CARTESIAN_POINT('Ctrl Pts',(-0.23232670433304,0.0158790365063827,
-0.00570322401511438));
#26831=CARTESIAN_POINT('Ctrl Pts',(-0.185723055456903,0.0136025708308564,
-0.00796594412460981));
#26832=CARTESIAN_POINT('Ctrl Pts',(-0.232326704333039,0.0138912669883084,
-0.00858048214849728));
#26833=CARTESIAN_POINT('Ctrl Pts',(-0.185723055456904,0.0107282744647946,
-0.00954209114738551));
#26834=CARTESIAN_POINT('Ctrl Pts',(-0.23232670433304,0.0109544909042364,
-0.010506785011137));
#26835=CARTESIAN_POINT('Ctrl Pts',(-0.185723055456903,0.00749999999987153,
-0.0100866616277759));
#26836=CARTESIAN_POINT('Ctrl Pts',(-0.232326704333039,0.00749999999987138,
-0.0111842362468306));
#26837=CARTESIAN_POINT('Ctrl Pts',(-0.185723055456904,0.00427172553496278,
-0.00954209114730134));
#26838=CARTESIAN_POINT('Ctrl Pts',(-0.23232670433304,0.00404550909552549,
-0.0105067850110401));
#26839=CARTESIAN_POINT('Ctrl Pts',(-0.185723055456903,0.00139742916894219,
-0.0079659441244508));
#26840=CARTESIAN_POINT('Ctrl Pts',(-0.232326704333039,0.00110873301150744,
-0.00858048214831799));
#26841=CARTESIAN_POINT('Ctrl Pts',(-0.185723055456904,-0.000804953666122893,
-0.00552554202959671));
#26842=CARTESIAN_POINT('Ctrl Pts',(-0.23232670433304,-0.000879036506486045,
-0.00570322401487933));
#26843=CARTESIAN_POINT('Ctrl Pts',(-0.185723055456903,-0.00165738001527906,
-0.00349659872598971));
#26844=CARTESIAN_POINT('Ctrl Pts',(-0.232326704333039,-0.0013854748419783,
-0.00344344619619682));
#26845=CARTESIAN_POINT('Ctrl Pts',(-0.185723055456903,-0.00199173196817847,
-0.00205818681044279));
#26846=CARTESIAN_POINT('Ctrl Pts',(-0.232326704333039,-0.00143274318789395,
-0.00190716237992731));
#26847=CARTESIAN_POINT('Ctrl Pts',(-0.185723055456903,-0.00213483890587743,
-0.00126455176511326));
#26848=CARTESIAN_POINT('Ctrl Pts',(-0.232326704333039,-0.00145297464812447,
-0.001131169564997));
#26849=CARTESIAN_POINT('Ctrl Pts',(-0.185723055456904,-0.00221238525369828,
8.33588010327838E-14));
#26850=CARTESIAN_POINT('Ctrl Pts',(-0.232326704333039,-0.0014639376096495,
1.20148665217339E-13));
#26851=CARTESIAN_POINT('Ctrl Pts',(-0.185723055456903,-0.00213483890585875,
0.00126455176527974));
#26852=CARTESIAN_POINT('Ctrl Pts',(-0.232326704333039,-0.00145297464812182,
0.00113116956523674));
#26853=CARTESIAN_POINT('Ctrl Pts',(-0.185723055456903,-0.00199173196814768,
0.00205818681060856));
#26854=CARTESIAN_POINT('Ctrl Pts',(-0.232326704333039,-0.0014327431878896,
0.00190716238016579));
#26855=CARTESIAN_POINT('Ctrl Pts',(-0.185723055456903,-0.00165738001522438,
0.00349659872621544));
#26856=CARTESIAN_POINT('Ctrl Pts',(-0.232326704333039,-0.00138547484194287,
0.00344344619705013));
#26857=CARTESIAN_POINT('Ctrl Pts',(-0.185723055456904,-0.000804955358563482,
0.00552554230330677));
#26858=CARTESIAN_POINT('Ctrl Pts',(-0.232326704333039,-0.000879051981413446,
0.0057032265164018));
#26859=CARTESIAN_POINT('Ctrl Pts',(-0.185723055456903,0.00139743580946407,
0.00796594412565152));
#26860=CARTESIAN_POINT('Ctrl Pts',(-0.232326704333039,0.00110879372578601,
0.00858048215857438));
#26861=CARTESIAN_POINT('Ctrl Pts',(-0.185723055456904,0.00381545901438577,
0.00929189433866225));
#26862=CARTESIAN_POINT('Ctrl Pts',(-0.232326704333039,0.00357932000252583,
0.0102010114195229));
#26863=CARTESIAN_POINT('Ctrl Pts',(-0.185723055456904,0.0054123742536131,
0.00969325716154195));
#26864=CARTESIAN_POINT('Ctrl Pts',(-0.232326704333039,0.00527133148148726,
0.0106961423740653));
#26865=CARTESIAN_POINT('Ctrl Pts',(-0.185723055456904,0.00596900147723498,
0.00978267384703966));
#26866=CARTESIAN_POINT('Ctrl Pts',(-0.23232670433304,0.00586421401192308,
0.0108066948117815));
#26867=CARTESIAN_POINT('',(-0.225761332775488,0.0164871798990637,0.00232893089033033));
#26868=CARTESIAN_POINT('',(-0.220090794747946,0.0165472343306677,0.00234431717574848));
#26869=CARTESIAN_POINT('Ctrl Pts',(-0.225761208631098,0.0164884121318173,
0.00232907518148799));
#26870=CARTESIAN_POINT('Ctrl Pts',(-0.220090794747946,0.0165472343306677,
0.00234431717574846));
#26871=CARTESIAN_POINT('',(-0.229322271958198,0.00910280340307597,0.0107454877379686));
#26872=CARTESIAN_POINT('Ctrl Pts',(-0.225761332775488,0.0164871798990637,
0.00232893089033043));
#26873=CARTESIAN_POINT('Ctrl Pts',(-0.225868813295687,0.0164702811459343,
0.00256572214437089));
#26874=CARTESIAN_POINT('Ctrl Pts',(-0.226137029027792,0.0164201503719644,
0.00311230936225717));
#26875=CARTESIAN_POINT('Ctrl Pts',(-0.226622346737041,0.0162529713835771,
0.00396894829373893));
#26876=CARTESIAN_POINT('Ctrl Pts',(-0.227136114083267,0.0160270537581582,
0.00471718824932398));
#26877=CARTESIAN_POINT('Ctrl Pts',(-0.227548052020872,0.015830334783286,
0.00523800076883081));
#26878=CARTESIAN_POINT('Ctrl Pts',(-0.227904933514641,0.0156518603798053,
0.00565166468326421));
#26879=CARTESIAN_POINT('Ctrl Pts',(-0.22824506964293,0.0154746912800295,
0.00601507791742848));
#26880=CARTESIAN_POINT('Ctrl Pts',(-0.228618690523152,0.0152744254805032,
0.0063844617087714));
#26881=CARTESIAN_POINT('Ctrl Pts',(-0.228906681001303,0.0151174744578315,
0.00664687659885061));
#26882=CARTESIAN_POINT('Ctrl Pts',(-0.22916173971917,0.0149769237018957,
0.00686832718740545));
#26883=CARTESIAN_POINT('Ctrl Pts',(-0.229386887100392,0.014851110571812,
0.00705580393505498));
#26884=CARTESIAN_POINT('Ctrl Pts',(-0.229526845406411,0.0147725603957695,
0.00716898590139015));
#26885=CARTESIAN_POINT('Ctrl Pts',(-0.22985665337706,0.0145837017217628,
0.00742915055021459));
#26886=CARTESIAN_POINT('Ctrl Pts',(-0.230067756669372,0.0144588911103182,
0.00758975272001023));
#26887=CARTESIAN_POINT('Ctrl Pts',(-0.230390189204541,0.0142582866306812,
0.00783304005481369));
#26888=CARTESIAN_POINT('Ctrl Pts',(-0.230587131929265,0.0141279794172046,
0.00798292444616597));
#26889=CARTESIAN_POINT('Ctrl Pts',(-0.230774468781011,0.013996606095421,
0.0081276487410968));
#26890=CARTESIAN_POINT('Ctrl Pts',(-0.230911642843167,0.013896223101725,
0.0082349516180805));
#26891=CARTESIAN_POINT('Ctrl Pts',(-0.231125605978502,0.013724550906806,
0.00840987345810032));
#26892=CARTESIAN_POINT('Ctrl Pts',(-0.231269225646072,0.0135968959048821,
0.00853388774673025));
#26893=CARTESIAN_POINT('Ctrl Pts',(-0.231454214398683,0.0134066528799722,
0.00870979256612292));
#26894=CARTESIAN_POINT('Ctrl Pts',(-0.231576826440879,0.0132527642207034,
0.00884432583919974));
#26895=CARTESIAN_POINT('Ctrl Pts',(-0.231699073871839,0.0130506469508559,
0.00901193941612837));
#26896=CARTESIAN_POINT('Ctrl Pts',(-0.231797984546367,0.0127794807589124,
0.00922301260208771));
#26897=CARTESIAN_POINT('Ctrl Pts',(-0.231797546311281,0.0124463550028915,
0.0094545189472133));
#26898=CARTESIAN_POINT('Ctrl Pts',(-0.231726490190532,0.01220148485762,
0.00960823702894843));
#26899=CARTESIAN_POINT('Ctrl Pts',(-0.231639005765325,0.0119843290682612,
0.00973688624094698));
#26900=CARTESIAN_POINT('Ctrl Pts',(-0.231525310404822,0.0117655522917993,
0.00985805531704937));
#26901=CARTESIAN_POINT('Ctrl Pts',(-0.231352361903446,0.0114927855298606,
0.00999609538197112));
#26902=CARTESIAN_POINT('Ctrl Pts',(-0.231244347684152,0.0113413363936371,
0.0100671311393663));
#26903=CARTESIAN_POINT('Ctrl Pts',(-0.231090705799142,0.01113549569015,
0.0101590920502647));
#26904=CARTESIAN_POINT('Ctrl Pts',(-0.230929371790275,0.0109316039033615,
0.0102437095233981));
#26905=CARTESIAN_POINT('Ctrl Pts',(-0.230719165437917,0.0106780079360857,
0.0103396054112657));
#26906=CARTESIAN_POINT('Ctrl Pts',(-0.230586872078737,0.0105231155941536,
0.0103934674402264));
#26907=CARTESIAN_POINT('Ctrl Pts',(-0.230414186940932,0.0103232538972528,
0.0104589357413493));
#26908=CARTESIAN_POINT('Ctrl Pts',(-0.230240646794771,0.0101254517763829,
0.0105184710817764));
#26909=CARTESIAN_POINT('Ctrl Pts',(-0.230026409330978,0.00988432845845099,
0.0105835997465218));
#26910=CARTESIAN_POINT('Ctrl Pts',(-0.229891307016393,0.00973360123118308,
0.0106204354698397));
#26911=CARTESIAN_POINT('Ctrl Pts',(-0.229656258725846,0.00947215625752134,
0.0106797649091995));
#26912=CARTESIAN_POINT('Ctrl Pts',(-0.229463316297648,0.00925865240873361,
0.0107203065532235));
#26913=CARTESIAN_POINT('Ctrl Pts',(-0.229322271958198,0.00910280340307599,
0.0107454877379686));
#26914=CARTESIAN_POINT('',(-0.227992309462812,0.0108760464259574,0.0102016547220559));
#26915=CARTESIAN_POINT('Ctrl Pts',(-0.229322271958198,0.00910280340307614,
0.0107454877379685));
#26916=CARTESIAN_POINT('Ctrl Pts',(-0.229248387424237,0.0091946609993933,
0.0107271294535291));
#26917=CARTESIAN_POINT('Ctrl Pts',(-0.229178401182458,0.00928183676705995,
0.0107081499431178));
#26918=CARTESIAN_POINT('Ctrl Pts',(-0.229120612526884,0.00935384619153853,
0.0106916491124385));
#26919=CARTESIAN_POINT('Ctrl Pts',(-0.22906282387131,0.00942585561601711,
0.0106751482817593));
#26920=CARTESIAN_POINT('Ctrl Pts',(-0.229017225542958,0.00948276183981316,
0.0106614506270637));
#26921=CARTESIAN_POINT('Ctrl Pts',(-0.228958941436709,0.0095562875725616,
0.0106428514999607));
#26922=CARTESIAN_POINT('Ctrl Pts',(-0.22890065733046,0.00962981330531004,
0.0106242523728578));
#26923=CARTESIAN_POINT('Ctrl Pts',(-0.228829699057721,0.0097198395476934,
0.0106002306726335));
#26924=CARTESIAN_POINT('Ctrl Pts',(-0.228770345698383,0.00979561634266397,
0.0105788852380152));
#26925=CARTESIAN_POINT('Ctrl Pts',(-0.228710992339046,0.00987139313763453,
0.0105575398033969));
#26926=CARTESIAN_POINT('Ctrl Pts',(-0.228663232364102,0.00993305883396627,
0.0105393906476383));
#26927=CARTESIAN_POINT('Ctrl Pts',(-0.228604723386985,0.0100100300555052,
0.0105157085654625));
#26928=CARTESIAN_POINT('Ctrl Pts',(-0.228546214409868,0.0100870012770442,
0.0104920264832867));
#26929=CARTESIAN_POINT('Ctrl Pts',(-0.228476966528714,0.0101791433991985,
0.0104623540609925));
#26930=CARTESIAN_POINT('Ctrl Pts',(-0.228414681428224,0.0102636793539038,
0.0104336680888423));
#26931=CARTESIAN_POINT('Ctrl Pts',(-0.228352396327734,0.0103482153086091,
0.0104049821166921));
#26932=CARTESIAN_POINT('Ctrl Pts',(-0.228297067653945,0.0104252427149842,
0.0103775724399405));
#26933=CARTESIAN_POINT('Ctrl Pts',(-0.228243303529506,0.0105019585952468,
0.0103492083290063));
#26934=CARTESIAN_POINT('Ctrl Pts',(-0.228189539405068,0.0105786744755093,
0.010320844218072));
#26935=CARTESIAN_POINT('Ctrl Pts',(-0.228137342432302,0.0106550348405252,
0.0102914062848182));
#26936=CARTESIAN_POINT('Ctrl Pts',(-0.228090589690832,0.0107250747442135,
0.0102634474254206));
#26937=CARTESIAN_POINT('Ctrl Pts',(-0.228062139674782,0.010767695483049,
0.0102464338776888));
#26938=CARTESIAN_POINT('Ctrl Pts',(-0.228035704099044,0.0108079890120059,
0.0102300065388951));
#26939=CARTESIAN_POINT('Ctrl Pts',(-0.228009004449627,0.0108497764912555,
0.0102126270296333));
#26940=CARTESIAN_POINT('Ctrl Pts',(-0.228003457661064,0.0108584577405253,
0.0102090164779849));
#26941=CARTESIAN_POINT('Ctrl Pts',(-0.227997899475325,0.0108672032881771,
0.0102053643805637));
#26942=CARTESIAN_POINT('Ctrl Pts',(-0.227992309462812,0.0108760464259574,
0.0102016547220559));
#26943=CARTESIAN_POINT('',(-0.227099026780033,0.01283031103747,0.00908913013680211));
#26944=CARTESIAN_POINT('Ctrl Pts',(-0.227992309462812,0.0108760464259574,
0.0102016547220559));
#26945=CARTESIAN_POINT('Ctrl Pts',(-0.227980588960823,0.0108945884230957,
0.0101938783175534));
#26946=CARTESIAN_POINT('Ctrl Pts',(-0.227968728545374,0.0109135602167407,
0.0101858506076612));
#26947=CARTESIAN_POINT('Ctrl Pts',(-0.2279565399122,0.0109332710148409,
0.0101774292059006));
#26948=CARTESIAN_POINT('Ctrl Pts',(-0.227910555558433,0.0110076344237606,
0.0101456575780034));
#26949=CARTESIAN_POINT('Ctrl Pts',(-0.227859905396422,0.0110924550180682,
0.0101081303354586));
#26950=CARTESIAN_POINT('Ctrl Pts',(-0.227813773705057,0.0111738765644079,
0.0100706078890561));
#26951=CARTESIAN_POINT('Ctrl Pts',(-0.227767642013693,0.0112552981107476,
0.0100330854426535));
#26952=CARTESIAN_POINT('Ctrl Pts',(-0.22772602561273,0.0113333921774084,
0.00999571733012953));
#26953=CARTESIAN_POINT('Ctrl Pts',(-0.227687001624059,0.0114100817697299,
0.00995776504015784));
#26954=CARTESIAN_POINT('Ctrl Pts',(-0.227647977635389,0.0114867713620514,
0.00991981275018614));
#26955=CARTESIAN_POINT('Ctrl Pts',(-0.227611544765425,0.0115620802269626,
0.00988133589719655));
#26956=CARTESIAN_POINT('Ctrl Pts',(-0.227574056474285,0.0116436347516357,
0.00983810533270652));
#26957=CARTESIAN_POINT('Ctrl Pts',(-0.227536568183146,0.0117251892763089,
0.00979487476821649));
#26958=CARTESIAN_POINT('Ctrl Pts',(-0.227498029236973,0.0118128746272589,
0.009746664582936));
#26959=CARTESIAN_POINT('Ctrl Pts',(-0.227464164954346,0.011892589671401,
0.00970124895034862));
#26960=CARTESIAN_POINT('Ctrl Pts',(-0.22743030067172,0.011972304715543,
0.00965583331776124));
#26961=CARTESIAN_POINT('Ctrl Pts',(-0.227401105512413,0.0120442031594079,
0.00961347988661202));
#26962=CARTESIAN_POINT('Ctrl Pts',(-0.227370538112144,0.0121209395116034,
0.00956682009479379));
#26963=CARTESIAN_POINT('Ctrl Pts',(-0.22735525441201,0.0121593076877011,
0.00954349019888468));
#26964=CARTESIAN_POINT('Ctrl Pts',(-0.227339627918637,0.0121988754292555,
0.00951907014777004));
#26965=CARTESIAN_POINT('Ctrl Pts',(-0.22732271689685,0.0122424277923068,
0.00949166041574463));
#26966=CARTESIAN_POINT('Ctrl Pts',(-0.227305805875064,0.0122859801553581,
0.00946425068371923));
#26967=CARTESIAN_POINT('Ctrl Pts',(-0.22728761252851,0.0123334516519383,
0.00943374365708379));
#26968=CARTESIAN_POINT('Ctrl Pts',(-0.227274223818761,0.012368527112979,
0.00941086715995704));
#26969=CARTESIAN_POINT('Ctrl Pts',(-0.227260835109012,0.0124036025740196,
0.00938799066283029));
#26970=CARTESIAN_POINT('Ctrl Pts',(-0.227252247760813,0.0124263866191674,
0.0093729066453705));
#26971=CARTESIAN_POINT('Ctrl Pts',(-0.227240923007382,0.0124564194502758,
0.0093528274289096));
#26972=CARTESIAN_POINT('Ctrl Pts',(-0.227229598253951,0.0124864522813842,
0.00933274821244871));
#26973=CARTESIAN_POINT('Ctrl Pts',(-0.227215537924042,0.0125236732667803,
0.00930758274915165));
#26974=CARTESIAN_POINT('Ctrl Pts',(-0.227200625928614,0.0125631084337543,
0.00928040810478293));
#26975=CARTESIAN_POINT('Ctrl Pts',(-0.227170806521505,0.0126419666458571,
0.00922606716916939));
#26976=CARTESIAN_POINT('Ctrl Pts',(-0.227137578349285,0.0127297909946739,
0.00916385101444131));
#26977=CARTESIAN_POINT('Ctrl Pts',(-0.227099060731718,0.0128303257879558,
0.00908912033180144));
#26978=CARTESIAN_POINT('',(-0.226399047365308,0.0128166254267281,0.00908546818530889));
#26979=CARTESIAN_POINT('Ctrl Pts',(-0.226399047380228,0.0128166254123418,
0.00908546808718478));
#26980=CARTESIAN_POINT('Ctrl Pts',(-0.226419607262987,0.0128187734864099,
0.00908429865679579));
#26981=CARTESIAN_POINT('Ctrl Pts',(-0.226454462989748,0.0128222624767334,
0.0090824250041845));
#26982=CARTESIAN_POINT('Ctrl Pts',(-0.226486204320344,0.0128250799254038,
0.00908097889269143));
#26983=CARTESIAN_POINT('Ctrl Pts',(-0.226517945651834,0.0128278973741534,
0.00907953278115769));
#26984=CARTESIAN_POINT('Ctrl Pts',(-0.226546572566094,0.0128300440654503,
0.00907851527844382));
#26985=CARTESIAN_POINT('Ctrl Pts',(-0.226573531760671,0.0128318691198156,
0.00907770064679367));
#26986=CARTESIAN_POINT('Ctrl Pts',(-0.226600490955248,0.0128336941741809,
0.00907688601514353));
#26987=CARTESIAN_POINT('Ctrl Pts',(-0.226625782433074,0.0128351974819294,
0.00907627410476947));
#26988=CARTESIAN_POINT('Ctrl Pts',(-0.22665804610537,0.012836295679909,
0.00907609638164778));
#26989=CARTESIAN_POINT('Ctrl Pts',(-0.226690309777666,0.0128373938778886,
0.00907591865852609));
#26990=CARTESIAN_POINT('Ctrl Pts',(-0.226729545644137,0.0128380869755876,
0.00907617513777574));
#26991=CARTESIAN_POINT('Ctrl Pts',(-0.226748701683591,0.0128383575711274,
0.00907635033279388));
#26992=CARTESIAN_POINT('Ctrl Pts',(-0.226758279703318,0.0128384928688973,
0.00907643793030296));
#26993=CARTESIAN_POINT('Ctrl Pts',(-0.226762837766467,0.0128385225347441,
0.00907650519775901));
#26994=CARTESIAN_POINT('Ctrl Pts',(-0.226777364157568,0.0128384660142501,
0.0090768309442104));
#26995=CARTESIAN_POINT('Ctrl Pts',(-0.22679189054867,0.0128384094937561,
0.00907715669066179));
#26996=CARTESIAN_POINT('Ctrl Pts',(-0.226816385267581,0.0128382667923632,
0.0090777409235453));
#26997=CARTESIAN_POINT('Ctrl Pts',(-0.226836329931151,0.0128380537045685,
0.00907828807316758));
#26998=CARTESIAN_POINT('Ctrl Pts',(-0.226876219258291,0.012837627528979,
0.00907938237241213));
#26999=CARTESIAN_POINT('Ctrl Pts',(-0.226897908364983,0.0128369197715561,
0.00908032829070822));
#27000=CARTESIAN_POINT('Ctrl Pts',(-0.22692393469492,0.0128360815957886,
0.0090814550142499));
#27001=CARTESIAN_POINT('Ctrl Pts',(-0.226975767174773,0.0128344123351328,
0.00908369892937038));
#27002=CARTESIAN_POINT('Ctrl Pts',(-0.227044802088362,0.0128322258406691,
0.00908665997123993));
#27003=CARTESIAN_POINT('Ctrl Pts',(-0.227098361224566,0.0128303951409884,
0.009089055605006));
#27004=CARTESIAN_POINT('',(-0.226520627876972,0.0132597435786184,0.00874175742880956));
#27005=CARTESIAN_POINT('Origin',(-0.22782078097521,0.00719470725115772,
0.00186149853466998));
#27006=CARTESIAN_POINT('',(-0.225316581766883,0.0132616346613913,0.00871757524912672));
#27007=CARTESIAN_POINT('',(-0.225316581766768,0.0132616346615032,0.00871757524903155));
#27008=CARTESIAN_POINT('',(-0.225201030506077,0.0128404758197692,0.0090447303940509));
#27009=CARTESIAN_POINT('Ctrl Pts',(-0.225201032785958,0.0128403937127591,
0.00904461617914099));
#27010=CARTESIAN_POINT('Ctrl Pts',(-0.22520217034852,0.0128447365367898,
0.00904144666023971));
#27011=CARTESIAN_POINT('Ctrl Pts',(-0.225206434504416,0.0128611961113402,
0.0090295544399252));
#27012=CARTESIAN_POINT('Ctrl Pts',(-0.22521694138661,0.0129006228490507,
0.00900027455390401));
#27013=CARTESIAN_POINT('Ctrl Pts',(-0.225227448268805,0.0129400495867611,
0.00897099466788282));
#27014=CARTESIAN_POINT('Ctrl Pts',(-0.225244204353462,0.0130022087793867,
0.00892400624483967));
#27015=CARTESIAN_POINT('Ctrl Pts',(-0.225258275192642,0.0130535473699845,
0.00888414630624995));
#27016=CARTESIAN_POINT('Ctrl Pts',(-0.225286416871002,0.01315622455118,
0.00880442642907052));
#27017=CARTESIAN_POINT('Ctrl Pts',(-0.225303791572998,0.0132167305635967,
0.00875462170239737));
#27018=CARTESIAN_POINT('Ctrl Pts',(-0.225316581929261,0.0132616274666869,
0.00871756658863472));
#27019=CARTESIAN_POINT('',(-0.224881672895038,0.0128394796279708,0.00903918282123092));
#27020=CARTESIAN_POINT('Ctrl Pts',(-0.224881672895038,0.0128394796279708,
0.00903918282123092));
#27021=CARTESIAN_POINT('Ctrl Pts',(-0.224944627892334,0.0128441999448473,
0.00903717439391197));
#27022=CARTESIAN_POINT('Ctrl Pts',(-0.225017590937262,0.0128449489007721,
0.00903629354585952));
#27023=CARTESIAN_POINT('Ctrl Pts',(-0.225078012179456,0.0128448149334077,
0.00903805276342249));
#27024=CARTESIAN_POINT('Ctrl Pts',(-0.225141875911401,0.012844673333276,
0.00903991221209972));
#27025=CARTESIAN_POINT('Ctrl Pts',(-0.225191718539843,0.0128427372415438,
0.00904291489718588));
#27026=CARTESIAN_POINT('Ctrl Pts',(-0.225201030475969,0.012840475865135,
0.00904473036080076));
#27027=CARTESIAN_POINT('',(-0.224871009513959,0.0128386119989575,0.00903955781216604));
#27028=CARTESIAN_POINT('Ctrl Pts',(-0.224871010004322,0.0128386125214796,
0.00903955742812217));
#27029=CARTESIAN_POINT('Ctrl Pts',(-0.22487452792311,0.0128389089493161,
0.00903943484621595));
#27030=CARTESIAN_POINT('Ctrl Pts',(-0.224878082488328,0.0128391918532535,
0.00903931570475177));
#27031=CARTESIAN_POINT('Ctrl Pts',(-0.224881672895038,0.0128394796279708,
0.00903918282123092));
#27032=CARTESIAN_POINT('',(-0.225012478343874,0.0119747516700286,0.00960390763878028));
#27033=CARTESIAN_POINT('Ctrl Pts',(-0.225012478352987,0.0119747517006528,
0.00960390762144819));
#27034=CARTESIAN_POINT('Ctrl Pts',(-0.225008710410711,0.012026996045218,
0.00957394039744444));
#27035=CARTESIAN_POINT('Ctrl Pts',(-0.225003438296681,0.0121091891020792,
0.00952597246849311));
#27036=CARTESIAN_POINT('Ctrl Pts',(-0.224994337261927,0.0121985784692992,
0.00947118760888405));
#27037=CARTESIAN_POINT('Ctrl Pts',(-0.22498978674455,0.0122432731529092,
0.00944379517907952));
#27038=CARTESIAN_POINT('Ctrl Pts',(-0.224984279372702,0.0122897558812711,
0.00941468016211316));
#27039=CARTESIAN_POINT('Ctrl Pts',(-0.224979096609221,0.0123276290221422,
0.00939056260385441));
#27040=CARTESIAN_POINT('Ctrl Pts',(-0.22497391384574,0.0123655021630133,
0.00936644504559567));
#27041=CARTESIAN_POINT('Ctrl Pts',(-0.22496905423407,0.0123948120512672,
0.00934739710168434));
#27042=CARTESIAN_POINT('Ctrl Pts',(-0.224965124481069,0.0124175278812019,
0.00933253807523926));
#27043=CARTESIAN_POINT('Ctrl Pts',(-0.224963159604568,0.0124288857961693,
0.00932510856201672));
#27044=CARTESIAN_POINT('Ctrl Pts',(-0.224961426927155,0.0124386035824382,
0.00931873941704309));
#27045=CARTESIAN_POINT('Ctrl Pts',(-0.224958010632985,0.0124564837209923,
0.00930690636953302));
#27046=CARTESIAN_POINT('Ctrl Pts',(-0.224954594338815,0.0124743638595464,
0.00929507332202296));
#27047=CARTESIAN_POINT('Ctrl Pts',(-0.224949495350036,0.012500376081017,
0.00927773042191478));
#27048=CARTESIAN_POINT('Ctrl Pts',(-0.224944426555004,0.0125247400917709,
0.00926128172483698));
#27049=CARTESIAN_POINT('Ctrl Pts',(-0.224939357759971,0.0125491041025248,
0.00924483302775918));
#27050=CARTESIAN_POINT('Ctrl Pts',(-0.224934318807232,0.0125718321678423,
0.00922929625790112));
#27051=CARTESIAN_POINT('Ctrl Pts',(-0.224930551299764,0.0125885920455888,
0.00921776851748214));
#27052=CARTESIAN_POINT('Ctrl Pts',(-0.224926783792295,0.0126053519233354,
0.00920624077706316));
#27053=CARTESIAN_POINT('Ctrl Pts',(-0.224924287175663,0.0126161623503046,
0.0091987498488507));
#27054=CARTESIAN_POINT('Ctrl Pts',(-0.224920930364144,0.0126305427729762,
0.00918873779061256));
#27055=CARTESIAN_POINT('Ctrl Pts',(-0.224914216741104,0.0126593036183194,
0.00916871367413629));
#27056=CARTESIAN_POINT('Ctrl Pts',(-0.224904065469932,0.0127022359337238,
0.00913844733481451));
#27057=CARTESIAN_POINT('Ctrl Pts',(-0.22489519761297,0.0127391097573549,
0.00911196635423408));
#27058=CARTESIAN_POINT('Ctrl Pts',(-0.224886329756008,0.012775983580986,
0.00908548537365366));
#27059=CARTESIAN_POINT('Ctrl Pts',(-0.224878742772621,0.0128068919285356,
0.00906291918311226));
#27060=CARTESIAN_POINT('Ctrl Pts',(-0.224871008983143,0.0128385761256605,
0.00903951085797481));
#27061=CARTESIAN_POINT('',(-0.224873054781352,0.0104158620395419,0.0103054854710163));
#27062=CARTESIAN_POINT('Ctrl Pts',(-0.225012478343874,0.0119747516700286,
0.00960390763878028));
#27063=CARTESIAN_POINT('Ctrl Pts',(-0.224987330133709,0.01182206617983,
0.00969074071080671));
#27064=CARTESIAN_POINT('Ctrl Pts',(-0.224965351168803,0.0116608808019534,
0.0097767691902134));
#27065=CARTESIAN_POINT('Ctrl Pts',(-0.224946345313378,0.0114844605087868,
0.00986337078472748));
#27066=CARTESIAN_POINT('Ctrl Pts',(-0.224927339457954,0.0113080402156202,
0.00994997237924156));
#27067=CARTESIAN_POINT('Ctrl Pts',(-0.224911318282184,0.0111160804773605,
0.0100365919910695));
#27068=CARTESIAN_POINT('Ctrl Pts',(-0.224898835482878,0.0109277687496176,
0.0101137329254911));
#27069=CARTESIAN_POINT('Ctrl Pts',(-0.224896811901168,0.0108972416091349,
0.0101262382121786));
#27070=CARTESIAN_POINT('Ctrl Pts',(-0.224894880873611,0.0108668147692598,
0.0101385061520976));
#27071=CARTESIAN_POINT('Ctrl Pts',(-0.224893040837449,0.0108364759539614,
0.0101505475595201));
#27072=CARTESIAN_POINT('Ctrl Pts',(-0.224884447118257,0.0106947813152176,
0.0102067858423248));
#27073=CARTESIAN_POINT('Ctrl Pts',(-0.22487783816785,0.0105550780358821,
0.0102582455724961));
#27074=CARTESIAN_POINT('Ctrl Pts',(-0.224873054781352,0.0104158620395419,
0.0103054854710163));
#27075=CARTESIAN_POINT('',(-0.224989656143797,0.00749503048378924,0.010792595233899));
#27076=CARTESIAN_POINT('Ctrl Pts',(-0.224873054781352,0.0104158620395419,
0.0103054854710163));
#27077=CARTESIAN_POINT('Ctrl Pts',(-0.224866226582386,0.0102173021707029,
0.0103733294134915));
#27078=CARTESIAN_POINT('Ctrl Pts',(-0.224863118344788,0.0100198072651585,
0.0104327497771305));
#27079=CARTESIAN_POINT('Ctrl Pts',(-0.22486326697531,0.00981927358101678,
0.0104860316796021));
#27080=CARTESIAN_POINT('Ctrl Pts',(-0.224863404497809,0.00963372694671159,
0.0105353315152647));
#27081=CARTESIAN_POINT('Ctrl Pts',(-0.22486633844048,0.00944551647501257,
0.0105790610493068));
#27082=CARTESIAN_POINT('Ctrl Pts',(-0.224872215239344,0.00925595755421325,
0.0106168125946656));
#27083=CARTESIAN_POINT('Ctrl Pts',(-0.224875153638775,0.00916117809381357,
0.010635688367345));
#27084=CARTESIAN_POINT('Ctrl Pts',(-0.224878825962802,0.00906607960841182,
0.0106531498380664));
#27085=CARTESIAN_POINT('Ctrl Pts',(-0.224883681329671,0.00896377930534679,
0.0106701043545088));
#27086=CARTESIAN_POINT('Ctrl Pts',(-0.224888536696539,0.00886147900228176,
0.0106870588709513));
#27087=CARTESIAN_POINT('Ctrl Pts',(-0.224894584175122,0.00875190532334013,
0.0107031016457275));
#27088=CARTESIAN_POINT('Ctrl Pts',(-0.224899808725538,0.00866487696745784,
0.0107145869666058));
#27089=CARTESIAN_POINT('Ctrl Pts',(-0.224905033275954,0.00857784861157555,
0.0107260722874841));
#27090=CARTESIAN_POINT('Ctrl Pts',(-0.224909420529746,0.00851344741040241,
0.010733638861035));
#27091=CARTESIAN_POINT('Ctrl Pts',(-0.224915038388532,0.00843441925484294,
0.0107420341088461));
#27092=CARTESIAN_POINT('Ctrl Pts',(-0.224920656247317,0.00835539109928347,
0.0107504293566573));
#27093=CARTESIAN_POINT('Ctrl Pts',(-0.22492751354538,0.00826169799655761,
0.0107592614034678));
#27094=CARTESIAN_POINT('Ctrl Pts',(-0.224935089512573,0.00816264216894523,
0.0107667780599388));
#27095=CARTESIAN_POINT('Ctrl Pts',(-0.22495024144696,0.00796453051372045,
0.0107818113728808));
#27096=CARTESIAN_POINT('Ctrl Pts',(-0.224968252959357,0.0077449941022938,
0.0107922510362213));
#27097=CARTESIAN_POINT('Ctrl Pts',(-0.224989656143797,0.00749503048378924,
0.010792595233899));
#27098=CARTESIAN_POINT('',(-0.224876132721504,0.00588096715315318,0.010642983684972));
#27099=CARTESIAN_POINT('Ctrl Pts',(-0.224989611770161,0.00749451541494347,
0.0107925939286014));
#27100=CARTESIAN_POINT('Ctrl Pts',(-0.224967889525284,0.00724236729651667,
0.0107919481648337));
#27101=CARTESIAN_POINT('Ctrl Pts',(-0.224949602833122,0.00702085004378462,
0.0107810653131202));
#27102=CARTESIAN_POINT('Ctrl Pts',(-0.224934211963363,0.00682092613373424,
0.0107655246226512));
#27103=CARTESIAN_POINT('Ctrl Pts',(-0.224926511289036,0.00672089611947813,
0.0107577489869667));
#27104=CARTESIAN_POINT('Ctrl Pts',(-0.224919539392079,0.00662627872449041,
0.0107486376236482));
#27105=CARTESIAN_POINT('Ctrl Pts',(-0.224913825599119,0.00654643123053275,
0.0107399825657948));
#27106=CARTESIAN_POINT('Ctrl Pts',(-0.224908111806159,0.0064665837365751,
0.0107313275079415));
#27107=CARTESIAN_POINT('Ctrl Pts',(-0.224903647137783,0.00640146658868505,
0.0107235271217113));
#27108=CARTESIAN_POINT('Ctrl Pts',(-0.224898329718857,0.00631360222420139,
0.0107117163940124));
#27109=CARTESIAN_POINT('Ctrl Pts',(-0.224893012299931,0.00622573785971773,
0.0106999056663135));
#27110=CARTESIAN_POINT('Ctrl Pts',(-0.224886856690796,0.0061152112912604,
0.0106834372017356));
#27111=CARTESIAN_POINT('Ctrl Pts',(-0.224881918316017,0.00601190187579096,
0.0106660263533176));
#27112=CARTESIAN_POINT('Ctrl Pts',(-0.224879775998716,0.00596708519864215,
0.0106584733498581));
#27113=CARTESIAN_POINT('Ctrl Pts',(-0.224877861054523,0.00592361449883146,
0.0106508077009257));
#27114=CARTESIAN_POINT('Ctrl Pts',(-0.224876132721504,0.00588096715315318,
0.010642983684972));
#27115=CARTESIAN_POINT('',(-0.224076522719914,0.00588277614622394,0.010625353510046));
#27116=CARTESIAN_POINT('Ctrl Pts',(-0.224876132721504,0.00588096715315317,
0.010642983684972));
#27117=CARTESIAN_POINT('Ctrl Pts',(-0.224076521518844,0.00588276506383911,
0.0106254138449689));
#27118=CARTESIAN_POINT('',(-0.224190648122848,0.00749528770010443,0.0107745370286281));
#27119=CARTESIAN_POINT('Ctrl Pts',(-0.224076522719914,0.00588277614622425,
0.010625353510046));
#27120=CARTESIAN_POINT('Ctrl Pts',(-0.224077151983702,0.00589828271375071,
0.0106282142999538));
#27121=CARTESIAN_POINT('Ctrl Pts',(-0.224082955020581,0.00603662211173329,
0.0106533554983067));
#27122=CARTESIAN_POINT('Ctrl Pts',(-0.224093480360963,0.0062288683222389,
0.0106833518343927));
#27123=CARTESIAN_POINT('Ctrl Pts',(-0.224110291260917,0.00649044232002643,
0.0107167590851501));
#27124=CARTESIAN_POINT('Ctrl Pts',(-0.224127481546521,0.00672803320751328,
0.0107404347775083));
#27125=CARTESIAN_POINT('Ctrl Pts',(-0.224137535386306,0.00685693381374031,
0.0107505870267272));
#27126=CARTESIAN_POINT('Ctrl Pts',(-0.224157907843775,0.00711079347145578,
0.0107671148153925));
#27127=CARTESIAN_POINT('Ctrl Pts',(-0.224176389710925,0.0073296949891921,
0.0107741272895942));
#27128=CARTESIAN_POINT('Ctrl Pts',(-0.224190649380928,0.00749528605098617,
0.0107745371458377));
#27129=CARTESIAN_POINT('',(-0.224080534199978,0.0105762623394819,0.0102317974583992));
#27130=CARTESIAN_POINT('Ctrl Pts',(-0.224190649231643,0.00749528779516735,
0.010774537143386));
#27131=CARTESIAN_POINT('Ctrl Pts',(-0.224176496049103,0.00766064698633964,
0.0107743046922629));
#27132=CARTESIAN_POINT('Ctrl Pts',(-0.224158158806334,0.00787923373782332,
0.0107675433910972));
#27133=CARTESIAN_POINT('Ctrl Pts',(-0.224137967011069,0.00813268605449651,
0.0107513356813969));
#27134=CARTESIAN_POINT('Ctrl Pts',(-0.224128006599897,0.00826137903423121,
0.0107413516624803));
#27135=CARTESIAN_POINT('Ctrl Pts',(-0.224111011590131,0.00849848535023519,
0.0107180136087507));
#27136=CARTESIAN_POINT('Ctrl Pts',(-0.224094433786784,0.00875959453805924,
0.0106850105184737));
#27137=CARTESIAN_POINT('Ctrl Pts',(-0.224072162870967,0.00917370885433421,
0.0106208996991876));
#27138=CARTESIAN_POINT('Ctrl Pts',(-0.224058304186119,0.00982143528436496,
0.0104791570008723));
#27139=CARTESIAN_POINT('Ctrl Pts',(-0.224068970775361,0.0103174374881225,
0.0103260156650735));
#27140=CARTESIAN_POINT('Ctrl Pts',(-0.224080534199978,0.0105762623394819,
0.0102317974583992));
#27141=CARTESIAN_POINT('',(-0.224520408689827,0.0132627824003338,0.00870166862344196));
#27142=CARTESIAN_POINT('Ctrl Pts',(-0.224080566034144,0.0105769745611062,
0.0102315381587443));
#27143=CARTESIAN_POINT('Ctrl Pts',(-0.224092151509287,0.0108360569066869,
0.0101372010598917));
#27144=CARTESIAN_POINT('Ctrl Pts',(-0.224118896843735,0.0112411393783209,
0.00996911208968928));
#27145=CARTESIAN_POINT('Ctrl Pts',(-0.224170735895982,0.0116930385087458,
0.0097434105075323));
#27146=CARTESIAN_POINT('Ctrl Pts',(-0.224215922342647,0.0119969042554561,
0.00957749590305291));
#27147=CARTESIAN_POINT('Ctrl Pts',(-0.224266689003916,0.0122607174895522,
0.00941974624796191));
#27148=CARTESIAN_POINT('Ctrl Pts',(-0.224313605564443,0.01247477238858,
0.00928306617490918));
#27149=CARTESIAN_POINT('Ctrl Pts',(-0.224360095211767,0.012667384538008,
0.00915273873550236));
#27150=CARTESIAN_POINT('Ctrl Pts',(-0.224383610132216,0.0127587835173505,
0.00908822365193216));
#27151=CARTESIAN_POINT('Ctrl Pts',(-0.224435627652213,0.0129574442013583,
0.00894448849032735));
#27152=CARTESIAN_POINT('Ctrl Pts',(-0.224483462100191,0.013131275288331,
0.00881005173864322));
#27153=CARTESIAN_POINT('Ctrl Pts',(-0.224520870146751,0.0132627197125121,
0.00870173325440467));
#27154=CARTESIAN_POINT('',(-0.22331682546513,0.0132649854369558,0.00867730801686743));
#27155=CARTESIAN_POINT('',(-0.223316825297034,0.0132649928747286,0.00867731700379056));
#27156=CARTESIAN_POINT('',(-0.222880616837559,0.010577337791327,0.0102052819769689));
#27157=CARTESIAN_POINT('Ctrl Pts',(-0.22331682546513,0.0132649854369558,
0.00867730801686743));
#27158=CARTESIAN_POINT('Ctrl Pts',(-0.223279798803615,0.0131348061383841,
0.00878434512588197));
#27159=CARTESIAN_POINT('Ctrl Pts',(-0.223232266045539,0.0129617921433397,
0.00891797582610665));
#27160=CARTESIAN_POINT('Ctrl Pts',(-0.223180368331416,0.0127626377797213,
0.0090618860882604));
#27161=CARTESIAN_POINT('Ctrl Pts',(-0.223156255037636,0.0126681475127752,
0.00912843001754567));
#27162=CARTESIAN_POINT('Ctrl Pts',(-0.223110670361712,0.0124772678792337,
0.00925731159444108));
#27163=CARTESIAN_POINT('Ctrl Pts',(-0.223064300581422,0.0122631114605902,
0.00939386631131441));
#27164=CARTESIAN_POINT('Ctrl Pts',(-0.22301407297073,0.0119976000119375,
0.0095523407640007));
#27165=CARTESIAN_POINT('Ctrl Pts',(-0.222969614485712,0.0116931713173529,
0.0097182094358203));
#27166=CARTESIAN_POINT('Ctrl Pts',(-0.222918481738802,0.0112405948889791,
0.00994374743151154));
#27167=CARTESIAN_POINT('Ctrl Pts',(-0.222892075429266,0.0108362091582251,
0.0101112031578736));
#27168=CARTESIAN_POINT('Ctrl Pts',(-0.222880616837559,0.010577337791327,
0.0102052819769689));
#27169=CARTESIAN_POINT('',(-0.222990244465972,0.0074958307571125,0.0107474072527987));
#27170=CARTESIAN_POINT('Ctrl Pts',(-0.222880616837559,0.010577337791327,
0.0102052819769689));
#27171=CARTESIAN_POINT('Ctrl Pts',(-0.222869158245852,0.010318466424429,
0.0102993607960641));
#27172=CARTESIAN_POINT('Ctrl Pts',(-0.222858532291739,0.0098221619311753,
0.0104524017706292));
#27173=CARTESIAN_POINT('Ctrl Pts',(-0.22287221561341,0.00917417190932849,
0.01059395889742));
#27174=CARTESIAN_POINT('Ctrl Pts',(-0.22289427636194,0.00876014094051484,
0.010657968090584));
#27175=CARTESIAN_POINT('Ctrl Pts',(-0.222910764672285,0.00849894378348925,
0.010690932418882));
#27176=CARTESIAN_POINT('Ctrl Pts',(-0.222927658039428,0.00826210241293319,
0.0107142206595775));
#27177=CARTESIAN_POINT('Ctrl Pts',(-0.222937661815565,0.00813238625044321,
0.0107242728838261));
#27178=CARTESIAN_POINT('Ctrl Pts',(-0.222957828125963,0.00787876829528368,
0.0107404453241587));
#27179=CARTESIAN_POINT('Ctrl Pts',(-0.222976130338379,0.00766059007085584,
0.0107471651883034));
#27180=CARTESIAN_POINT('Ctrl Pts',(-0.222990244465972,0.0074958307571125,
0.0107474072527987));
#27181=CARTESIAN_POINT('',(-0.222876594854072,0.00588547347265839,0.0105989910637735));
#27182=CARTESIAN_POINT('Ctrl Pts',(-0.222990239545162,0.00749577366117287,
0.0107474071147549));
#27183=CARTESIAN_POINT('Ctrl Pts',(-0.22297603597005,0.00733096986388736,
0.0107470081671261));
#27184=CARTESIAN_POINT('Ctrl Pts',(-0.222957600580606,0.00711260011738536,
0.0107400754574236));
#27185=CARTESIAN_POINT('Ctrl Pts',(-0.222937252471541,0.00685858184257114,
0.0107236246276555));
#27186=CARTESIAN_POINT('Ctrl Pts',(-0.22292712606046,0.00672831097961292,
0.0107133900195418));
#27187=CARTESIAN_POINT('Ctrl Pts',(-0.222910059900934,0.00649137236979646,
0.010689833478941));
#27188=CARTESIAN_POINT('Ctrl Pts',(-0.22289333691819,0.00622976706583754,
0.0106565195733224));
#27189=CARTESIAN_POINT('Ctrl Pts',(-0.222882927058416,0.00603800133094661,
0.0106266668100976));
#27190=CARTESIAN_POINT('Ctrl Pts',(-0.222877192716254,0.00590029280163884,
0.0106017151325738));
#27191=CARTESIAN_POINT('Ctrl Pts',(-0.222876594854072,0.00588547347265862,
0.0105989910637735));
#27192=CARTESIAN_POINT('',(-0.222077231673906,0.00588727068028757,0.0105814273450435));
#27193=CARTESIAN_POINT('Ctrl Pts',(-0.222876593582855,0.00588546307913867,
0.0105990478538717));
#27194=CARTESIAN_POINT('Ctrl Pts',(-0.22207723054939,0.00588726043182086,
0.0105814834668851));
#27195=CARTESIAN_POINT('',(-0.222191219837884,0.00749641675969908,0.0107293488757352));
#27196=CARTESIAN_POINT('Ctrl Pts',(-0.222077231673906,0.00588727068028781,
0.0105814273450436));
#27197=CARTESIAN_POINT('Ctrl Pts',(-0.222077817443984,0.00590163889072924,
0.010584062875708));
#27198=CARTESIAN_POINT('Ctrl Pts',(-0.222083585840763,0.00603885906659558,
0.0106088832961562));
#27199=CARTESIAN_POINT('Ctrl Pts',(-0.22209405093591,0.00622999833890161,
0.010638590169762));
#27200=CARTESIAN_POINT('Ctrl Pts',(-0.222110861395534,0.00649158239727542,
0.0106718672026456));
#27201=CARTESIAN_POINT('Ctrl Pts',(-0.22212805244651,0.00672918335429661,
0.0106954431976079));
#27202=CARTESIAN_POINT('Ctrl Pts',(-0.22213810188887,0.00685802378461892,
0.0107055446600767));
#27203=CARTESIAN_POINT('Ctrl Pts',(-0.222158473656955,0.0071118708222244,
0.0107219929296602));
#27204=CARTESIAN_POINT('Ctrl Pts',(-0.222176957436455,0.00733079304772627,
0.0107289601534279));
#27205=CARTESIAN_POINT('Ctrl Pts',(-0.222191219837884,0.00749641675969908,
0.0107293488757352));
#27206=CARTESIAN_POINT('',(-0.222081197665177,0.0105780449623156,0.0101876296223523));
#27207=CARTESIAN_POINT('Ctrl Pts',(-0.222191219671532,0.00749641870290202,
0.0107293488727541));
#27208=CARTESIAN_POINT('Ctrl Pts',(-0.222177058733032,0.00766183514344189,
0.0107290950868428));
#27209=CARTESIAN_POINT('Ctrl Pts',(-0.222158713562285,0.00788046962613566,
0.0107223213320887));
#27210=CARTESIAN_POINT('Ctrl Pts',(-0.22213851683349,0.00813393428353906,
0.0107061245783974));
#27211=CARTESIAN_POINT('Ctrl Pts',(-0.222128559102259,0.00826256686459831,
0.0106961574222194));
#27212=CARTESIAN_POINT('Ctrl Pts',(-0.222111558904582,0.00849971984722734,
0.0106728517706667));
#27213=CARTESIAN_POINT('Ctrl Pts',(-0.222094980050245,0.00876085477560986,
0.0106399064973814));
#27214=CARTESIAN_POINT('Ctrl Pts',(-0.222072711961566,0.00917502974014479,
0.0105759159488009));
#27215=CARTESIAN_POINT('Ctrl Pts',(-0.222058878162029,0.00982287571753665,
0.0104344849162957));
#27216=CARTESIAN_POINT('Ctrl Pts',(-0.222069605421447,0.0103192093797939,
0.0102815997590037));
#27217=CARTESIAN_POINT('Ctrl Pts',(-0.222081197665177,0.0105780449623156,
0.0101876296223523));
#27218=CARTESIAN_POINT('',(-0.222521351578035,0.0132670948112432,0.00866068980045947));
#27219=CARTESIAN_POINT('Ctrl Pts',(-0.222081228766005,0.0105787390845834,
0.0101873775888729));
#27220=CARTESIAN_POINT('Ctrl Pts',(-0.222092842521717,0.0108378253339584,
0.0100932920251452));
#27221=CARTESIAN_POINT('Ctrl Pts',(-0.222119627444957,0.011242674877814,
0.00992576375075805));
#27222=CARTESIAN_POINT('Ctrl Pts',(-0.222171526065299,0.0116950336032214,
0.00970054580926344));
#27223=CARTESIAN_POINT('Ctrl Pts',(-0.222216807058984,0.0119996304538849,
0.00953473789079934));
#27224=CARTESIAN_POINT('Ctrl Pts',(-0.222267519311081,0.0122635513148824,
0.00937741358971341));
#27225=CARTESIAN_POINT('Ctrl Pts',(-0.22231438826496,0.0124778714741315,
0.00924100644392873));
#27226=CARTESIAN_POINT('Ctrl Pts',(-0.222360817077006,0.012670745258053,
0.00911092961363663));
#27227=CARTESIAN_POINT('Ctrl Pts',(-0.222384295531511,0.0127622736095719,
0.0090465381747067));
#27228=CARTESIAN_POINT('Ctrl Pts',(-0.222436236646195,0.0129612471208603,
0.00890306004810599));
#27229=CARTESIAN_POINT('Ctrl Pts',(-0.222483998152326,0.0131353820046699,
0.00876885123967379));
#27230=CARTESIAN_POINT('Ctrl Pts',(-0.222521353943371,0.0132670959637705,
0.00866069202955122));
#27231=CARTESIAN_POINT('',(-0.22131750689037,0.0132679777242635,0.00863749771222783));
#27232=CARTESIAN_POINT('',(-0.221317506737634,0.013267984478113,0.00863750590557259));
#27233=CARTESIAN_POINT('',(-0.22088115156098,0.0105783645468105,0.010161402673548));
#27234=CARTESIAN_POINT('Ctrl Pts',(-0.22131750689037,0.0132679777242635,
0.00863749771222783));
#27235=CARTESIAN_POINT('Ctrl Pts',(-0.221280596683195,0.0131376209513906,
0.00874425583075433));
#27236=CARTESIAN_POINT('Ctrl Pts',(-0.221233204347556,0.0129643814873638,
0.008877547080368));
#27237=CARTESIAN_POINT('Ctrl Pts',(-0.221181438272831,0.0127649663026909,
0.00902110773845264));
#27238=CARTESIAN_POINT('Ctrl Pts',(-0.221157370058087,0.0126703006863166,
0.00908752698191699));
#27239=CARTESIAN_POINT('Ctrl Pts',(-0.221111880231701,0.0124792324471473,
0.00921606458370327));
#27240=CARTESIAN_POINT('Ctrl Pts',(-0.221065554909024,0.0122648142583938,
0.00935229104230504));
#27241=CARTESIAN_POINT('Ctrl Pts',(-0.221015368911087,0.011999454456574,
0.0095101388491494));
#27242=CARTESIAN_POINT('Ctrl Pts',(-0.220970544862955,0.0116933253634984,
0.00967635688216004));
#27243=CARTESIAN_POINT('Ctrl Pts',(-0.220919169872804,0.0112401297049436,
0.00990131927234546));
#27244=CARTESIAN_POINT('Ctrl Pts',(-0.220892657893147,0.0108367113854765,
0.0100677899435825));
#27245=CARTESIAN_POINT('Ctrl Pts',(-0.22088115156098,0.0105783645468105,
0.010161402673548));
#27246=CARTESIAN_POINT('',(-0.220990767119986,0.00749707322251576,0.010702217868989));
#27247=CARTESIAN_POINT('Ctrl Pts',(-0.22088115156098,0.0105783645468105,
0.010161402673548));
#27248=CARTESIAN_POINT('Ctrl Pts',(-0.220869645228813,0.0103200177081445,
0.0102550154035136));
#27249=CARTESIAN_POINT('Ctrl Pts',(-0.220858969206354,0.00982452144610325,
0.0104075054283932));
#27250=CARTESIAN_POINT('Ctrl Pts',(-0.220872745540538,0.00917495312743478,
0.0105490903500837));
#27251=CARTESIAN_POINT('Ctrl Pts',(-0.220894819848736,0.00876114659657297,
0.010612900546867));
#27252=CARTESIAN_POINT('Ctrl Pts',(-0.220911311157844,0.00849998081158383,
0.0106457941366486));
#27253=CARTESIAN_POINT('Ctrl Pts',(-0.220928202324832,0.00826319748824002,
0.0106690348315061));
#27254=CARTESIAN_POINT('Ctrl Pts',(-0.220938201788269,0.00813353165458825,
0.0106790696234058));
#27255=CARTESIAN_POINT('Ctrl Pts',(-0.22095836166011,0.00787996925633426,
0.0106952234487667));
#27256=CARTESIAN_POINT('Ctrl Pts',(-0.220976657670658,0.00766182000071475,
0.0107019528152277));
#27257=CARTESIAN_POINT('Ctrl Pts',(-0.220990767119986,0.00749707322251576,
0.010702217868989));
#27258=CARTESIAN_POINT('',(-0.220877304433504,0.00588996792097283,0.0105550654063144));
#27259=CARTESIAN_POINT('Ctrl Pts',(-0.220990762709943,0.00749702203711106,
0.0107022177524562));
#27260=CARTESIAN_POINT('Ctrl Pts',(-0.220976559819124,0.00733217508802056,
0.0107018420080365));
#27261=CARTESIAN_POINT('Ctrl Pts',(-0.22095812756767,0.00711377483183485,
0.0106949566930038));
#27262=CARTESIAN_POINT('Ctrl Pts',(-0.220937786972359,0.00685976194883156,
0.0106785878913699));
#27263=CARTESIAN_POINT('Ctrl Pts',(-0.220927669297289,0.00672955702063277,
0.0106684068115));
#27264=CARTESIAN_POINT('Ctrl Pts',(-0.220910609290499,0.00649259338853425,
0.0106449511936309));
#27265=CARTESIAN_POINT('Ctrl Pts',(-0.220893896329436,0.00623097711339245,
0.0106117714895317));
#27266=CARTESIAN_POINT('Ctrl Pts',(-0.220883552434346,0.0060402582927849,
0.0105821976385212));
#27267=CARTESIAN_POINT('Ctrl Pts',(-0.220877859202795,0.00590367268940595,
0.0105575697530104));
#27268=CARTESIAN_POINT('Ctrl Pts',(-0.220877304433504,0.005889967920973,
0.0105550654063144));
#27269=CARTESIAN_POINT('',(-0.220077799936617,0.00589176565002758,0.0105374974776579));
#27270=CARTESIAN_POINT('Ctrl Pts',(-0.220877303267762,0.00588995844564909,
0.0105551174901662));
#27271=CARTESIAN_POINT('Ctrl Pts',(-0.220077798878423,0.0058917561161673,
0.0105375499971699));
#27272=CARTESIAN_POINT('',(-0.220191750495462,0.00749752817580766,0.0106841595550818));
#27273=CARTESIAN_POINT('Ctrl Pts',(-0.220077799936617,0.00589176565002776,
0.0105374974776579));
#27274=CARTESIAN_POINT('Ctrl Pts',(-0.220078351608142,0.00590522124109448,
0.0105399511847801));
#27275=CARTESIAN_POINT('Ctrl Pts',(-0.220084100627504,0.00604148651957028,
0.0105644754757549));
#27276=CARTESIAN_POINT('Ctrl Pts',(-0.220094528895997,0.00623167523773941,
0.010593906086857));
#27277=CARTESIAN_POINT('Ctrl Pts',(-0.220111351815037,0.00649315070770517,
0.0106270223766921));
#27278=CARTESIAN_POINT('Ctrl Pts',(-0.220128554181359,0.00673065566572463,
0.0106504779393937));
#27279=CARTESIAN_POINT('Ctrl Pts',(-0.220138604498337,0.00685937820658921,
0.0106605198785713));
#27280=CARTESIAN_POINT('Ctrl Pts',(-0.220158985618377,0.00711309953252186,
0.0106768746775319));
#27281=CARTESIAN_POINT('Ctrl Pts',(-0.220177479403337,0.00733194518244467,
0.0106837913787835));
#27282=CARTESIAN_POINT('Ctrl Pts',(-0.220191750495462,0.00749752817580766,
0.0106841595550818));
#27283=CARTESIAN_POINT('',(-0.220080922141363,0.0105666342787044,0.0101482127006066));
#27284=CARTESIAN_POINT('Ctrl Pts',(-0.220191750367871,0.00749752966457758,
0.0106841595526083));
#27285=CARTESIAN_POINT('Ctrl Pts',(-0.220177627116492,0.00766232360287522,
0.0106838857496589));
#27286=CARTESIAN_POINT('Ctrl Pts',(-0.22015933208859,0.00788007512162449,
0.0106771540698828));
#27287=CARTESIAN_POINT('Ctrl Pts',(-0.220139190917174,0.00813238879895161,
0.0106611110916827));
#27288=CARTESIAN_POINT('Ctrl Pts',(-0.220129266225352,0.00826033660350853,
0.0106512514860819));
#27289=CARTESIAN_POINT('Ctrl Pts',(-0.220112302357682,0.00849632083744043,
0.0106282022977969));
#27290=CARTESIAN_POINT('Ctrl Pts',(-0.220095725865799,0.00875628513266106,
0.010595617319954));
#27291=CARTESIAN_POINT('Ctrl Pts',(-0.220073367500684,0.00916890990113659,
0.0105322979819828));
#27292=CARTESIAN_POINT('Ctrl Pts',(-0.220059171892308,0.00981497694871467,
0.0103921745952535));
#27293=CARTESIAN_POINT('Ctrl Pts',(-0.220069554539533,0.010308881910491,
0.0102410928523781));
#27294=CARTESIAN_POINT('Ctrl Pts',(-0.220080922141363,0.0105666342787044,
0.0101482127006066));
#27295=CARTESIAN_POINT('',(-0.220516756733524,0.0132502006776825,0.00863716366641789));
#27296=CARTESIAN_POINT('Ctrl Pts',(-0.220080948889328,0.0105672405317447,
0.0101479942146856));
#27297=CARTESIAN_POINT('Ctrl Pts',(-0.220092335098988,0.0108252120871597,
0.0100550139845299));
#27298=CARTESIAN_POINT('Ctrl Pts',(-0.220118697300213,0.0112285596160589,
0.00988944046538119));
#27299=CARTESIAN_POINT('Ctrl Pts',(-0.220169906485688,0.0116799609641777,
0.00966654457709283));
#27300=CARTESIAN_POINT('Ctrl Pts',(-0.220214571302728,0.0119840360542289,
0.00950241318882273));
#27301=CARTESIAN_POINT('Ctrl Pts',(-0.220264797648843,0.0122482886171999,
0.00934622564793901));
#27302=CARTESIAN_POINT('Ctrl Pts',(-0.220311203197558,0.0124622454996215,
0.00921119607442466));
#27303=CARTESIAN_POINT('Ctrl Pts',(-0.220356992400339,0.0126538793364392,
0.0090831156431634));
#27304=CARTESIAN_POINT('Ctrl Pts',(-0.220380703772808,0.012746902376668,
0.00901827556250336));
#27305=CARTESIAN_POINT('Ctrl Pts',(-0.220432380283764,0.0129458253658021,
0.00887609019326517));
#27306=CARTESIAN_POINT('Ctrl Pts',(-0.220479785242708,0.0131192947887207,
0.00874360326452844));
#27307=CARTESIAN_POINT('Ctrl Pts',(-0.22051677874237,0.013250196930254,
0.0086371671501659));
#27308=CARTESIAN_POINT('',(-0.219244233672426,0.0130315029362845,0.00878633472257528));
#27309=CARTESIAN_POINT('Ctrl Pts',(-0.220516438237267,0.0132502507262974,
0.00863711659192548));
#27310=CARTESIAN_POINT('Ctrl Pts',(-0.220480268319726,0.013255974430882,
0.00863175603814082));
#27311=CARTESIAN_POINT('Ctrl Pts',(-0.220444069983548,0.0132619562961405,
0.00862616257509982));
#27312=CARTESIAN_POINT('Ctrl Pts',(-0.220413824310793,0.0132667445129213,
0.0086216573058079));
#27313=CARTESIAN_POINT('Ctrl Pts',(-0.220383483725874,0.0132715477553231,
0.00861713789879583));
#27314=CARTESIAN_POINT('Ctrl Pts',(-0.220367610104368,0.0132739986326908,
0.00861482180772873));
#27315=CARTESIAN_POINT('Ctrl Pts',(-0.220344973659625,0.0132771549469773,
0.00861179794256445));
#27316=CARTESIAN_POINT('Ctrl Pts',(-0.220322337214882,0.0132803112612638,
0.00860877407740017));
#27317=CARTESIAN_POINT('Ctrl Pts',(-0.220292924362422,0.0132839471365864,
0.0086052268546576));
#27318=CARTESIAN_POINT('Ctrl Pts',(-0.220265102204071,0.0132865904342554,
0.0086025299413693));
#27319=CARTESIAN_POINT('Ctrl Pts',(-0.220237280045721,0.0132892337319244,
0.00859983302808099));
#27320=CARTESIAN_POINT('Ctrl Pts',(-0.220211364377883,0.0132908098461735,
0.00859805395339447));
#27321=CARTESIAN_POINT('Ctrl Pts',(-0.220185552309859,0.0132914489697062,
0.00859705519961988));
#27322=CARTESIAN_POINT('Ctrl Pts',(-0.220133928173812,0.0132927272167718,
0.0085950576920707));
#27323=CARTESIAN_POINT('Ctrl Pts',(-0.220082288209308,0.013290467608556,
0.00859600043319445));
#27324=CARTESIAN_POINT('Ctrl Pts',(-0.220025068662385,0.0132840223930742,
0.00860026211803082));
#27325=CARTESIAN_POINT('Ctrl Pts',(-0.219967849115462,0.0132775771775925,
0.0086045238028672));
#27326=CARTESIAN_POINT('Ctrl Pts',(-0.219911157066727,0.0132674150573731,
0.00861182319958806));
#27327=CARTESIAN_POINT('Ctrl Pts',(-0.219858169150949,0.0132553285520544,
0.00862069118620989));
#27328=CARTESIAN_POINT('Ctrl Pts',(-0.219805181235171,0.0132432420467357,
0.00862955917283173));
#27329=CARTESIAN_POINT('Ctrl Pts',(-0.219755810159764,0.0132294672326508,
0.00863980980627492));
#27330=CARTESIAN_POINT('Ctrl Pts',(-0.219703713004701,0.0132129558824833,
0.00865213539350521));
#27331=CARTESIAN_POINT('Ctrl Pts',(-0.219651615849639,0.0131964445323158,
0.00866446098073551));
#27332=CARTESIAN_POINT('Ctrl Pts',(-0.219596945811511,0.0131768246090758,
0.0086791425006151));
#27333=CARTESIAN_POINT('Ctrl Pts',(-0.219551385430325,0.0131593781368699,
0.00869216144093205));
#27334=CARTESIAN_POINT('Ctrl Pts',(-0.219505825049139,0.0131419316646639,
0.008705180381249));
#27335=CARTESIAN_POINT('Ctrl Pts',(-0.219469184677475,0.0131270680608145,
0.00871625684184567));
#27336=CARTESIAN_POINT('Ctrl Pts',(-0.21941888662179,0.0131060788644454,
0.00873177776888143));
#27337=CARTESIAN_POINT('Ctrl Pts',(-0.21936858951329,0.0130850900633333,
0.00874729840363565));
#27338=CARTESIAN_POINT('Ctrl Pts',(-0.219313998061988,0.0130616867100786,
0.00876453744485508));
#27339=CARTESIAN_POINT('Ctrl Pts',(-0.21924423382129,0.0130315026592322,
0.00878633481537574));
#27340=CARTESIAN_POINT('',(-0.218875465344166,0.0104240813886614,0.0101716525593504));
#27341=CARTESIAN_POINT('Ctrl Pts',(-0.219244229875535,0.01303150113094,
0.00878633627788661));
#27342=CARTESIAN_POINT('Ctrl Pts',(-0.219212468167501,0.0129041535974503,
0.00888326996627987));
#27343=CARTESIAN_POINT('Ctrl Pts',(-0.219171618151564,0.0127349113020677,
0.00900461726313376));
#27344=CARTESIAN_POINT('Ctrl Pts',(-0.219126905471443,0.0125395266838569,
0.00913592699872258));
#27345=CARTESIAN_POINT('Ctrl Pts',(-0.219105910134124,0.0124456963448853,
0.00919740664822915));
#27346=CARTESIAN_POINT('Ctrl Pts',(-0.21906680529408,0.0122586484724146,
0.00931499746594284));
#27347=CARTESIAN_POINT('Ctrl Pts',(-0.219027129640222,0.0120491216573116,
0.00943952759860135));
#27348=CARTESIAN_POINT('Ctrl Pts',(-0.218984562930208,0.0117904939538435,
0.00958354134450399));
#27349=CARTESIAN_POINT('Ctrl Pts',(-0.218947335080204,0.0114953276327174,
0.00973376831601864));
#27350=CARTESIAN_POINT('Ctrl Pts',(-0.218905067925516,0.011059173820964,
0.00993691740974779));
#27351=CARTESIAN_POINT('Ctrl Pts',(-0.218884139782213,0.010673657181293,
0.0100865682928677));
#27352=CARTESIAN_POINT('Ctrl Pts',(-0.218875511383952,0.0104254101427982,
0.0101711999131546));
#27353=CARTESIAN_POINT('Ctrl Pts',(-0.218875465344166,0.0104240813886614,
0.0101716525593504));
#27354=CARTESIAN_POINT('',(-0.218991322981713,0.00749805982928716,0.0106570290092488));
#27355=CARTESIAN_POINT('Ctrl Pts',(-0.218875465344166,0.0104240813886614,
0.0101716525593504));
#27356=CARTESIAN_POINT('Ctrl Pts',(-0.218866957649238,0.0101785408296986,
0.0102552970778239));
#27357=CARTESIAN_POINT('Ctrl Pts',(-0.218860390040912,0.00970408442057063,
0.010393046425217));
#27358=CARTESIAN_POINT('Ctrl Pts',(-0.21887667134308,0.00908642942615499,
0.0105199428177679));
#27359=CARTESIAN_POINT('Ctrl Pts',(-0.218898757952546,0.00869434427410445,
0.0105770294824024));
#27360=CARTESIAN_POINT('Ctrl Pts',(-0.218914911213311,0.00844740082145461,
0.0106064119739009));
#27361=CARTESIAN_POINT('Ctrl Pts',(-0.218931211986323,0.00822432582340474,
0.0106271363044335));
#27362=CARTESIAN_POINT('Ctrl Pts',(-0.218940889961919,0.00810101478696289,
0.0106361869864059));
#27363=CARTESIAN_POINT('Ctrl Pts',(-0.218960284069682,0.00786083539543083,
0.0106506878405709));
#27364=CARTESIAN_POINT('Ctrl Pts',(-0.2189778221636,0.00765412001126297,
0.0106567575785991));
#27365=CARTESIAN_POINT('Ctrl Pts',(-0.218991322981713,0.00749805982928716,
0.0106570290092488));
#27366=CARTESIAN_POINT('',(-0.218877735683465,0.00589448248302666,0.0105110260225545));
#27367=CARTESIAN_POINT('Ctrl Pts',(-0.21899132312477,0.00749805817564265,
0.0106570290121248));
#27368=CARTESIAN_POINT('Ctrl Pts',(-0.218977743467873,0.00734187731821718,
0.0106566883481389));
#27369=CARTESIAN_POINT('Ctrl Pts',(-0.218960091281344,0.00713491968854588,
0.0106505193076562));
#27370=CARTESIAN_POINT('Ctrl Pts',(-0.218940535583419,0.00689420098152088,
0.0106358601259392));
#27371=CARTESIAN_POINT('Ctrl Pts',(-0.218930767179068,0.00677056161632596,
0.0106267188712399));
#27372=CARTESIAN_POINT('Ctrl Pts',(-0.218914264768996,0.00654649653511506,
0.010605761807423));
#27373=CARTESIAN_POINT('Ctrl Pts',(-0.218897888368177,0.00629855136156268,
0.0105760736711211));
#27374=CARTESIAN_POINT('Ctrl Pts',(-0.218886088918103,0.00609175956828754,
0.0105457931374041));
#27375=CARTESIAN_POINT('Ctrl Pts',(-0.218879322128981,0.00593446536993965,
0.0105182897355673));
#27376=CARTESIAN_POINT('Ctrl Pts',(-0.218877735683465,0.00589448248302666,
0.0105110260225545));
#27377=CARTESIAN_POINT('',(-0.218078126203157,0.00589629686000176,0.0104933642872807));
#27378=CARTESIAN_POINT('Ctrl Pts',(-0.218877732216029,0.00589445444339055,
0.0105111809578404));
#27379=CARTESIAN_POINT('Ctrl Pts',(-0.2180781221123,0.00589625235160557,
0.0104936111419841));
#27380=CARTESIAN_POINT('',(-0.218192328422137,0.00749852093264668,0.0106389711280447));
#27381=CARTESIAN_POINT('Ctrl Pts',(-0.218078126203157,0.00589629686000176,
0.0104933642872807));
#27382=CARTESIAN_POINT('Ctrl Pts',(-0.218080721583118,0.00596266805916596,
0.0105053741575296));
#27383=CARTESIAN_POINT('Ctrl Pts',(-0.218088632405485,0.00614064320404191,
0.0105356256713857));
#27384=CARTESIAN_POINT('Ctrl Pts',(-0.218101925206918,0.0063619630293138,
0.0105662762574105));
#27385=CARTESIAN_POINT('Ctrl Pts',(-0.218117994796678,0.00659663549417377,
0.0105928968047437));
#27386=CARTESIAN_POINT('Ctrl Pts',(-0.21813409507781,0.00680948317083492,
0.0106117489251953));
#27387=CARTESIAN_POINT('Ctrl Pts',(-0.218143411151013,0.00692497699745548,
0.010619841250455));
#27388=CARTESIAN_POINT('Ctrl Pts',(-0.218162246558742,0.00715281682608959,
0.0106330394232576));
#27389=CARTESIAN_POINT('Ctrl Pts',(-0.218179240829485,0.00734956024527172,
0.0106386506502909));
#27390=CARTESIAN_POINT('Ctrl Pts',(-0.218192327995395,0.0074985079816192,
0.010638971132602));
#27391=CARTESIAN_POINT('',(-0.218168590358226,0.00777884796634574,0.0106341206922536));
#27392=CARTESIAN_POINT('Ctrl Pts',(-0.218168590358226,0.00777884796634574,
0.0106341206922536));
#27393=CARTESIAN_POINT('Ctrl Pts',(-0.218176366284116,0.00768367623554517,
0.0106372600686865));
#27394=CARTESIAN_POINT('Ctrl Pts',(-0.218184322411749,0.00759032145937544,
0.0106388051579624));
#27395=CARTESIAN_POINT('Ctrl Pts',(-0.218192385381993,0.00749853455275086,
0.0106389724339549));
#27396=CARTESIAN_POINT('',(-0.218067140731952,0.00994796991712816,0.0103007556072607));
#27397=CARTESIAN_POINT('Ctrl Pts',(-0.218067140731952,0.00994796991712816,
0.0103007556072607));
#27398=CARTESIAN_POINT('Ctrl Pts',(-0.218067114512319,0.00993046860657864,
0.0103056312397923));
#27399=CARTESIAN_POINT('Ctrl Pts',(-0.218067118414372,0.00991224463072161,
0.0103106497977678));
#27400=CARTESIAN_POINT('Ctrl Pts',(-0.218067160950739,0.00989326393083498,
0.0103158106977222));
#27401=CARTESIAN_POINT('Ctrl Pts',(-0.218067298393995,0.00983193360694396,
0.0103324865667715));
#27402=CARTESIAN_POINT('Ctrl Pts',(-0.218067841273241,0.00976267553591436,
0.0103505546203546));
#27403=CARTESIAN_POINT('Ctrl Pts',(-0.218068705378173,0.00969648956991687,
0.0103669952228347));
#27404=CARTESIAN_POINT('Ctrl Pts',(-0.218070433588036,0.00956411763792191,
0.0103998764277948));
#27405=CARTESIAN_POINT('Ctrl Pts',(-0.218073437444364,0.00944413893557428,
0.0104266653780147));
#27406=CARTESIAN_POINT('Ctrl Pts',(-0.218077040466343,0.00933195733859977,
0.0104497653775281));
#27407=CARTESIAN_POINT('Ctrl Pts',(-0.218078841977332,0.0092758665401125,
0.0104613153772848));
#27408=CARTESIAN_POINT('Ctrl Pts',(-0.218080794635338,0.00922171204223149,
0.0104718823298127));
#27409=CARTESIAN_POINT('Ctrl Pts',(-0.218082474141969,0.00917710991001544,
0.0104802748380597));
#27410=CARTESIAN_POINT('Ctrl Pts',(-0.2180841536486,0.00913250777779939,
0.0104886673463067));
#27411=CARTESIAN_POINT('Ctrl Pts',(-0.218085555727444,0.0090974952685411,
0.0104950768614037));
#27412=CARTESIAN_POINT('Ctrl Pts',(-0.218088070100538,0.00904085165419785,
0.0105048607679938));
#27413=CARTESIAN_POINT('Ctrl Pts',(-0.218090584473632,0.00898420803985461,
0.0105146446745839));
#27414=CARTESIAN_POINT('Ctrl Pts',(-0.218094219358009,0.00890586854398972,
0.0105274358597375));
#27415=CARTESIAN_POINT('Ctrl Pts',(-0.218097832002953,0.00883396461653103,
0.0105381790015194));
#27416=CARTESIAN_POINT('Ctrl Pts',(-0.218101444647896,0.00876206068907235,
0.0105489221433012));
#27417=CARTESIAN_POINT('Ctrl Pts',(-0.218105029025212,0.00869663063622081,
0.0105578856505614));
#27418=CARTESIAN_POINT('Ctrl Pts',(-0.218108834948437,0.0086308229479829,
0.0105662276970903));
#27419=CARTESIAN_POINT('Ctrl Pts',(-0.218116446794885,0.00849920757150708,
0.0105829117901482));
#27420=CARTESIAN_POINT('Ctrl Pts',(-0.218124951180851,0.00836605377240373,
0.0105968281293923));
#27421=CARTESIAN_POINT('Ctrl Pts',(-0.218133937516825,0.00823651643260574,
0.0106075978802791));
#27422=CARTESIAN_POINT('Ctrl Pts',(-0.218144870524618,0.00807891796869424,
0.0106207006365895));
#27423=CARTESIAN_POINT('Ctrl Pts',(-0.218156513090154,0.00792668571681208,
0.0106293143666714));
#27424=CARTESIAN_POINT('Ctrl Pts',(-0.218168590358226,0.00777884796634574,
0.0106341206922536));
#27425=CARTESIAN_POINT('',(-0.218240142405069,0.0120825022396936,0.00940257574060758));
#27426=CARTESIAN_POINT('Ctrl Pts',(-0.218240142405069,0.0120825022396936,
0.00940257574060758));
#27427=CARTESIAN_POINT('Ctrl Pts',(-0.218227634732032,0.012011138019393,
0.00944389882041555));
#27428=CARTESIAN_POINT('Ctrl Pts',(-0.218214333283586,0.0119322602189668,
0.00948802720542979));
#27429=CARTESIAN_POINT('Ctrl Pts',(-0.21820394437181,0.0118677561250279,
0.00952309834051516));
#27430=CARTESIAN_POINT('Ctrl Pts',(-0.218193555460033,0.0118032520310891,
0.00955816947560053));
#27431=CARTESIAN_POINT('Ctrl Pts',(-0.21818607359624,0.0117532614381398,
0.00958444739640607));
#27432=CARTESIAN_POINT('Ctrl Pts',(-0.218179879131554,0.0117108626589821,
0.0096064495912512));
#27433=CARTESIAN_POINT('Ctrl Pts',(-0.218173684666869,0.0116684638798244,
0.00962845178609632));
#27434=CARTESIAN_POINT('Ctrl Pts',(-0.218168779249113,0.0116336188534382,
0.0096461000314644));
#27435=CARTESIAN_POINT('Ctrl Pts',(-0.218166009981003,0.0116140367509713,
0.00965596779068263));
#27436=CARTESIAN_POINT('Ctrl Pts',(-0.218163240712894,0.0115944546485044,
0.00966583554990086));
#27437=CARTESIAN_POINT('Ctrl Pts',(-0.218162606670219,0.0115901572125468,
0.00966796681318666));
#27438=CARTESIAN_POINT('Ctrl Pts',(-0.218161139921569,0.0115785731573726,
0.00967374443478997));
#27439=CARTESIAN_POINT('Ctrl Pts',(-0.218158206424268,0.0115554050470242,
0.0096852996779966));
#27440=CARTESIAN_POINT('Ctrl Pts',(-0.218151944072019,0.01150304239737,
0.00971134617996922));
#27441=CARTESIAN_POINT('Ctrl Pts',(-0.218144576693071,0.0114339717952896,
0.0097443075472982));
#27442=CARTESIAN_POINT('Ctrl Pts',(-0.218137209314123,0.0113649011932092,
0.00977726891462718));
#27443=CARTESIAN_POINT('Ctrl Pts',(-0.218128734773963,0.0112791720929526,
0.00981724654533353));
#27444=CARTESIAN_POINT('Ctrl Pts',(-0.218119656687413,0.0111717758059659,
0.0098644073772456));
#27445=CARTESIAN_POINT('Ctrl Pts',(-0.218115117644138,0.0111180776624726,
0.00988798779320165));
#27446=CARTESIAN_POINT('Ctrl Pts',(-0.218110428342051,0.0110589494854822,
0.00991333451127713));
#27447=CARTESIAN_POINT('Ctrl Pts',(-0.218105811430685,0.0109950563350908,
0.00993980046272872));
#27448=CARTESIAN_POINT('Ctrl Pts',(-0.218101615715708,0.0109369920954247,
0.00996385195085639));
#27449=CARTESIAN_POINT('Ctrl Pts',(-0.218097479388685,0.0108750002765632,
0.00998884314078868));
#27450=CARTESIAN_POINT('Ctrl Pts',(-0.218093504352807,0.0108074520307542,
0.0100150801168543));
#27451=CARTESIAN_POINT('Ctrl Pts',(-0.218093105309792,0.0108006710465076,
0.0100177139753542));
#27452=CARTESIAN_POINT('Ctrl Pts',(-0.218092707892206,0.010793834015395,
0.010020360228592));
#27453=CARTESIAN_POINT('Ctrl Pts',(-0.21809231220314,0.0107869392578784,
0.0100230190826078));
#27454=CARTESIAN_POINT('Ctrl Pts',(-0.218087974888293,0.0107113629109957,
0.0100521639035715));
#27455=CARTESIAN_POINT('Ctrl Pts',(-0.218083847156932,0.0106288204023902,
0.0100827571992526));
#27456=CARTESIAN_POINT('Ctrl Pts',(-0.218080324272248,0.0105466504959989,
0.0101118150425837));
#27457=CARTESIAN_POINT('Ctrl Pts',(-0.218078562829906,0.0105055655428032,
0.0101263439642493));
#27458=CARTESIAN_POINT('Ctrl Pts',(-0.218076951141839,0.0104645988975483,
0.0101405562838599));
#27459=CARTESIAN_POINT('Ctrl Pts',(-0.218075307620494,0.0104142110796976,
0.0101575130842937));
#27460=CARTESIAN_POINT('Ctrl Pts',(-0.21807366409915,0.0103638232618468,
0.0101744698847275));
#27461=CARTESIAN_POINT('Ctrl Pts',(-0.218071994487696,0.0103039249942364,
0.0101939079797174));
#27462=CARTESIAN_POINT('Ctrl Pts',(-0.218071182598693,0.0102734617826065,
0.0102036129024837));
#27463=CARTESIAN_POINT('Ctrl Pts',(-0.218070370709691,0.0102429985709766,
0.01021331782525));
#27464=CARTESIAN_POINT('Ctrl Pts',(-0.218070410527697,0.0102420558816815,
0.0102135637764575));
#27465=CARTESIAN_POINT('Ctrl Pts',(-0.218070223423177,0.0102316246750146,
0.0102168335306616));
#27466=CARTESIAN_POINT('Ctrl Pts',(-0.218070036318657,0.0102211934683478,
0.0102201032848658));
#27467=CARTESIAN_POINT('Ctrl Pts',(-0.218069623973603,0.0102012502108673,
0.0102263202343639));
#27468=CARTESIAN_POINT('Ctrl Pts',(-0.218069266473067,0.0101812898039636,
0.0102324502074999));
#27469=CARTESIAN_POINT('Ctrl Pts',(-0.218068551471994,0.0101413689901562,
0.0102447101537719));
#27470=CARTESIAN_POINT('Ctrl Pts',(-0.218068053649516,0.0101014089975905,
0.0102567221360035));
#27471=CARTESIAN_POINT('Ctrl Pts',(-0.218067671539871,0.0100547164560643,
0.0102703336166971));
#27472=CARTESIAN_POINT('Ctrl Pts',(-0.21806740768671,0.0100224744678928,
0.0102797325739003));
#27473=CARTESIAN_POINT('Ctrl Pts',(-0.21806719923304,0.0099870201303414,
0.0102898840623915));
#27474=CARTESIAN_POINT('Ctrl Pts',(-0.218067140731952,0.00994796991712816,
0.0103007556072607));
#27475=CARTESIAN_POINT('',(-0.218374802370667,0.012770849952475,0.00895972547844891));
#27476=CARTESIAN_POINT('Ctrl Pts',(-0.218374815649956,0.0127718879457763,
0.00896105065188488));
#27477=CARTESIAN_POINT('Ctrl Pts',(-0.218353771441862,0.0126721758023642,
0.00903141856439606));
#27478=CARTESIAN_POINT('Ctrl Pts',(-0.218331273836085,0.0125623045273881,
0.00910578154191035));
#27479=CARTESIAN_POINT('Ctrl Pts',(-0.218309124848712,0.0124504844741805,
0.00917776855508357));
#27480=CARTESIAN_POINT('Ctrl Pts',(-0.218286972241046,0.0123386461437777,
0.00924976733466765));
#27481=CARTESIAN_POINT('Ctrl Pts',(-0.218265157751142,0.0122252306802948,
0.00931992958099163));
#27482=CARTESIAN_POINT('Ctrl Pts',(-0.218240142405069,0.0120825022396936,
0.00940257574060758));
#27483=CARTESIAN_POINT('',(-0.217734598291091,0.0127648501815041,0.00895357626288772));
#27484=CARTESIAN_POINT('Ctrl Pts',(-0.218374739957786,0.0127719565711068,
0.00896100046641628));
#27485=CARTESIAN_POINT('Ctrl Pts',(-0.218331429070052,0.0127783087890815,
0.00895564837322821));
#27486=CARTESIAN_POINT('Ctrl Pts',(-0.218256946939598,0.0127887785152065,
0.00894674424652318));
#27487=CARTESIAN_POINT('Ctrl Pts',(-0.21821074281553,0.0127961462225746,
0.00894058692440315));
#27488=CARTESIAN_POINT('Ctrl Pts',(-0.218041570987848,0.0128061304184166,
0.0089301565708801));
#27489=CARTESIAN_POINT('Ctrl Pts',(-0.217906442184221,0.0127950441559907,
0.00893548464298887));
#27490=CARTESIAN_POINT('Ctrl Pts',(-0.217785680204843,0.0127750237429539,
0.00894736337346077));
#27491=CARTESIAN_POINT('Ctrl Pts',(-0.217734598291091,0.0127648501815041,
0.00895357626288772));
#27492=CARTESIAN_POINT('',(-0.217125125910816,0.0125755126764789,0.00907193450211442));
#27493=CARTESIAN_POINT('Ctrl Pts',(-0.217734109130233,0.0127647526978011,
0.00895363580049309));
#27494=CARTESIAN_POINT('Ctrl Pts',(-0.217682923213736,0.0127545455248966,
0.00895987032802755));
#27495=CARTESIAN_POINT('Ctrl Pts',(-0.21759918313078,0.0127337893410419,
0.00897289746848775));
#27496=CARTESIAN_POINT('Ctrl Pts',(-0.217407044851832,0.0126752427904671,
0.00900981145746635));
#27497=CARTESIAN_POINT('Ctrl Pts',(-0.217324996157004,0.0126461555887933,
0.00902814986930927));
#27498=CARTESIAN_POINT('Ctrl Pts',(-0.217195934007024,0.0126008953837128,
0.00905634036820808));
#27499=CARTESIAN_POINT('Ctrl Pts',(-0.217125125910815,0.0125755126764789,
0.00907193450211442));
#27500=CARTESIAN_POINT('',(-0.216865308842943,0.0101529809944104,0.0102146591943612));
#27501=CARTESIAN_POINT('Ctrl Pts',(-0.217125116861616,0.012575509432593,
0.00907193649502888));
#27502=CARTESIAN_POINT('Ctrl Pts',(-0.217103825873541,0.0124556142350541,
0.00915177820299817));
#27503=CARTESIAN_POINT('Ctrl Pts',(-0.21708543586629,0.0123492680897509,
0.00921865902026808));
#27504=CARTESIAN_POINT('Ctrl Pts',(-0.217069076401892,0.0122522130671093,
0.00927757091324666));
#27505=CARTESIAN_POINT('Ctrl Pts',(-0.217060896669693,0.0122036855557885,
0.00930702685973596));
#27506=CARTESIAN_POINT('Ctrl Pts',(-0.217053225625487,0.0121574472103491,
0.00933443792808312));
#27507=CARTESIAN_POINT('Ctrl Pts',(-0.217046930550406,0.0121191622263696,
0.00935679855708027));
#27508=CARTESIAN_POINT('Ctrl Pts',(-0.217040635475325,0.0120808772423901,
0.00937915918607743));
#27509=CARTESIAN_POINT('Ctrl Pts',(-0.217035713759174,0.0120506219046572,
0.00939659786253759));
#27510=CARTESIAN_POINT('Ctrl Pts',(-0.21702870095117,0.0120061367071534,
0.00942173938324392));
#27511=CARTESIAN_POINT('Ctrl Pts',(-0.217021688143166,0.0119616515096496,
0.00944688090395027));
#27512=CARTESIAN_POINT('Ctrl Pts',(-0.217012588916355,0.0119028062528194,
0.00947949707937416));
#27513=CARTESIAN_POINT('Ctrl Pts',(-0.217004505587796,0.0118486712007352,
0.00950870635721085));
#27514=CARTESIAN_POINT('Ctrl Pts',(-0.216996422259236,0.011794536148651,
0.00953791563504754));
#27515=CARTESIAN_POINT('Ctrl Pts',(-0.216989351628543,0.0117451932488908,
0.00956387226315191));
#27516=CARTESIAN_POINT('Ctrl Pts',(-0.216982616444841,0.0116968197156397,
0.00958881655457117));
#27517=CARTESIAN_POINT('Ctrl Pts',(-0.216969146077438,0.0116000726491376,
0.00963870513740967));
#27518=CARTESIAN_POINT('Ctrl Pts',(-0.216957017981496,0.0115071990302703,
0.00968452334188844));
#27519=CARTESIAN_POINT('Ctrl Pts',(-0.21694575682019,0.0114110167413363,
0.00972996806454795));
#27520=CARTESIAN_POINT('Ctrl Pts',(-0.216923234497579,0.0112186521634682,
0.00982085750986698));
#27521=CARTESIAN_POINT('Ctrl Pts',(-0.216904190106109,0.0110128311572041,
0.00990977153176363));
#27522=CARTESIAN_POINT('Ctrl Pts',(-0.216890581505355,0.0107996070424065,
0.00999216578621756));
#27523=CARTESIAN_POINT('Ctrl Pts',(-0.216876972904601,0.0105863829276089,
0.0100745600406715));
#27524=CARTESIAN_POINT('Ctrl Pts',(-0.216868805975623,0.0103656090193981,
0.0101501540238545));
#27525=CARTESIAN_POINT('Ctrl Pts',(-0.21686536061782,0.0101561495392998,
0.010213698561222));
#27526=CARTESIAN_POINT('Ctrl Pts',(-0.216865343240117,0.0101550930670962,
0.0102140190673045));
#27527=CARTESIAN_POINT('Ctrl Pts',(-0.216865325981855,0.0101540368923536,
0.0102143392976063));
#27528=CARTESIAN_POINT('Ctrl Pts',(-0.216865308842943,0.0101529809944104,
0.0102146591943612));
#27529=CARTESIAN_POINT('',(-0.216992039547609,0.00749886050208332,0.0106118434853889));
#27530=CARTESIAN_POINT('Ctrl Pts',(-0.216865308842943,0.0101529809944104,
0.0102146591943612));
#27531=CARTESIAN_POINT('Ctrl Pts',(-0.216861927967694,0.00994469453364889,
0.0102777746867437));
#27532=CARTESIAN_POINT('Ctrl Pts',(-0.21686319133722,0.00974782023658563,
0.0103301991819165));
#27533=CARTESIAN_POINT('Ctrl Pts',(-0.216868396633366,0.00953023558922692,
0.0103799113220085));
#27534=CARTESIAN_POINT('Ctrl Pts',(-0.216871012475229,0.0094208917568765,
0.0104048933966999));
#27535=CARTESIAN_POINT('Ctrl Pts',(-0.216874630000908,0.00930625788422588,
0.0104289129990826));
#27536=CARTESIAN_POINT('Ctrl Pts',(-0.21687910933658,0.0091927203230611,
0.0104504437509994));
#27537=CARTESIAN_POINT('Ctrl Pts',(-0.216881349004416,0.0091359515424787,
0.0104612091269577));
#27538=CARTESIAN_POINT('Ctrl Pts',(-0.216883802899309,0.00907946720242295,
0.0104714071013028));
#27539=CARTESIAN_POINT('Ctrl Pts',(-0.216886764362047,0.00901787666734833,
0.0104818695431398));
#27540=CARTESIAN_POINT('Ctrl Pts',(-0.216889725824785,0.00895628613227371,
0.0104923319849768));
#27541=CARTESIAN_POINT('Ctrl Pts',(-0.216893198774523,0.0088895590569111,
0.0105028838422591));
#27542=CARTESIAN_POINT('Ctrl Pts',(-0.216895951836754,0.00883901354239403,
0.0105104550763784));
#27543=CARTESIAN_POINT('Ctrl Pts',(-0.216898704898984,0.00878846802787697,
0.0105180263104978));
#27544=CARTESIAN_POINT('Ctrl Pts',(-0.216900732586707,0.00875413964732611,
0.0105228613321503));
#27545=CARTESIAN_POINT('Ctrl Pts',(-0.216903232709149,0.0087130859209821,
0.0105284362036829));
#27546=CARTESIAN_POINT('Ctrl Pts',(-0.216905732831591,0.00867203219463808,
0.0105340110752155));
#27547=CARTESIAN_POINT('Ctrl Pts',(-0.216908708333334,0.00862423631372646,
0.010540194832042));
#27548=CARTESIAN_POINT('Ctrl Pts',(-0.216911865038629,0.00857530837293379,
0.0105460897542788));
#27549=CARTESIAN_POINT('Ctrl Pts',(-0.216918178449217,0.00847745249134844,
0.0105578795987525));
#27550=CARTESIAN_POINT('Ctrl Pts',(-0.216925213052354,0.00837508469828663,
0.0105686748320112));
#27551=CARTESIAN_POINT('Ctrl Pts',(-0.21693318406884,0.00826407226117057,
0.0105782317652135));
#27552=CARTESIAN_POINT('Ctrl Pts',(-0.216949126069373,0.00804204783873716,
0.0105973455927233));
#27553=CARTESIAN_POINT('Ctrl Pts',(-0.216968817133433,0.00778544299277556,
0.0106113550316752));
#27554=CARTESIAN_POINT('Ctrl Pts',(-0.216992039472508,0.007498860496276,
0.0106118436486008));
#27555=CARTESIAN_POINT('',(-0.216882060774437,0.00589894167293227,0.0104673301115656));
#27556=CARTESIAN_POINT('Ctrl Pts',(-0.216992039614274,0.00749885874677076,
0.0106118436515835));
#27557=CARTESIAN_POINT('Ctrl Pts',(-0.216968696387162,0.00721250076742298,
0.010611279820427));
#27558=CARTESIAN_POINT('Ctrl Pts',(-0.216948881624643,0.00695603249159739,
0.010597224811972));
#27559=CARTESIAN_POINT('Ctrl Pts',(-0.216932813946421,0.00673401117115549,
0.0105780613240776));
#27560=CARTESIAN_POINT('Ctrl Pts',(-0.216924780107311,0.00662300051093453,
0.0105684795801305));
#27561=CARTESIAN_POINT('Ctrl Pts',(-0.216917682194779,0.00652060110169468,
0.0105576579948596));
#27562=CARTESIAN_POINT('Ctrl Pts',(-0.216911304122608,0.00642272431681689,
0.0105458427496648));
#27563=CARTESIAN_POINT('Ctrl Pts',(-0.216908115086522,0.006373785924378,
0.0105399351270675));
#27564=CARTESIAN_POINT('Ctrl Pts',(-0.216905106906988,0.00632598223781525,
0.0105337393045049));
#27565=CARTESIAN_POINT('Ctrl Pts',(-0.21690257496323,0.00628486308718463,
0.0105281454815176));
#27566=CARTESIAN_POINT('Ctrl Pts',(-0.216900043019471,0.00624374393655401,
0.0105225516585303));
#27567=CARTESIAN_POINT('Ctrl Pts',(-0.216897984395554,0.00620929264573658,
0.0105176895280296));
#27568=CARTESIAN_POINT('Ctrl Pts',(-0.216895196305536,0.00615881306811144,
0.0105101149587025));
#27569=CARTESIAN_POINT('Ctrl Pts',(-0.216892408215518,0.0061083334904863,
0.0105025403893753));
#27570=CARTESIAN_POINT('Ctrl Pts',(-0.216888896080399,0.00604186083493618,
0.0104920119045022));
#27571=CARTESIAN_POINT('Ctrl Pts',(-0.216885892590301,0.00598048099048582,
0.0104815726477788));
#27572=CARTESIAN_POINT('Ctrl Pts',(-0.216884519120359,0.00595241252061771,
0.0104767988663297));
#27573=CARTESIAN_POINT('Ctrl Pts',(-0.216883251207378,0.00592540375787019,
0.0104720739912376));
#27574=CARTESIAN_POINT('Ctrl Pts',(-0.216882060774437,0.00589894167293226,
0.0104673301115656));
#27575=CARTESIAN_POINT('',(-0.216081273279547,0.00590074222848907,0.0104497344249182));
#27576=CARTESIAN_POINT('Ctrl Pts',(-0.216882060774437,0.00589894167293227,
0.0104673301115656));
#27577=CARTESIAN_POINT('Ctrl Pts',(-0.216081273279547,0.00590074222848907,
0.0104497344249183));
#27578=CARTESIAN_POINT('',(-0.216192972388059,0.00749913681337735,0.0105937841926617));
#27579=CARTESIAN_POINT('Ctrl Pts',(-0.216081273279547,0.00590074222848906,
0.0104497344249182));
#27580=CARTESIAN_POINT('Ctrl Pts',(-0.216082791066702,0.00593458609584699,
0.0104557868301711));
#27581=CARTESIAN_POINT('Ctrl Pts',(-0.21608442756336,0.00596908492338023,
0.0104617673197763));
#27582=CARTESIAN_POINT('Ctrl Pts',(-0.216086248348797,0.00600539180340494,
0.0104678328343025));
#27583=CARTESIAN_POINT('Ctrl Pts',(-0.216089278806263,0.00606581982170094,
0.0104779280840874));
#27584=CARTESIAN_POINT('Ctrl Pts',(-0.216092823551175,0.00613128149711444,
0.0104881115930235));
#27585=CARTESIAN_POINT('Ctrl Pts',(-0.216095619523186,0.00618069805460236,
0.0104953971611742));
#27586=CARTESIAN_POINT('Ctrl Pts',(-0.216098415495197,0.00623011461209028,
0.0105026827293249));
#27587=CARTESIAN_POINT('Ctrl Pts',(-0.216100457387313,0.00626345219645691,
0.0105073067142719));
#27588=CARTESIAN_POINT('Ctrl Pts',(-0.21610298377209,0.00630350339604497,
0.0105126662070077));
#27589=CARTESIAN_POINT('Ctrl Pts',(-0.216105510156868,0.00634355459563303,
0.0105180256997435));
#27590=CARTESIAN_POINT('Ctrl Pts',(-0.216108523881857,0.00639033543187153,
0.0105239940636935));
#27591=CARTESIAN_POINT('Ctrl Pts',(-0.216111720854193,0.00643827294491396,
0.0105296922193121));
#27592=CARTESIAN_POINT('Ctrl Pts',(-0.216118114798864,0.00653414797099881,
0.0105410885305492));
#27593=CARTESIAN_POINT('Ctrl Pts',(-0.216125238212349,0.00663463402037178,
0.0105515602441198));
#27594=CARTESIAN_POINT('Ctrl Pts',(-0.216133313517992,0.00674383793891926,
0.0105608594503349));
#27595=CARTESIAN_POINT('Ctrl Pts',(-0.216149464114079,0.00696224557046546,
0.0105794578452618));
#27596=CARTESIAN_POINT('Ctrl Pts',(-0.216169425475875,0.00721552619151367,
0.0105932247838232));
#27597=CARTESIAN_POINT('Ctrl Pts',(-0.216192972777483,0.00749913678123476,
0.0105937840962717));
#27598=CARTESIAN_POINT('',(-0.216064560542751,0.0101118708899842,0.0102094226853462));
#27599=CARTESIAN_POINT('Ctrl Pts',(-0.216192972843966,0.00749913758197346,
0.0105937840978508));
#27600=CARTESIAN_POINT('Ctrl Pts',(-0.216169511009818,0.0077829711165385,
0.010593280960363));
#27601=CARTESIAN_POINT('Ctrl Pts',(-0.21614963981566,0.00803639489599444,
0.0105795447869103));
#27602=CARTESIAN_POINT('Ctrl Pts',(-0.216133579485032,0.00825490153361357,
0.0105609705977376));
#27603=CARTESIAN_POINT('Ctrl Pts',(-0.216125549319719,0.00836415485242313,
0.0105516835031512));
#27604=CARTESIAN_POINT('Ctrl Pts',(-0.216118471086411,0.00846467923742192,
0.0105412215031039));
#27605=CARTESIAN_POINT('Ctrl Pts',(-0.216112126913198,0.00856054432573829,
0.0105298400899683));
#27606=CARTESIAN_POINT('Ctrl Pts',(-0.216108954826591,0.00860847686989648,
0.0105241493834004));
#27607=CARTESIAN_POINT('Ctrl Pts',(-0.216105967127652,0.00865524070694128,
0.0105181900976421));
#27608=CARTESIAN_POINT('Ctrl Pts',(-0.216103461654188,0.00869531413130442,
0.0105128334261085));
#27609=CARTESIAN_POINT('Ctrl Pts',(-0.216100956180724,0.00873538755566756,
0.010507476754575));
#27610=CARTESIAN_POINT('Ctrl Pts',(-0.216098930112014,0.00876878642481055,
0.0105028481395904));
#27611=CARTESIAN_POINT('Ctrl Pts',(-0.216096170413117,0.00881809405563216,
0.0104955859918311));
#27612=CARTESIAN_POINT('Ctrl Pts',(-0.21609341071422,0.00886740168645377,
0.0104883238440719));
#27613=CARTESIAN_POINT('Ctrl Pts',(-0.216089922626847,0.00893258466305817,
0.0104781947154111));
#27614=CARTESIAN_POINT('Ctrl Pts',(-0.216086943126735,0.00899279416913099,
0.0104681492303132));
#27615=CARTESIAN_POINT('Ctrl Pts',(-0.216083963626623,0.00905300367520381,
0.0104581037452152));
#27616=CARTESIAN_POINT('Ctrl Pts',(-0.216081488978781,0.00910826813489991,
0.0104483086920604));
#27617=CARTESIAN_POINT('Ctrl Pts',(-0.21607922328395,0.00916383245088221,
0.0104379673721727));
#27618=CARTESIAN_POINT('Ctrl Pts',(-0.216074691894287,0.0092749610828468,
0.0104172847323973));
#27619=CARTESIAN_POINT('Ctrl Pts',(-0.216071000885213,0.00938725056091497,
0.010394212662589));
#27620=CARTESIAN_POINT('Ctrl Pts',(-0.216068305929166,0.00949480823549394,
0.0103701146189438));
#27621=CARTESIAN_POINT('Ctrl Pts',(-0.216062916017071,0.00970992358465189,
0.0103219185316535));
#27622=CARTESIAN_POINT('Ctrl Pts',(-0.216061489104538,0.00990631862573795,
0.0102705706903127));
#27623=CARTESIAN_POINT('Ctrl Pts',(-0.216064560542751,0.0101118708899842,
0.0102094226853462));
#27624=CARTESIAN_POINT('',(-0.216308818597444,0.0125017236340575,0.00910474588717665));
#27625=CARTESIAN_POINT('Ctrl Pts',(-0.216064560542751,0.0101118708899842,
0.0102094226853462));
#27626=CARTESIAN_POINT('Ctrl Pts',(-0.216067631980963,0.0103174231542305,
0.0101482746803796));
#27627=CARTESIAN_POINT('Ctrl Pts',(-0.216075221767079,0.0105318422526481,
0.0100764137690631));
#27628=CARTESIAN_POINT('Ctrl Pts',(-0.216088333546939,0.010742801430779,
0.00999663280107556));
#27629=CARTESIAN_POINT('Ctrl Pts',(-0.216089497788197,0.0107615332415328,
0.00998954876705846));
#27630=CARTESIAN_POINT('Ctrl Pts',(-0.216090705584094,0.0107802390027244,
0.00998240422592453));
#27631=CARTESIAN_POINT('Ctrl Pts',(-0.216091955010119,0.0107989083874413,
0.00997520316767751));
#27632=CARTESIAN_POINT('Ctrl Pts',(-0.216104776721723,0.0109904951337436,
0.0099013053215298));
#27633=CARTESIAN_POINT('Ctrl Pts',(-0.216121982515131,0.011178144367165,
0.00982123433870025));
#27634=CARTESIAN_POINT('Ctrl Pts',(-0.216141492564637,0.0113514549451286,
0.0097409837926396));
#27635=CARTESIAN_POINT('Ctrl Pts',(-0.216152198178685,0.0114465544556392,
0.00969694846751261));
#27636=CARTESIAN_POINT('Ctrl Pts',(-0.216163593829438,0.0115374139528911,
0.00965302332847526));
#27637=CARTESIAN_POINT('Ctrl Pts',(-0.216176229165743,0.0116325830866664,
0.00960496228856018));
#27638=CARTESIAN_POINT('Ctrl Pts',(-0.216182546833896,0.0116801676535541,
0.00958093176860265));
#27639=CARTESIAN_POINT('Ctrl Pts',(-0.216189174365757,0.011728828677417,
0.00955586940376413));
#27640=CARTESIAN_POINT('Ctrl Pts',(-0.216196770953834,0.011782465366349,
0.00952753419512687));
#27641=CARTESIAN_POINT('Ctrl Pts',(-0.216204367541912,0.011836102055281,
0.0094991989864896));
#27642=CARTESIAN_POINT('Ctrl Pts',(-0.216212936459505,0.0118946326686426,
0.00946743362499819));
#27643=CARTESIAN_POINT('Ctrl Pts',(-0.216219428400284,0.0119382154723126,
0.00944332261912472));
#27644=CARTESIAN_POINT('Ctrl Pts',(-0.216225920341063,0.0119817982759826,
0.00941921161325124));
#27645=CARTESIAN_POINT('Ctrl Pts',(-0.216230330548599,0.0120105625630745,
0.00940298648815025));
#27646=CARTESIAN_POINT('Ctrl Pts',(-0.216236085834532,0.0120477886518902,
0.00938172145544078));
#27647=CARTESIAN_POINT('Ctrl Pts',(-0.216241841120465,0.012085014740706,
0.0093604564227313));
#27648=CARTESIAN_POINT('Ctrl Pts',(-0.21624894412124,0.0121306276008068,
0.00933402218323825));
#27649=CARTESIAN_POINT('Ctrl Pts',(-0.216256536977254,0.0121787064133767,
0.00930549209652678));
#27650=CARTESIAN_POINT('Ctrl Pts',(-0.216271722689283,0.0122748640385166,
0.00924843192310387));
#27651=CARTESIAN_POINT('Ctrl Pts',(-0.216288863445513,0.0123810212896488,
0.00918320633356622));
#27652=CARTESIAN_POINT('Ctrl Pts',(-0.216308820388115,0.0125016658513436,
0.00910465761837708));
#27653=CARTESIAN_POINT('',(-0.215098009459442,0.0124568456463798,0.0091097211321646));
#27654=CARTESIAN_POINT('',(-0.215098005579294,0.0124567804451349,0.00910961844171237));
#27655=CARTESIAN_POINT('',(-0.214992631591026,0.00749947366491129,0.0105666553962969));
#27656=CARTESIAN_POINT('Ctrl Pts',(-0.215098003539502,0.0124568465122051,
0.00910972101494852));
#27657=CARTESIAN_POINT('Ctrl Pts',(-0.215078872046694,0.0123380764007811,
0.00918586969150996));
#27658=CARTESIAN_POINT('Ctrl Pts',(-0.215054131147941,0.0121807387915435,
0.00928132552116643));
#27659=CARTESIAN_POINT('Ctrl Pts',(-0.215026675832497,0.0119991748863345,
0.00938495086713676));
#27660=CARTESIAN_POINT('Ctrl Pts',(-0.215013610883414,0.0119113355207368,
0.00943387856890056));
#27661=CARTESIAN_POINT('Ctrl Pts',(-0.214989031420947,0.0117378895077981,
0.00952674741057423));
#27662=CARTESIAN_POINT('Ctrl Pts',(-0.214963576161329,0.0115442929638235,
0.00962484494645074));
#27663=CARTESIAN_POINT('Ctrl Pts',(-0.214925227292808,0.0112265332226401,
0.00977661166210876));
#27664=CARTESIAN_POINT('Ctrl Pts',(-0.214881441558165,0.0107160404592738,
0.00998992422239802));
#27665=CARTESIAN_POINT('Ctrl Pts',(-0.214860205463023,0.0100784557054517,
0.0102002397837531));
#27666=CARTESIAN_POINT('Ctrl Pts',(-0.214864228119364,0.00959024177348553,
0.0103262146705758));
#27667=CARTESIAN_POINT('Ctrl Pts',(-0.21487723133723,0.00920082508041648,
0.0104053314978383));
#27668=CARTESIAN_POINT('Ctrl Pts',(-0.214887103785318,0.00898179083587286,
0.0104437555890133));
#27669=CARTESIAN_POINT('Ctrl Pts',(-0.214897482284705,0.00878838978616738,
0.010473386966028));
#27670=CARTESIAN_POINT('Ctrl Pts',(-0.214903550412397,0.00868845669247843,
0.0104869713617598));
#27671=CARTESIAN_POINT('Ctrl Pts',(-0.21491541624627,0.00850295185423011,
0.010510401431549));
#27672=CARTESIAN_POINT('Ctrl Pts',(-0.214939980745825,0.00815449444337298,
0.0105460278742306));
#27673=CARTESIAN_POINT('Ctrl Pts',(-0.214969453551002,0.00777926145812896,
0.0105661478361195));
#27674=CARTESIAN_POINT('Ctrl Pts',(-0.214992631591026,0.00749947366491129,
0.0105666553962969));
#27675=CARTESIAN_POINT('',(-0.214881405086202,0.00590343232515273,0.010423413516648));
#27676=CARTESIAN_POINT('Ctrl Pts',(-0.214992631712683,0.00749947219635508,
0.0105666553989609));
#27677=CARTESIAN_POINT('Ctrl Pts',(-0.214969345086721,0.00721945056383405,
0.0105661127593133));
#27678=CARTESIAN_POINT('Ctrl Pts',(-0.214939718136512,0.00684386172483547,
0.0105459149352619));
#27679=CARTESIAN_POINT('Ctrl Pts',(-0.214914989990807,0.00649491171184848,
0.0105101571201946));
#27680=CARTESIAN_POINT('Ctrl Pts',(-0.214903034202549,0.00630918418157328,
0.010486651391931));
#27681=CARTESIAN_POINT('Ctrl Pts',(-0.214896903335095,0.00620889075875752,
0.0104729859984906));
#27682=CARTESIAN_POINT('Ctrl Pts',(-0.214887550141049,0.00603608466518826,
0.0104464571131324));
#27683=CARTESIAN_POINT('Ctrl Pts',(-0.214883083515895,0.00594134340781319,
0.0104301910449969));
#27684=CARTESIAN_POINT('Ctrl Pts',(-0.214881405086202,0.00590343232515273,
0.010423413516648));
#27685=CARTESIAN_POINT('',(-0.214076623138809,0.00590524964646623,0.0104056862898775));
#27686=CARTESIAN_POINT('Ctrl Pts',(-0.214881405971139,0.00590344010746865,
0.0104233697659896));
#27687=CARTESIAN_POINT('Ctrl Pts',(-0.214076623138809,0.00590524964646622,
0.0104056862898775));
#27688=CARTESIAN_POINT('',(-0.214193732109028,0.0074996355091127,0.0105485995725959));
#27689=CARTESIAN_POINT('Ctrl Pts',(-0.214076623138809,0.00590524964646623,
0.0104056862898775));
#27690=CARTESIAN_POINT('Ctrl Pts',(-0.214081030343595,0.0060102586589984,
0.0104243439605997));
#27691=CARTESIAN_POINT('Ctrl Pts',(-0.214086490632834,0.00611852560763557,
0.0104415773943015));
#27692=CARTESIAN_POINT('Ctrl Pts',(-0.214092160447561,0.00621752004041992,
0.0104557189458005));
#27693=CARTESIAN_POINT('Ctrl Pts',(-0.214098162696277,0.00632231873944863,
0.01047068964827));
#27694=CARTESIAN_POINT('Ctrl Pts',(-0.214104391052137,0.00641667668968166,
0.0104825643640814));
#27695=CARTESIAN_POINT('Ctrl Pts',(-0.214111719185919,0.00651975718570092,
0.010493857431119));
#27696=CARTESIAN_POINT('Ctrl Pts',(-0.21411538325281,0.00657129743371054,
0.0104995039646378));
#27697=CARTESIAN_POINT('Ctrl Pts',(-0.214119323016901,0.00662501987917694,
0.0105049718007339));
#27698=CARTESIAN_POINT('Ctrl Pts',(-0.214123856766003,0.00668403817010079,
0.0105103742411977));
#27699=CARTESIAN_POINT('Ctrl Pts',(-0.214128390515105,0.00674305646102463,
0.0105157766816615));
#27700=CARTESIAN_POINT('Ctrl Pts',(-0.214133521551491,0.00680738547514745,
0.0105209671307191));
#27701=CARTESIAN_POINT('Ctrl Pts',(-0.21413756648669,0.00685708916630594,
0.0105245747996913));
#27702=CARTESIAN_POINT('Ctrl Pts',(-0.214141611421888,0.00690679285746443,
0.0105281824686634));
#27703=CARTESIAN_POINT('Ctrl Pts',(-0.214144565043588,0.00694185507893422,
0.010530438346143));
#27704=CARTESIAN_POINT('Ctrl Pts',(-0.214148272384198,0.00698531422333201,
0.0105329838694676));
#27705=CARTESIAN_POINT('Ctrl Pts',(-0.214151979724807,0.00702877336772981,
0.0105355293927922));
#27706=CARTESIAN_POINT('Ctrl Pts',(-0.214156443777976,0.00708063634940085,
0.0105382319945326));
#27707=CARTESIAN_POINT('Ctrl Pts',(-0.214161201957962,0.0071351444945118,
0.0105405294888697));
#27708=CARTESIAN_POINT('Ctrl Pts',(-0.214170718317934,0.0072441607847337,
0.010545124477544));
#27709=CARTESIAN_POINT('Ctrl Pts',(-0.214181406291325,0.00736375332914952,
0.0105483155487178));
#27710=CARTESIAN_POINT('Ctrl Pts',(-0.214193732134263,0.00749963493590358,
0.0105485996009061));
#27711=CARTESIAN_POINT('',(-0.214298616704839,0.0123842992752686,0.00914002570287846));
#27712=CARTESIAN_POINT('Ctrl Pts',(-0.214193732082292,0.00749963550673335,
0.0105485995997545));
#27713=CARTESIAN_POINT('Ctrl Pts',(-0.21418135470816,0.00763558496278679,
0.0105483253328312));
#27714=CARTESIAN_POINT('Ctrl Pts',(-0.214170627765918,0.00775519907777331,
0.0105451404750745));
#27715=CARTESIAN_POINT('Ctrl Pts',(-0.214161082456179,0.00786421691816746,
0.0105405524240497));
#27716=CARTESIAN_POINT('Ctrl Pts',(-0.21415630979463,0.00791872591465589,
0.0105382583953265));
#27717=CARTESIAN_POINT('Ctrl Pts',(-0.214151833770909,0.00797058473444226,
0.0105355591998067));
#27718=CARTESIAN_POINT('Ctrl Pts',(-0.214148119499745,0.00801400838918349,
0.0105330187644806));
#27719=CARTESIAN_POINT('Ctrl Pts',(-0.214144405228581,0.00805743204392473,
0.0105304783291545));
#27720=CARTESIAN_POINT('Ctrl Pts',(-0.214141449705021,0.00809242746166554,
0.0105282297214948));
#27721=CARTESIAN_POINT('Ctrl Pts',(-0.214137397798384,0.0081421383557626,
0.0105246256114229));
#27722=CARTESIAN_POINT('Ctrl Pts',(-0.214133345891746,0.00819184924985966,
0.010521021501351));
#27723=CARTESIAN_POINT('Ctrl Pts',(-0.214128202838708,0.0082562594338092,
0.0105158298221815));
#27724=CARTESIAN_POINT('Ctrl Pts',(-0.214123663791741,0.00831534124163444,
0.010510425603309));
#27725=CARTESIAN_POINT('Ctrl Pts',(-0.214119124744774,0.00837442304945969,
0.0105050213844365));
#27726=CARTESIAN_POINT('Ctrl Pts',(-0.214115186372202,0.00842819143853195,
0.0104995525234799));
#27727=CARTESIAN_POINT('Ctrl Pts',(-0.214111522655542,0.00847986203160938,
0.0104938941059396));
#27728=CARTESIAN_POINT('Ctrl Pts',(-0.214104195222222,0.00858320321776425,
0.0104825772708589));
#27729=CARTESIAN_POINT('Ctrl Pts',(-0.214097963705752,0.00867815821440496,
0.0104706218623882));
#27730=CARTESIAN_POINT('Ctrl Pts',(-0.214092018994477,0.00878283988616916,
0.0104556648092747));
#27731=CARTESIAN_POINT('Ctrl Pts',(-0.214086074283202,0.00888752155793336,
0.0104407077561611));
#27732=CARTESIAN_POINT('Ctrl Pts',(-0.21408042455788,0.00900188078205631,
0.0104223849419874));
#27733=CARTESIAN_POINT('Ctrl Pts',(-0.214075995668272,0.00911209226776831,
0.0104025901996249));
#27734=CARTESIAN_POINT('Ctrl Pts',(-0.214071566778664,0.00922230375348032,
0.0103827954572624));
#27735=CARTESIAN_POINT('Ctrl Pts',(-0.214068354575988,0.00932840606684898,
0.0103617148722127));
#27736=CARTESIAN_POINT('Ctrl Pts',(-0.21406606092194,0.00943215845042625,
0.0103393090665216));
#27737=CARTESIAN_POINT('Ctrl Pts',(-0.214061473613844,0.0096396632175808,
0.0102944974551394));
#27738=CARTESIAN_POINT('Ctrl Pts',(-0.214060553047391,0.00983780282009029,
0.010244714261598));
#27739=CARTESIAN_POINT('Ctrl Pts',(-0.214064457168896,0.0100437599210286,
0.0101854017246378));
#27740=CARTESIAN_POINT('Ctrl Pts',(-0.214068361290401,0.0102497170219669,
0.0101260891876776));
#27741=CARTESIAN_POINT('Ctrl Pts',(-0.214077112891257,0.0104632184510982,
0.0100562165635347));
#27742=CARTESIAN_POINT('Ctrl Pts',(-0.214089778662037,0.0106579611285809,
0.00998505527974717));
#27743=CARTESIAN_POINT('Ctrl Pts',(-0.214092686874479,0.0107026763762739,
0.0099687157979662));
#27744=CARTESIAN_POINT('Ctrl Pts',(-0.214095800114063,0.0107464159991479,
0.00995234655654839));
#27745=CARTESIAN_POINT('Ctrl Pts',(-0.214099201263413,0.0107904022882614,
0.0099355014535182));
#27746=CARTESIAN_POINT('Ctrl Pts',(-0.214103206412418,0.0108421999672176,
0.00991566488043311));
#27747=CARTESIAN_POINT('Ctrl Pts',(-0.214107610809052,0.0108943415937377,
0.00989517215769459));
#27748=CARTESIAN_POINT('Ctrl Pts',(-0.214112549798375,0.0109487698960818,
0.00987316106416006));
#27749=CARTESIAN_POINT('Ctrl Pts',(-0.214121682948841,0.0110494183976918,
0.00983245827741794));
#27750=CARTESIAN_POINT('Ctrl Pts',(-0.214132652227213,0.0111577726619784,
0.00978628689672306));
#27751=CARTESIAN_POINT('Ctrl Pts',(-0.214143344904991,0.0112548181255048,
0.00974288121974354));
#27752=CARTESIAN_POINT('Ctrl Pts',(-0.214154037582768,0.0113518635890311,
0.00969947554276402));
#27753=CARTESIAN_POINT('Ctrl Pts',(-0.214164444648207,0.011437799618632,
0.00965926249227631));
#27754=CARTESIAN_POINT('Ctrl Pts',(-0.214176207369434,0.0115304860340288,
0.00961406849670311));
#27755=CARTESIAN_POINT('Ctrl Pts',(-0.214182088730047,0.0115768292417272,
0.00959147149891651));
#27756=CARTESIAN_POINT('Ctrl Pts',(-0.214188309585668,0.0116248432647129,
0.00956760069860009));
#27757=CARTESIAN_POINT('Ctrl Pts',(-0.21419536162867,0.0116774425761363,
0.00954078007922124));
#27758=CARTESIAN_POINT('Ctrl Pts',(-0.214202413671673,0.0117300418875597,
0.00951395945984239));
#27759=CARTESIAN_POINT('Ctrl Pts',(-0.214210299808724,0.0117871572668679,
0.00948405000663253));
#27760=CARTESIAN_POINT('Ctrl Pts',(-0.21421633123925,0.0118301674283987,
0.00946109345410688));
#27761=CARTESIAN_POINT('Ctrl Pts',(-0.214222362669776,0.0118731775899295,
0.00943813690158122));
#27762=CARTESIAN_POINT('Ctrl Pts',(-0.214226535000872,0.0119021970009535,
0.00942234608511879));
#27763=CARTESIAN_POINT('Ctrl Pts',(-0.214231897691757,0.0119391914736748,
0.0094019549473163));
#27764=CARTESIAN_POINT('Ctrl Pts',(-0.214237260382641,0.0119761859463962,
0.00938156380951382));
#27765=CARTESIAN_POINT('Ctrl Pts',(-0.214243815897177,0.012021088180201,
0.00935645208833323));
#27766=CARTESIAN_POINT('Ctrl Pts',(-0.214250800777236,0.0120683176568899,
0.00932941698431488));
#27767=CARTESIAN_POINT('Ctrl Pts',(-0.214264770500878,0.0121627763636332,
0.00927534691745677));
#27768=CARTESIAN_POINT('Ctrl Pts',(-0.214280453653274,0.0122666637658923,
0.0092137826947823));
#27769=CARTESIAN_POINT('Ctrl Pts',(-0.214298616704839,0.0123842992752686,
0.00914002570287846));
#27770=CARTESIAN_POINT('',(-0.213096469059738,0.0123844644794285,0.0091159443654941));
#27771=CARTESIAN_POINT('',(-0.214298616958418,0.0123842966787186,0.00914001954130824));
#27772=CARTESIAN_POINT('',(-0.212993233607984,0.00749979378001809,0.0105214673239713));
#27773=CARTESIAN_POINT('Ctrl Pts',(-0.213096467719112,0.0123844633545295,
0.00911594223570887));
#27774=CARTESIAN_POINT('Ctrl Pts',(-0.213078420142776,0.0122675494764246,
0.00918905359400996));
#27775=CARTESIAN_POINT('Ctrl Pts',(-0.213054987849986,0.0121122935736829,
0.00928101043997303));
#27776=CARTESIAN_POINT('Ctrl Pts',(-0.213028799864989,0.0119324471038202,
0.00938126321650623));
#27777=CARTESIAN_POINT('Ctrl Pts',(-0.213016132724809,0.0118440752678231,
0.00942931729501684));
#27778=CARTESIAN_POINT('Ctrl Pts',(-0.21299265415091,0.0116732229327397,
0.00951867247851693));
#27779=CARTESIAN_POINT('Ctrl Pts',(-0.212967912547534,0.0114808221189265,
0.00961383183775737));
#27780=CARTESIAN_POINT('Ctrl Pts',(-0.212941941715022,0.0112643974489121,
0.00971525592341462));
#27781=CARTESIAN_POINT('Ctrl Pts',(-0.212909723910377,0.0109415762419991,
0.00985240537371464));
#27782=CARTESIAN_POINT('Ctrl Pts',(-0.212881010751181,0.0105690751444958,
0.00999510672893007));
#27783=CARTESIAN_POINT('Ctrl Pts',(-0.212859850312569,0.0100382998289195,
0.0101685314876836));
#27784=CARTESIAN_POINT('Ctrl Pts',(-0.212862264629342,0.00954044254449958,
0.0102927030439336));
#27785=CARTESIAN_POINT('Ctrl Pts',(-0.212875146130418,0.00911578320726967,
0.0103772945146413));
#27786=CARTESIAN_POINT('Ctrl Pts',(-0.212892087627978,0.00877197251470777,
0.0104321046170394));
#27787=CARTESIAN_POINT('Ctrl Pts',(-0.21290752809911,0.00853543064909932,
0.0104615284810289));
#27788=CARTESIAN_POINT('Ctrl Pts',(-0.212923142391528,0.00832054440866613,
0.0104835679646797));
#27789=CARTESIAN_POINT('Ctrl Pts',(-0.21293837109707,0.00812810624263752,
0.0104989675440877));
#27790=CARTESIAN_POINT('Ctrl Pts',(-0.212947295077721,0.00802145374136446,
0.0105057380077258));
#27791=CARTESIAN_POINT('Ctrl Pts',(-0.212965075598067,0.00781377237991675,
0.0105165932490521));
#27792=CARTESIAN_POINT('Ctrl Pts',(-0.212981009563412,0.00763489019592171,
0.0105211941227256));
#27793=CARTESIAN_POINT('Ctrl Pts',(-0.212993233607984,0.00749979378001809,
0.0105214673239713));
#27794=CARTESIAN_POINT('',(-0.212877121847906,0.00590794924227077,0.0103793151952651));
#27795=CARTESIAN_POINT('Ctrl Pts',(-0.212993233832586,0.00749979129778757,
0.0105214673289907));
#27796=CARTESIAN_POINT('Ctrl Pts',(-0.212981064276903,0.00736479612297992,
0.0105211891819061));
#27797=CARTESIAN_POINT('Ctrl Pts',(-0.212965188112315,0.00718593222917332,
0.0105165874876166));
#27798=CARTESIAN_POINT('Ctrl Pts',(-0.212947440678806,0.00697802927922566,
0.0105057127229899));
#27799=CARTESIAN_POINT('Ctrl Pts',(-0.212938511600499,0.00687104507816289,
0.0104989140613425));
#27800=CARTESIAN_POINT('Ctrl Pts',(-0.212923279603605,0.00667828233926936,
0.010483467255871));
#27801=CARTESIAN_POINT('Ctrl Pts',(-0.212907633153483,0.00646298952442557,
0.0104613557234546));
#27802=CARTESIAN_POINT('Ctrl Pts',(-0.212892518991003,0.00623200226523625,
0.0104325693249221));
#27803=CARTESIAN_POINT('Ctrl Pts',(-0.212881462846515,0.00601154310194284,
0.0103975761963385));
#27804=CARTESIAN_POINT('Ctrl Pts',(-0.212877121847906,0.00590794924227077,
0.0103793151952651));
#27805=CARTESIAN_POINT('',(-0.212077933064703,0.00590974366334612,0.0103617691152544));
#27806=CARTESIAN_POINT('Ctrl Pts',(-0.212877121524224,0.00590794670319015,
0.0103793296663314));
#27807=CARTESIAN_POINT('Ctrl Pts',(-0.212077933064703,0.00590974366334613,
0.0103617691152544));
#27808=CARTESIAN_POINT('',(-0.212194330076657,0.00749995162518921,0.0105034114101302));
#27809=CARTESIAN_POINT('Ctrl Pts',(-0.212077933064703,0.00590974366334612,
0.0103617691152544));
#27810=CARTESIAN_POINT('Ctrl Pts',(-0.212082368745612,0.00601342674098364,
0.010380079592749));
#27811=CARTESIAN_POINT('Ctrl Pts',(-0.212087815760883,0.00612012877535262,
0.010396980289355));
#27812=CARTESIAN_POINT('Ctrl Pts',(-0.212093440442612,0.00621771619664684,
0.0104108738576259));
#27813=CARTESIAN_POINT('Ctrl Pts',(-0.212099476969926,0.00632244907977018,
0.0104257847287463));
#27814=CARTESIAN_POINT('Ctrl Pts',(-0.212105709360604,0.00641663519518074,
0.0104375997296922));
#27815=CARTESIAN_POINT('Ctrl Pts',(-0.212113022792179,0.0065197130300263,
0.0104488559154187));
#27816=CARTESIAN_POINT('Ctrl Pts',(-0.212116679507966,0.00657125194744908,
0.010454484008282));
#27817=CARTESIAN_POINT('Ctrl Pts',(-0.212120607255694,0.0066250154413234,
0.0104599382687491));
#27818=CARTESIAN_POINT('Ctrl Pts',(-0.212125117953049,0.00668407316279022,
0.0104653259590911));
#27819=CARTESIAN_POINT('Ctrl Pts',(-0.212129628650405,0.00674313088425705,
0.0104707136494332));
#27820=CARTESIAN_POINT('Ctrl Pts',(-0.212134725573122,0.0068074975565799,
0.0104758893432661));
#27821=CARTESIAN_POINT('Ctrl Pts',(-0.212138749104645,0.00685733713676164,
0.0104794930978266));
#27822=CARTESIAN_POINT('Ctrl Pts',(-0.212142772636168,0.00690717671694339,
0.0104830968523871));
#27823=CARTESIAN_POINT('Ctrl Pts',(-0.212145717600668,0.00694247322496747,
0.0104853580454887));
#27824=CARTESIAN_POINT('Ctrl Pts',(-0.212149400129846,0.00698607185520561,
0.0104878990841841));
#27825=CARTESIAN_POINT('Ctrl Pts',(-0.212153082659023,0.00702967048544376,
0.0104904401228795));
#27826=CARTESIAN_POINT('Ctrl Pts',(-0.212157505724507,0.0070815780620546,
0.0104931294137848));
#27827=CARTESIAN_POINT('Ctrl Pts',(-0.212162213970043,0.00713608398057281,
0.0104954127786815));
#27828=CARTESIAN_POINT('Ctrl Pts',(-0.212171630461117,0.00724509581760926,
0.0104999795084749));
#27829=CARTESIAN_POINT('Ctrl Pts',(-0.212182182843636,0.00736449674603688,
0.0105031361654474));
#27830=CARTESIAN_POINT('Ctrl Pts',(-0.212194330095429,0.0074999511942267,
0.0105034114311707));
#27831=CARTESIAN_POINT('',(-0.212297175950961,0.0123849010587109,0.00909973979562649));
#27832=CARTESIAN_POINT('Ctrl Pts',(-0.212194330056779,0.00749995162344025,
0.0105034114302995));
#27833=CARTESIAN_POINT('Ctrl Pts',(-0.212182132380261,0.00763540882905098,
0.0105031364739071));
#27834=CARTESIAN_POINT('Ctrl Pts',(-0.212171540637664,0.00775478092759007,
0.0104999805125386));
#27835=CARTESIAN_POINT('Ctrl Pts',(-0.212162092907394,0.00786375793232145,
0.0104954163568162));
#27836=CARTESIAN_POINT('Ctrl Pts',(-0.21215736903727,0.00791824649223841,
0.0104931342765446));
#27837=CARTESIAN_POINT('Ctrl Pts',(-0.212152932382641,0.00797013520137814,
0.0104904465348834));
#27838=CARTESIAN_POINT('Ctrl Pts',(-0.212149241231138,0.00801368798592748,
0.0104879090327744));
#27839=CARTESIAN_POINT('Ctrl Pts',(-0.212145550079636,0.0080572407704768,
0.0104853715306654));
#27840=CARTESIAN_POINT('Ctrl Pts',(-0.212142601449191,0.00809246447236669,
0.0104831163236127));
#27841=CARTESIAN_POINT('Ctrl Pts',(-0.212138567500056,0.0081423062165424,
0.0104795141318218));
#27842=CARTESIAN_POINT('Ctrl Pts',(-0.212134533550921,0.00819214796071812,
0.010475911940031));
#27843=CARTESIAN_POINT('Ctrl Pts',(-0.212129419483177,0.00825659171681023,
0.0104707323120953));
#27844=CARTESIAN_POINT('Ctrl Pts',(-0.212124898353902,0.00831570414042495,
0.0104653409394229));
#27845=CARTESIAN_POINT('Ctrl Pts',(-0.212120377224626,0.00837481656403967,
0.0104599495667504));
#27846=CARTESIAN_POINT('Ctrl Pts',(-0.212116445728773,0.00842861246583197,
0.0104544931741294));
#27847=CARTESIAN_POINT('Ctrl Pts',(-0.21211278424837,0.00848025913524566,
0.0104488535403145));
#27848=CARTESIAN_POINT('Ctrl Pts',(-0.212105461287565,0.00858355247407304,
0.0104375742726846));
#27849=CARTESIAN_POINT('Ctrl Pts',(-0.212099215586247,0.00867825431068825,
0.0104256859327208));
#27850=CARTESIAN_POINT('Ctrl Pts',(-0.212093221159177,0.00878282659072353,
0.0104107923438481));
#27851=CARTESIAN_POINT('Ctrl Pts',(-0.212087226732106,0.0088873988707588,
0.0103958987549755));
#27852=CARTESIAN_POINT('Ctrl Pts',(-0.212081491858564,0.00900179202119997,
0.0103776313788772));
#27853=CARTESIAN_POINT('Ctrl Pts',(-0.212076978987956,0.00911199897354088,
0.0103579020720291));
#27854=CARTESIAN_POINT('Ctrl Pts',(-0.212072466117349,0.00922220592588179,
0.0103381727651811));
#27855=CARTESIAN_POINT('Ctrl Pts',(-0.212069171050528,0.00932826550458844,
0.0103171699030088));
#27856=CARTESIAN_POINT('Ctrl Pts',(-0.212066791644702,0.00943199934212568,
0.0102948428129182));
#27857=CARTESIAN_POINT('Ctrl Pts',(-0.212062032833051,0.00963946701720017,
0.0102501886327371));
#27858=CARTESIAN_POINT('Ctrl Pts',(-0.212060929441922,0.00983766460797513,
0.0102005566356354));
#27859=CARTESIAN_POINT('Ctrl Pts',(-0.212064581442097,0.0100435201415751,
0.0101414775852836));
#27860=CARTESIAN_POINT('Ctrl Pts',(-0.212068233442271,0.0102493756751751,
0.0100823985349317));
#27861=CARTESIAN_POINT('Ctrl Pts',(-0.212076662975467,0.010462624545103,
0.0100128706935483));
#27862=CARTESIAN_POINT('Ctrl Pts',(-0.212089094170597,0.0106577554360329,
0.00994182361406666));
#27863=CARTESIAN_POINT('Ctrl Pts',(-0.212091761677008,0.0106996269453244,
0.0099265782142508));
#27864=CARTESIAN_POINT('Ctrl Pts',(-0.212094612320762,0.0107406751960078,
0.00991129437080939));
#27865=CARTESIAN_POINT('Ctrl Pts',(-0.212097710996392,0.0107818588971139,
0.00989562568130839));
#27866=CARTESIAN_POINT('Ctrl Pts',(-0.212101832592334,0.0108366379690795,
0.00987478451728645));
#27867=CARTESIAN_POINT('Ctrl Pts',(-0.212106393007951,0.0108916597408158,
0.00985326912746405));
#27868=CARTESIAN_POINT('Ctrl Pts',(-0.212111544956238,0.0109491208093745,
0.00983011378293056));
#27869=CARTESIAN_POINT('Ctrl Pts',(-0.212120570213998,0.0110497819429915,
0.0097895499144105));
#27870=CARTESIAN_POINT('Ctrl Pts',(-0.212131418571356,0.0111578178242854,
0.00974368193973834));
#27871=CARTESIAN_POINT('Ctrl Pts',(-0.212142039045027,0.0112547719580293,
0.00970048378486729));
#27872=CARTESIAN_POINT('Ctrl Pts',(-0.212152659518698,0.0113517260917732,
0.00965728562999623));
#27873=CARTESIAN_POINT('Ctrl Pts',(-0.212163043358788,0.0114377915105051,
0.00961717228658461));
#27874=CARTESIAN_POINT('Ctrl Pts',(-0.212174781369626,0.0115305319976495,
0.00957213117622237));
#27875=CARTESIAN_POINT('Ctrl Pts',(-0.212180650375044,0.0115769022412217,
0.00954961062104125));
#27876=CARTESIAN_POINT('Ctrl Pts',(-0.212186858479183,0.0116249251490129,
0.00952583071720044));
#27877=CARTESIAN_POINT('Ctrl Pts',(-0.212193904618974,0.0116775623276343,
0.00949909874670926));
#27878=CARTESIAN_POINT('Ctrl Pts',(-0.212200950758764,0.0117301995062557,
0.00947236677621809));
#27879=CARTESIAN_POINT('Ctrl Pts',(-0.212208837846504,0.0117873817604858,
0.00944254326647152));
#27880=CARTESIAN_POINT('Ctrl Pts',(-0.212214862593021,0.0118303815249037,
0.00941968588074516));
#27881=CARTESIAN_POINT('Ctrl Pts',(-0.212220887339537,0.0118733812893216,
0.0093968284950188));
#27882=CARTESIAN_POINT('Ctrl Pts',(-0.212225045352742,0.0119023127283524,
0.00938115035527493));
#27883=CARTESIAN_POINT('Ctrl Pts',(-0.212230400693812,0.0119392716659875,
0.00936086398329727));
#27884=CARTESIAN_POINT('Ctrl Pts',(-0.212235756034883,0.0119762306036225,
0.00934057761131961));
#27885=CARTESIAN_POINT('Ctrl Pts',(-0.212242311164843,0.0120211499898962,
0.00931556268835316));
#27886=CARTESIAN_POINT('Ctrl Pts',(-0.212249298978313,0.0120684169725973,
0.00928862110546898));
#27887=CARTESIAN_POINT('Ctrl Pts',(-0.2122632745675,0.0121629506826447,
0.00923473808524962));
#27888=CARTESIAN_POINT('Ctrl Pts',(-0.212278976851095,0.0122669943691938,
0.0091733484633276));
#27889=CARTESIAN_POINT('Ctrl Pts',(-0.212297175950961,0.0123849010587109,
0.00909973979562649));
#27890=CARTESIAN_POINT('',(-0.211094963303624,0.0123855555142644,0.00907540141503557));
#27891=CARTESIAN_POINT('',(-0.212297176216748,0.0123848982829031,0.00909973325119912));
#27892=CARTESIAN_POINT('',(-0.210993898514632,0.00749995658642614,0.010476280662273));
#27893=CARTESIAN_POINT('Ctrl Pts',(-0.211094961783628,0.0123855543264941,
0.00907539913122092));
#27894=CARTESIAN_POINT('Ctrl Pts',(-0.211076890136153,0.012268357395815,
0.00914837879912795));
#27895=CARTESIAN_POINT('Ctrl Pts',(-0.211053444315123,0.0121128461295332,
0.00924009652403312));
#27896=CARTESIAN_POINT('Ctrl Pts',(-0.211027274789818,0.0119329009254192,
0.0093399877574131));
#27897=CARTESIAN_POINT('Ctrl Pts',(-0.211014657068081,0.0118447643381785,
0.00938772124358589));
#27898=CARTESIAN_POINT('Ctrl Pts',(-0.21099119418584,0.0116736959797512,
0.00947683380478672));
#27899=CARTESIAN_POINT('Ctrl Pts',(-0.210966522628683,0.0114812428550573,
0.00957164908266));
#27900=CARTESIAN_POINT('Ctrl Pts',(-0.210940620910424,0.0112643612015598,
0.00967287560159098));
#27901=CARTESIAN_POINT('Ctrl Pts',(-0.210908819689275,0.0109427780958805,
0.00980901902062219));
#27902=CARTESIAN_POINT('Ctrl Pts',(-0.210880462883198,0.0105684325415033,
0.00995195000100696));
#27903=CARTESIAN_POINT('Ctrl Pts',(-0.210860078776075,0.0100383092010752,
0.0101244849284952));
#27904=CARTESIAN_POINT('Ctrl Pts',(-0.210862935637832,0.00954053436561135,
0.01024825280501));
#27905=CARTESIAN_POINT('Ctrl Pts',(-0.210876137375512,0.00911593919119299,
0.0103325648865413));
#27906=CARTESIAN_POINT('Ctrl Pts',(-0.210893328842,0.00877175418342708,
0.0103872508672743));
#27907=CARTESIAN_POINT('Ctrl Pts',(-0.210908796910629,0.00853585371980837,
0.0104165008407334));
#27908=CARTESIAN_POINT('Ctrl Pts',(-0.210924389683485,0.00832083102382324,
0.0104384918762313));
#27909=CARTESIAN_POINT('Ctrl Pts',(-0.210939545249769,0.00812824961765805,
0.0104538562101529));
#27910=CARTESIAN_POINT('Ctrl Pts',(-0.210948448409464,0.00802099004519663,
0.0104606402662976));
#27911=CARTESIAN_POINT('Ctrl Pts',(-0.21096608665718,0.00781318629174079,
0.0104714488432744));
#27912=CARTESIAN_POINT('Ctrl Pts',(-0.210981836917698,0.00763462031690367,
0.0104760087040924));
#27913=CARTESIAN_POINT('Ctrl Pts',(-0.210993898514632,0.00749995658642614,
0.010476280662273));
#27914=CARTESIAN_POINT('',(-0.210878462469796,0.00591244389125894,0.0103353945802353));
#27915=CARTESIAN_POINT('Ctrl Pts',(-0.210993898714441,0.00749995435564087,
0.0104762806667779));
#27916=CARTESIAN_POINT('Ctrl Pts',(-0.210981892668771,0.00736532351394722,
0.0104760086450893));
#27917=CARTESIAN_POINT('Ctrl Pts',(-0.210966203249496,0.00718669232467104,
0.0104714501353086));
#27918=CARTESIAN_POINT('Ctrl Pts',(-0.210948605953594,0.00697858674150669,
0.0104606209082496));
#27919=CARTESIAN_POINT('Ctrl Pts',(-0.210939703683893,0.00687096559900909,
0.0104538079458758));
#27920=CARTESIAN_POINT('Ctrl Pts',(-0.21092455816711,0.00667800085658727,
0.010438393086424));
#27921=CARTESIAN_POINT('Ctrl Pts',(-0.210908952138233,0.00646249488114474,
0.0104163222518967));
#27922=CARTESIAN_POINT('Ctrl Pts',(-0.210893929543052,0.00623342510638356,
0.0103878647232971));
#27923=CARTESIAN_POINT('Ctrl Pts',(-0.210882826575908,0.00601460089362695,
0.0103532881465335));
#27924=CARTESIAN_POINT('Ctrl Pts',(-0.210878462469796,0.00591244389125894,
0.0103353945802353));
#27925=CARTESIAN_POINT('',(-0.21007929998055,0.00591424122749678,0.0103178320466886));
#27926=CARTESIAN_POINT('Ctrl Pts',(-0.210878462054166,0.00591244065125743,
0.0103354131641705));
#27927=CARTESIAN_POINT('Ctrl Pts',(-0.210079299576428,0.00591423755299386,
0.0103178531839906));
#27928=CARTESIAN_POINT('',(-0.210194951358703,0.00750007523249054,0.0104582237667519));
#27929=CARTESIAN_POINT('Ctrl Pts',(-0.21007929998055,0.00591424122749678,
0.0103178320466886));
#27930=CARTESIAN_POINT('Ctrl Pts',(-0.210083751067343,0.00601645214670358,
0.0103356854655352));
#27931=CARTESIAN_POINT('Ctrl Pts',(-0.210095071594484,0.00623600174548137,
0.0103702841806485));
#27932=CARTESIAN_POINT('Ctrl Pts',(-0.210110128003962,0.00646332524691155,
0.010398431828706));
#27933=CARTESIAN_POINT('Ctrl Pts',(-0.210125776896694,0.00667853050594156,
0.0104204386569121));
#27934=CARTESIAN_POINT('Ctrl Pts',(-0.21014095902768,0.00687163015652102,
0.0104358281073399));
#27935=CARTESIAN_POINT('Ctrl Pts',(-0.21014977367735,0.00697823725658171,
0.010442563363362));
#27936=CARTESIAN_POINT('Ctrl Pts',(-0.21016731346144,0.0071860660981192,
0.0104533779643737));
#27937=CARTESIAN_POINT('Ctrl Pts',(-0.210182963205961,0.00736496853713723,
0.0104579539494083));
#27938=CARTESIAN_POINT('Ctrl Pts',(-0.210194951369192,0.00750007498543175,
0.0104582237809153));
#27939=CARTESIAN_POINT('',(-0.210295577942689,0.0123859825112166,0.00905923576391993));
#27940=CARTESIAN_POINT('Ctrl Pts',(-0.210194951347265,0.00750007523149893,
0.0104582237804177));
#27941=CARTESIAN_POINT('Ctrl Pts',(-0.210182907666862,0.00763523111115919,
0.010457950468014));
#27942=CARTESIAN_POINT('Ctrl Pts',(-0.210172431709479,0.00775451113746308,
0.0104548172251436));
#27943=CARTESIAN_POINT('Ctrl Pts',(-0.210163068965682,0.00786355077921227,
0.0104502697590671));
#27944=CARTESIAN_POINT('Ctrl Pts',(-0.210158387590943,0.00791807063317346,
0.010447996024649));
#27945=CARTESIAN_POINT('Ctrl Pts',(-0.210153985715518,0.00797002934151878,
0.0104453158402741));
#27946=CARTESIAN_POINT('Ctrl Pts',(-0.21015031426293,0.00801374514118166,
0.0104427776730748));
#27947=CARTESIAN_POINT('Ctrl Pts',(-0.210146642810342,0.00805746094084455,
0.0104402395058756));
#27948=CARTESIAN_POINT('Ctrl Pts',(-0.210143698823214,0.00809294059101559,
0.0104379743195514));
#27949=CARTESIAN_POINT('Ctrl Pts',(-0.210139683892845,0.0081429132131209,
0.0104343719254984));
#27950=CARTESIAN_POINT('Ctrl Pts',(-0.210135668962475,0.00819288583522622,
0.0104307695314454));
#27951=CARTESIAN_POINT('Ctrl Pts',(-0.210130588242887,0.00825733556983972,
0.0104256015122868));
#27952=CARTESIAN_POINT('Ctrl Pts',(-0.210126088751837,0.00831647279630859,
0.0104202212801215));
#27953=CARTESIAN_POINT('Ctrl Pts',(-0.210121589260786,0.00837561002277747,
0.0104148410479561));
#27954=CARTESIAN_POINT('Ctrl Pts',(-0.210117667730163,0.00842944937139556,
0.0104093936980803));
#27955=CARTESIAN_POINT('Ctrl Pts',(-0.210114012308968,0.00848109369784154,
0.0104037684374952));
#27956=CARTESIAN_POINT('Ctrl Pts',(-0.210106701466579,0.00858438235073352,
0.010392517916325));
#27957=CARTESIAN_POINT('Ctrl Pts',(-0.210100452137536,0.00867889688402659,
0.0103806850618465));
#27958=CARTESIAN_POINT('Ctrl Pts',(-0.210094415517649,0.00878350791480637,
0.0103658268947457));
#27959=CARTESIAN_POINT('Ctrl Pts',(-0.210088378897761,0.00888811894558615,
0.0103509687276449));
#27960=CARTESIAN_POINT('Ctrl Pts',(-0.210082563432376,0.00900277600701533,
0.0103327092752339));
#27961=CARTESIAN_POINT('Ctrl Pts',(-0.21007797133636,0.00911312815624517,
0.0103130047596318));
#27962=CARTESIAN_POINT('Ctrl Pts',(-0.210073379240344,0.00922348030547501,
0.0102933002440297));
#27963=CARTESIAN_POINT('Ctrl Pts',(-0.21007000621618,0.00932956712989777,
0.0102723434943911));
#27964=CARTESIAN_POINT('Ctrl Pts',(-0.210067544254891,0.00943326599643501,
0.0102500828349819));
#27965=CARTESIAN_POINT('Ctrl Pts',(-0.210062620332315,0.00964066372950947,
0.0102055615161635));
#27966=CARTESIAN_POINT('Ctrl Pts',(-0.210061333369762,0.00983854323490633,
0.0101561467361826));
#27967=CARTESIAN_POINT('Ctrl Pts',(-0.210064741391414,0.0100441652705734,
0.0100973199897705));
#27968=CARTESIAN_POINT('Ctrl Pts',(-0.210068149413066,0.0102497873062405,
0.0100384932433585));
#27969=CARTESIAN_POINT('Ctrl Pts',(-0.210076274349181,0.0104628899608491,
0.00996926186745797));
#27970=CARTESIAN_POINT('Ctrl Pts',(-0.210088469406629,0.0106584516234858,
0.00989829532363724));
#27971=CARTESIAN_POINT('Ctrl Pts',(-0.210090884318977,0.0106971774987838,
0.0098842422547009));
#27972=CARTESIAN_POINT('Ctrl Pts',(-0.210093457913029,0.0107352244438639,
0.00987014672261548));
#27973=CARTESIAN_POINT('Ctrl Pts',(-0.210096239220074,0.0107733155848942,
0.00985575027748959));
#27974=CARTESIAN_POINT('Ctrl Pts',(-0.210100480569403,0.0108314026039995,
0.00983379644359394));
#27975=CARTESIAN_POINT('Ctrl Pts',(-0.210105204948483,0.0108895968858756,
0.00981115310644442));
#27976=CARTESIAN_POINT('Ctrl Pts',(-0.210110586232912,0.010950395982138,
0.00978673331551824));
#27977=CARTESIAN_POINT('Ctrl Pts',(-0.210119496348177,0.0110510646910251,
0.00974630000359497));
#27978=CARTESIAN_POINT('Ctrl Pts',(-0.210130214863807,0.0111587657784774,
0.00970073002795545));
#27979=CARTESIAN_POINT('Ctrl Pts',(-0.210140752998032,0.0112556061415998,
0.00965773926679269));
#27980=CARTESIAN_POINT('Ctrl Pts',(-0.210151291132256,0.0113524465047223,
0.00961474850562993));
#27981=CARTESIAN_POINT('Ctrl Pts',(-0.210161640396964,0.011438612936933,
0.0095747400194307));
#27982=CARTESIAN_POINT('Ctrl Pts',(-0.210173341134653,0.0115313791441276,
0.00952985714870897));
#27983=CARTESIAN_POINT('Ctrl Pts',(-0.210179191503498,0.0115777622477249,
0.00950741571334811));
#27984=CARTESIAN_POINT('Ctrl Pts',(-0.210185380272374,0.0116257798470562,
0.00948372939897313));
#27985=CARTESIAN_POINT('Ctrl Pts',(-0.210192412741908,0.0116784375103859,
0.00945709044010566));
#27986=CARTESIAN_POINT('Ctrl Pts',(-0.210199445211442,0.0117310951737156,
0.00943045148123819));
#27987=CARTESIAN_POINT('Ctrl Pts',(-0.21020732429623,0.0117883237967492,
0.00940072009878417));
#27988=CARTESIAN_POINT('Ctrl Pts',(-0.210213336041793,0.0118313014592588,
0.00937796454941558));
#27989=CARTESIAN_POINT('Ctrl Pts',(-0.210219347787355,0.0118742791217684,
0.009355209000047));
#27990=CARTESIAN_POINT('Ctrl Pts',(-0.210223487807067,0.0119031195863775,
0.00933964247891056));
#27991=CARTESIAN_POINT('Ctrl Pts',(-0.210228830139808,0.01194003302514,
0.00931946325008595));
#27992=CARTESIAN_POINT('Ctrl Pts',(-0.210234172472549,0.0119769464639024,
0.00929928402126134));
#27993=CARTESIAN_POINT('Ctrl Pts',(-0.210240719573932,0.0120218661345205,
0.00927437182809841));
#27994=CARTESIAN_POINT('Ctrl Pts',(-0.210247701848314,0.0120691509098138,
0.00924753170250139));
#27995=CARTESIAN_POINT('Ctrl Pts',(-0.210261666357686,0.0121637201936272,
0.00919385160273513));
#27996=CARTESIAN_POINT('Ctrl Pts',(-0.210277367518394,0.0122678692136601,
0.00913266022226723));
#27997=CARTESIAN_POINT('Ctrl Pts',(-0.210295577942689,0.0123859825112166,
0.00905923576391993));
#27998=CARTESIAN_POINT('',(-0.209093386669321,0.0123867890340704,0.00903485594096656));
#27999=CARTESIAN_POINT('',(-0.210295578218103,0.0123859796930808,0.009059229030905));
#28000=CARTESIAN_POINT('',(-0.208994544866511,0.00750001217157779,0.0104310935790768));
#28001=CARTESIAN_POINT('Ctrl Pts',(-0.209093384956975,0.0123867878335644,
0.00903485357938685));
#28002=CARTESIAN_POINT('Ctrl Pts',(-0.209075271471196,0.0122692180496618,
0.00910775390628676));
#28003=CARTESIAN_POINT('Ctrl Pts',(-0.209051790486463,0.0121133375619839,
0.00919929174406344));
#28004=CARTESIAN_POINT('Ctrl Pts',(-0.209025620677105,0.0119331891109362,
0.00929886865408172));
#28005=CARTESIAN_POINT('Ctrl Pts',(-0.209013043216911,0.0118452328040021,
0.00934630625189574));
#28006=CARTESIAN_POINT('Ctrl Pts',(-0.20898959237479,0.0116739217040356,
0.00943517733250513));
#28007=CARTESIAN_POINT('Ctrl Pts',(-0.20896498827012,0.0114813739337843,
0.00952965577098411));
#28008=CARTESIAN_POINT('Ctrl Pts',(-0.20893915704693,0.0112639714210063,
0.00963069685261997));
#28009=CARTESIAN_POINT('Ctrl Pts',(-0.208907791001968,0.0109436242567375,
0.00976581223976034));
#28010=CARTESIAN_POINT('Ctrl Pts',(-0.208879845713628,0.0105675636138655,
0.00990890057783304));
#28011=CARTESIAN_POINT('Ctrl Pts',(-0.208860241917163,0.0100378203115335,
0.0100805840213093));
#28012=CARTESIAN_POINT('Ctrl Pts',(-0.20886359193908,0.00954120967817297,
0.0102036756318696));
#28013=CARTESIAN_POINT('Ctrl Pts',(-0.208877126664812,0.00911647469127787,
0.0102877839561455));
#28014=CARTESIAN_POINT('Ctrl Pts',(-0.208894583352245,0.00877121788909045,
0.0103424510565681));
#28015=CARTESIAN_POINT('Ctrl Pts',(-0.208910056796663,0.00853595851793098,
0.0103715120818308));
#28016=CARTESIAN_POINT('Ctrl Pts',(-0.208925617543613,0.00832081882800243,
0.0103934437827441));
#28017=CARTESIAN_POINT('Ctrl Pts',(-0.208940687467563,0.00812822373671741,
0.0104087564496012));
#28018=CARTESIAN_POINT('Ctrl Pts',(-0.208949569648136,0.00802036799570133,
0.0104155514242314));
#28019=CARTESIAN_POINT('Ctrl Pts',(-0.208967066582641,0.00781248286347796,
0.0104263073185167));
#28020=CARTESIAN_POINT('Ctrl Pts',(-0.208982639473909,0.0076342416541042,
0.0104308243299841));
#28021=CARTESIAN_POINT('Ctrl Pts',(-0.208994544866511,0.00750001217157779,
0.0104310935790768));
#28022=CARTESIAN_POINT('',(-0.208879854976475,0.00591693841052602,0.0102914751265115));
#28023=CARTESIAN_POINT('Ctrl Pts',(-0.208994545029769,0.00750001033091269,
0.0104310935827688));
#28024=CARTESIAN_POINT('Ctrl Pts',(-0.208982707573584,0.0073658755916226,
0.0104308261979098));
#28025=CARTESIAN_POINT('Ctrl Pts',(-0.20896721346356,0.00718766232772565,
0.0104263173020414));
#28026=CARTESIAN_POINT('Ctrl Pts',(-0.208949780090682,0.00697958258322114,
0.0104155541122085));
#28027=CARTESIAN_POINT('Ctrl Pts',(-0.20894091519731,0.00687147249956225,
0.0104087427206195));
#28028=CARTESIAN_POINT('Ctrl Pts',(-0.208925870776048,0.00667848686935303,
0.0103933897413847));
#28029=CARTESIAN_POINT('Ctrl Pts',(-0.208910320714726,0.0064628834835101,
0.0103713923556962));
#28030=CARTESIAN_POINT('Ctrl Pts',(-0.20889540134221,0.00623562335293567,
0.0103432779976701));
#28031=CARTESIAN_POINT('Ctrl Pts',(-0.208884244471473,0.00601792720410426,
0.0103090504550555));
#28032=CARTESIAN_POINT('Ctrl Pts',(-0.208879854976475,0.00591693841052602,
0.0102914751265115));
#28033=CARTESIAN_POINT('',(-0.208080872472194,0.00591873554374485,0.0102739153516223));
#28034=CARTESIAN_POINT('Ctrl Pts',(-0.208879854469394,0.00591693448266163,
0.0102914978020838));
#28035=CARTESIAN_POINT('Ctrl Pts',(-0.208080871978074,0.005918730979702,
0.0102739417767417));
#28036=CARTESIAN_POINT('',(-0.208195607365079,0.0075000238688742,0.0104130369087551));
#28037=CARTESIAN_POINT('Ctrl Pts',(-0.208080872472194,0.00591873554374485,
0.0102739153516223));
#28038=CARTESIAN_POINT('Ctrl Pts',(-0.208085329775637,0.00601949218603198,
0.0102914009897838));
#28039=CARTESIAN_POINT('Ctrl Pts',(-0.208096663114823,0.00623761016686182,
0.0103256168419561));
#28040=CARTESIAN_POINT('Ctrl Pts',(-0.208111573860928,0.00646304574628812,
0.010353430237953));
#28041=CARTESIAN_POINT('Ctrl Pts',(-0.20812714033341,0.00667838970390981,
0.0103753803244538));
#28042=CARTESIAN_POINT('Ctrl Pts',(-0.208142186770862,0.00687138867708767,
0.0103907122427205));
#28043=CARTESIAN_POINT('Ctrl Pts',(-0.208150968215157,0.00697867959623386,
0.0103974668961326));
#28044=CARTESIAN_POINT('Ctrl Pts',(-0.20816833676301,0.00718664995486033,
0.0104082341148987));
#28045=CARTESIAN_POINT('Ctrl Pts',(-0.208183789388884,0.00736530067962771,
0.0104127701685665));
#28046=CARTESIAN_POINT('Ctrl Pts',(-0.208195607372227,0.00750002370009737,
0.0104130369160257));
#28047=CARTESIAN_POINT('',(-0.208294260069062,0.0123873539202809,0.00901864499536075));
#28048=CARTESIAN_POINT('Ctrl Pts',(-0.208195607357402,0.00750002386821102,
0.0104130369156901));
#28049=CARTESIAN_POINT('Ctrl Pts',(-0.208183725521012,0.00763476041676933,
0.0104127680247592));
#28050=CARTESIAN_POINT('Ctrl Pts',(-0.208173372346303,0.00775385061720008,
0.0104096649778735));
#28051=CARTESIAN_POINT('Ctrl Pts',(-0.208164101441032,0.00786286797816972,
0.0104051436089863));
#28052=CARTESIAN_POINT('Ctrl Pts',(-0.208159465986469,0.00791737668132509,
0.0104028829236024));
#28053=CARTESIAN_POINT('Ctrl Pts',(-0.208155102276373,0.00796936615530415,
0.0104002155912398));
#28054=CARTESIAN_POINT('Ctrl Pts',(-0.208151453172895,0.00801321643662261,
0.0103976814114876));
#28055=CARTESIAN_POINT('Ctrl Pts',(-0.208147804069418,0.00805706671794107,
0.0103951472317354));
#28056=CARTESIAN_POINT('Ctrl Pts',(-0.208144866645942,0.00809278446206585,
0.0103928758074853));
#28057=CARTESIAN_POINT('Ctrl Pts',(-0.208140874703066,0.00814285080404548,
0.0103892798192253));
#28058=CARTESIAN_POINT('Ctrl Pts',(-0.20813688276019,0.00819291714602511,
0.0103856838309653));
#28059=CARTESIAN_POINT('Ctrl Pts',(-0.20813184139307,0.00825731645169599,
0.0103805374635568));
#28060=CARTESIAN_POINT('Ctrl Pts',(-0.20812736863174,0.00831644241587525,
0.0103751771930394));
#28061=CARTESIAN_POINT('Ctrl Pts',(-0.208122895870409,0.00837556838005451,
0.010369816922522));
#28062=CARTESIAN_POINT('Ctrl Pts',(-0.208118988493735,0.00842943539830661,
0.0103643857681925));
#28063=CARTESIAN_POINT('Ctrl Pts',(-0.208115343387974,0.0084810693505092,
0.010358781032824));
#28064=CARTESIAN_POINT('Ctrl Pts',(-0.208108053176452,0.00858433725491439,
0.0103475715620869));
#28065=CARTESIAN_POINT('Ctrl Pts',(-0.208101808983563,0.00867867946861084,
0.010335803318858));
#28066=CARTESIAN_POINT('Ctrl Pts',(-0.208095735383128,0.00878341828696095,
0.0103209780293898));
#28067=CARTESIAN_POINT('Ctrl Pts',(-0.208089661782693,0.00888815710531106,
0.0103061527399216));
#28068=CARTESIAN_POINT('Ctrl Pts',(-0.208083767437249,0.00900324089728844,
0.0102878847212649));
#28069=CARTESIAN_POINT('Ctrl Pts',(-0.20807909837359,0.00911384130045568,
0.0102681932846837));
#28070=CARTESIAN_POINT('Ctrl Pts',(-0.208074429309932,0.00922444170362292,
0.0102485018481024));
#28071=CARTESIAN_POINT('Ctrl Pts',(-0.208070981091356,0.00933059943503606,
0.0102275861108202));
#28072=CARTESIAN_POINT('Ctrl Pts',(-0.208068438597206,0.00943425036157439,
0.0102053993543059));
#28073=CARTESIAN_POINT('Ctrl Pts',(-0.208063353608906,0.00964155221465106,
0.0101610258412775));
#28074=CARTESIAN_POINT('Ctrl Pts',(-0.208061883982439,0.00983886264689967,
0.0101119014126196));
#28075=CARTESIAN_POINT('Ctrl Pts',(-0.208065050743897,0.0100441495251014,
0.010053375551578));
#28076=CARTESIAN_POINT('Ctrl Pts',(-0.208068217505355,0.0102494364033031,
0.00999484969053644));
#28077=CARTESIAN_POINT('Ctrl Pts',(-0.208076042548387,0.0104624381000747,
0.00992593082114766));
#28078=CARTESIAN_POINT('Ctrl Pts',(-0.208088010578668,0.0106586113426422,
0.00985499861608774));
#28079=CARTESIAN_POINT('Ctrl Pts',(-0.208090192295864,0.0106943728277592,
0.00984206799944312));
#28080=CARTESIAN_POINT('Ctrl Pts',(-0.208092510941534,0.0107295822993813,
0.00982909116751217));
#28081=CARTESIAN_POINT('Ctrl Pts',(-0.208095002750416,0.0107647732770846,
0.00981587956169499));
#28082=CARTESIAN_POINT('Ctrl Pts',(-0.208099345476324,0.0108261041326129,
0.00979285436772329));
#28083=CARTESIAN_POINT('Ctrl Pts',(-0.208104214160172,0.0108873846775921,
0.00976912991166498));
#28084=CARTESIAN_POINT('Ctrl Pts',(-0.208109800610626,0.0109513663728325,
0.00974352101739119));
#28085=CARTESIAN_POINT('Ctrl Pts',(-0.208118592505577,0.0110520600687654,
0.00970321801817414));
#28086=CARTESIAN_POINT('Ctrl Pts',(-0.208129169253644,0.0111593388284774,
0.00965798950224713));
#28087=CARTESIAN_POINT('Ctrl Pts',(-0.208139623820843,0.0112560665917109,
0.00961521305913846));
#28088=CARTESIAN_POINT('Ctrl Pts',(-0.208150078388041,0.0113527943549444,
0.00957243661602978));
#28089=CARTESIAN_POINT('Ctrl Pts',(-0.208160402620197,0.0114391501065935,
0.00953249992055839));
#28090=CARTESIAN_POINT('Ctrl Pts',(-0.208172074236449,0.0115320013768258,
0.00948775271911064));
#28091=CARTESIAN_POINT('Ctrl Pts',(-0.208177910044575,0.0115784270119419,
0.00946537911838677));
#28092=CARTESIAN_POINT('Ctrl Pts',(-0.20818408319898,0.0116264619118133,
0.0094417780872376));
#28093=CARTESIAN_POINT('Ctrl Pts',(-0.208191106905069,0.0116791675793703,
0.00941522122005211));
#28094=CARTESIAN_POINT('Ctrl Pts',(-0.208198130611159,0.0117318732469273,
0.00938866435286662));
#28095=CARTESIAN_POINT('Ctrl Pts',(-0.208206007790269,0.011789180565019,
0.00935901134666794));
#28096=CARTESIAN_POINT('Ctrl Pts',(-0.208212011214235,0.0118321593655242,
0.00933634716649299));
#28097=CARTESIAN_POINT('Ctrl Pts',(-0.208218014638201,0.0118751381660294,
0.00931368298631804));
#28098=CARTESIAN_POINT('Ctrl Pts',(-0.208222139920884,0.0119039019332434,
0.00929822114678945));
#28099=CARTESIAN_POINT('Ctrl Pts',(-0.208227473863976,0.0119407908460249,
0.00927813875387184));
#28100=CARTESIAN_POINT('Ctrl Pts',(-0.208232807807067,0.0119776797588065,
0.00925805636095424));
#28101=CARTESIAN_POINT('Ctrl Pts',(-0.208239352863477,0.0120226273113437,
0.00923323308531815));
#28102=CARTESIAN_POINT('Ctrl Pts',(-0.208246336249947,0.0120699600589816,
0.00920647857997257));
#28103=CARTESIAN_POINT('Ctrl Pts',(-0.208260302981663,0.0121646252748504,
0.00915296972721423));
#28104=CARTESIAN_POINT('Ctrl Pts',(-0.208276018986776,0.0122689504658964,
0.0090919370770759));
#28105=CARTESIAN_POINT('Ctrl Pts',(-0.208294260069062,0.0123873539202809,
0.00901864499536075));
#28106=CARTESIAN_POINT('',(-0.207092313768591,0.0123882174867341,0.00899428887323861));
#28107=CARTESIAN_POINT('',(-0.208294260353821,0.0123873510979057,0.00901863812336346));
#28108=CARTESIAN_POINT('',(-0.206995158242226,0.00749997779533629,0.0103859057504772));
#28109=CARTESIAN_POINT('Ctrl Pts',(-0.20709231184162,0.012388216289393,
0.00899428645318913));
#28110=CARTESIAN_POINT('Ctrl Pts',(-0.207074169755397,0.0122704302801191,
0.0090670078806541));
#28111=CARTESIAN_POINT('Ctrl Pts',(-0.207050668983289,0.0121143816651057,
0.00915825300058597));
#28112=CARTESIAN_POINT('Ctrl Pts',(-0.207024508217981,0.0119342143511166,
0.00925742631421442));
#28113=CARTESIAN_POINT('Ctrl Pts',(-0.207011976852465,0.0118465431096515,
0.0093045210258247));
#28114=CARTESIAN_POINT('Ctrl Pts',(-0.206988525025257,0.0116750185140633,
0.00939315137049461));
#28115=CARTESIAN_POINT('Ctrl Pts',(-0.206963979310437,0.0114824390834477,
0.00948728155437886));
#28116=CARTESIAN_POINT('Ctrl Pts',(-0.206938206287943,0.0112645547797643,
0.00958813968390749));
#28117=CARTESIAN_POINT('Ctrl Pts',(-0.206907269851096,0.0109455825524754,
0.00972221310561395));
#28118=CARTESIAN_POINT('Ctrl Pts',(-0.206879687420821,0.0105673434823094,
0.00986567451972152));
#28119=CARTESIAN_POINT('Ctrl Pts',(-0.206860821301113,0.0100376767561021,
0.0100366007334439));
#28120=CARTESIAN_POINT('Ctrl Pts',(-0.206864629141656,0.00954303962447637,
0.0101588564587864));
#28121=CARTESIAN_POINT('Ctrl Pts',(-0.206878437662789,0.00911790159733215,
0.0102428688551869));
#28122=CARTESIAN_POINT('Ctrl Pts',(-0.206896112137639,0.00877089042089746,
0.0102976375929108));
#28123=CARTESIAN_POINT('Ctrl Pts',(-0.206911523653191,0.00853624604372451,
0.0103265108082205));
#28124=CARTESIAN_POINT('Ctrl Pts',(-0.206926997316845,0.00832094260799099,
0.0103483888826665));
#28125=CARTESIAN_POINT('Ctrl Pts',(-0.20694192568622,0.00812840320520952,
0.0103636459186607));
#28126=CARTESIAN_POINT('Ctrl Pts',(-0.206950766774903,0.00801985265443885,
0.010370459281196));
#28127=CARTESIAN_POINT('Ctrl Pts',(-0.206968077025284,0.0078118100493795,
0.0103811661821285));
#28128=CARTESIAN_POINT('Ctrl Pts',(-0.206983436288678,0.00763382030278916,
0.010385641149766));
#28129=CARTESIAN_POINT('Ctrl Pts',(-0.206995158242226,0.00749997779533629,
0.0103859057504772));
#28130=CARTESIAN_POINT('',(-0.206881571004172,0.00592143254235674,0.0102475607510614));
#28131=CARTESIAN_POINT('Ctrl Pts',(-0.206995158364972,0.00749997639380803,
0.0103859057532479));
#28132=CARTESIAN_POINT('Ctrl Pts',(-0.206983492947492,0.00736607084721818,
0.0103856417602202));
#28133=CARTESIAN_POINT('Ctrl Pts',(-0.206968200812035,0.00718792179638615,
0.0103811634468022));
#28134=CARTESIAN_POINT('Ctrl Pts',(-0.20695095010466,0.00697952724386687,
0.0103704294756607));
#28135=CARTESIAN_POINT('Ctrl Pts',(-0.206942127827325,0.00687066431350494,
0.0103635889922793));
#28136=CARTESIAN_POINT('Ctrl Pts',(-0.20692723590354,0.00667768022036194,
0.0103482739306657));
#28137=CARTESIAN_POINT('Ctrl Pts',(-0.206911792379283,0.00646186189337934,
0.0103263096445771));
#28138=CARTESIAN_POINT('Ctrl Pts',(-0.20689707330291,0.00623681443106316,
0.0102985550840657));
#28139=CARTESIAN_POINT('Ctrl Pts',(-0.206885945076055,0.00602074128867715,
0.0102647305309386));
#28140=CARTESIAN_POINT('Ctrl Pts',(-0.206881571004172,0.00592143254235674,
0.0102475607510614));
#28141=CARTESIAN_POINT('',(-0.206082602390132,0.00592322960732982,0.0102300014544386));
#28142=CARTESIAN_POINT('Ctrl Pts',(-0.206881570360281,0.00592142758673692,
0.0102475895477209));
#28143=CARTESIAN_POINT('Ctrl Pts',(-0.206082601797357,0.00592322405245955,
0.0102300338284272));
#28144=CARTESIAN_POINT('',(-0.206196245004281,0.00749992072476384,0.0103678496348724));
#28145=CARTESIAN_POINT('Ctrl Pts',(-0.206082602390132,0.00592322960732983,
0.0102300014544386));
#28146=CARTESIAN_POINT('Ctrl Pts',(-0.206087053038459,0.00602255130965301,
0.0102471249980864));
#28147=CARTESIAN_POINT('Ctrl Pts',(-0.206098374242025,0.00623937330301455,
0.0102809786338258));
#28148=CARTESIAN_POINT('Ctrl Pts',(-0.206113102929825,0.00646287265370996,
0.0103084456160293));
#28149=CARTESIAN_POINT('Ctrl Pts',(-0.206128560594177,0.00667833597196627,
0.0103303329190581));
#28150=CARTESIAN_POINT('Ctrl Pts',(-0.206143447710207,0.00687116699017132,
0.0103455994805507));
#28151=CARTESIAN_POINT('Ctrl Pts',(-0.206152184530551,0.00697912187521234,
0.010352371501617));
#28152=CARTESIAN_POINT('Ctrl Pts',(-0.206169362913561,0.00718720041427173,
0.0103630888895013));
#28153=CARTESIAN_POINT('Ctrl Pts',(-0.206184605677713,0.00736558647702679,
0.010367585415964));
#28154=CARTESIAN_POINT('Ctrl Pts',(-0.206196245007266,0.00749992065302299,
0.010367849635414));
#28155=CARTESIAN_POINT('',(-0.206293181463369,0.0123888250109843,0.00897808768959864));
#28156=CARTESIAN_POINT('Ctrl Pts',(-0.206196245001035,0.0074999207244816,
0.0103678496352738));
#28157=CARTESIAN_POINT('Ctrl Pts',(-0.206184542529965,0.00763412632884294,
0.0103675863081985));
#28158=CARTESIAN_POINT('Ctrl Pts',(-0.2061692179339,0.00781233643911382,
0.0103630995604675));
#28159=CARTESIAN_POINT('Ctrl Pts',(-0.206151946738275,0.00802024236853892,
0.0103524012407256));
#28160=CARTESIAN_POINT('Ctrl Pts',(-0.206143167389231,0.00812804320649983,
0.0103456471072809));
#28161=CARTESIAN_POINT('Ctrl Pts',(-0.206128189094492,0.00832091762604645,
0.0103303904006423));
#28162=CARTESIAN_POINT('Ctrl Pts',(-0.206112648998793,0.008536396951546,
0.0103085230622252));
#28163=CARTESIAN_POINT('Ctrl Pts',(-0.206097072443987,0.00877190099198238,
0.0102795657449935));
#28164=CARTESIAN_POINT('Ctrl Pts',(-0.206079161137434,0.00911884914045566,
0.0102248371881941));
#28165=CARTESIAN_POINT('Ctrl Pts',(-0.206065089571356,0.00954381660755296,
0.0101409002075465));
#28166=CARTESIAN_POINT('Ctrl Pts',(-0.206060937605528,0.010035297153322,
0.010019686043107));
#28167=CARTESIAN_POINT('Ctrl Pts',(-0.206079738162382,0.0105675848158489,
0.00984827657715455));
#28168=CARTESIAN_POINT('Ctrl Pts',(-0.206107422248231,0.0109458329710147,
0.00970501723280112));
#28169=CARTESIAN_POINT('Ctrl Pts',(-0.206138686284396,0.011266165094612,
0.00957054361039449));
#28170=CARTESIAN_POINT('Ctrl Pts',(-0.206164458349906,0.0114825743096787,
0.00947049134904797));
#28171=CARTESIAN_POINT('Ctrl Pts',(-0.206189095067363,0.0116749698665059,
0.00937663021818898));
#28172=CARTESIAN_POINT('Ctrl Pts',(-0.206212738063899,0.0118471644912719,
0.0092877970955207));
#28173=CARTESIAN_POINT('Ctrl Pts',(-0.206225078944011,0.0119332236759434,
0.00924164612878725));
#28174=CARTESIAN_POINT('Ctrl Pts',(-0.206251270428428,0.0121132674835715,
0.00914276021107132));
#28175=CARTESIAN_POINT('Ctrl Pts',(-0.206274891330583,0.0122700535809347,
0.00905129095501176));
#28176=CARTESIAN_POINT('Ctrl Pts',(-0.206293181463369,0.0123888250109843,
0.00897808768959864));
#28177=CARTESIAN_POINT('',(-0.205091194491485,0.0123896885085703,0.00895378586049373));
#28178=CARTESIAN_POINT('',(-0.206293181757635,0.0123888222119803,0.00897808071050165));
#28179=CARTESIAN_POINT('',(-0.204995827543056,0.00749981733645938,0.0103407191840654));
#28180=CARTESIAN_POINT('Ctrl Pts',(-0.205091192354661,0.012389687321618,
0.00895378339447929));
#28181=CARTESIAN_POINT('Ctrl Pts',(-0.205073014821144,0.01227160358044,
0.00902637100980068));
#28182=CARTESIAN_POINT('Ctrl Pts',(-0.205049485910908,0.0121152792329455,
0.00911737677581394));
#28183=CARTESIAN_POINT('Ctrl Pts',(-0.205023328523559,0.0119349871360469,
0.00921619202382797));
#28184=CARTESIAN_POINT('Ctrl Pts',(-0.205010838477898,0.0118475323830429,
0.00926297457286685));
#28185=CARTESIAN_POINT('Ctrl Pts',(-0.204987393403255,0.0116757713626103,
0.00935136047384095));
#28186=CARTESIAN_POINT('Ctrl Pts',(-0.204962913930657,0.0114831266914915,
0.00944514341353462));
#28187=CARTESIAN_POINT('Ctrl Pts',(-0.20493720267966,0.0112646364096667,
0.0095458509373571));
#28188=CARTESIAN_POINT('Ctrl Pts',(-0.204906741670358,0.0109473007740114,
0.00967875276225383));
#28189=CARTESIAN_POINT('Ctrl Pts',(-0.204879520873365,0.0105666748706983,
0.00982263833066586));
#28190=CARTESIAN_POINT('Ctrl Pts',(-0.204861373406722,0.0100372093631709,
0.00999271941458411));
#28191=CARTESIAN_POINT('Ctrl Pts',(-0.204865624696935,0.00954478680686117,
0.0101140694872304));
#28192=CARTESIAN_POINT('Ctrl Pts',(-0.204879700592637,0.00911920611846394,
0.0101979851582911));
#28193=CARTESIAN_POINT('Ctrl Pts',(-0.204897588310666,0.00877029818710369,
0.0102528656904525));
#28194=CARTESIAN_POINT('Ctrl Pts',(-0.204912941251136,0.00853620075514094,
0.0102815493069361));
#28195=CARTESIAN_POINT('Ctrl Pts',(-0.204928337381059,0.00832076733418454,
0.0103033614244297));
#28196=CARTESIAN_POINT('Ctrl Pts',(-0.204943136754122,0.00812836001515498,
0.0103185508067787));
#28197=CARTESIAN_POINT('Ctrl Pts',(-0.204951944478282,0.00801917500798704,
0.0103253762389851));
#28198=CARTESIAN_POINT('Ctrl Pts',(-0.204969092080602,0.00781102280142051,
0.0103360285986065));
#28199=CARTESIAN_POINT('Ctrl Pts',(-0.204984265519491,0.00763328673646041,
0.0103404605227132));
#28200=CARTESIAN_POINT('Ctrl Pts',(-0.204995827543056,0.00749981733645938,
0.0103407191840654));
#28201=CARTESIAN_POINT('',(-0.204883316991064,0.00592592657070326,0.0102036471645642));
#28202=CARTESIAN_POINT('Ctrl Pts',(-0.204995827641741,0.0074998161972604,
0.0103407191862731));
#28203=CARTESIAN_POINT('Ctrl Pts',(-0.204984332499912,0.00736625211880565,
0.0103404567187726));
#28204=CARTESIAN_POINT('Ctrl Pts',(-0.20496924147999,0.00718832573187981,
0.0103360137909475));
#28205=CARTESIAN_POINT('Ctrl Pts',(-0.204952174630355,0.00697980517123724,
0.0103253251092728));
#28206=CARTESIAN_POINT('Ctrl Pts',(-0.204943399499021,0.00687032365940605,
0.0103184693400497));
#28207=CARTESIAN_POINT('Ctrl Pts',(-0.204928658370534,0.00667745245189651,
0.0103032129340482));
#28208=CARTESIAN_POINT('Ctrl Pts',(-0.204913320512947,0.00646149678877712,
0.0102813055099391));
#28209=CARTESIAN_POINT('Ctrl Pts',(-0.20489879336288,0.00623853473943785,
0.0102539134026724));
#28210=CARTESIAN_POINT('Ctrl Pts',(-0.204887680136377,0.00602375668886092,
0.0102204500366935));
#28211=CARTESIAN_POINT('Ctrl Pts',(-0.204883316991064,0.00592592657070326,
0.0102036471645642));
#28212=CARTESIAN_POINT('',(-0.204084593180221,0.00592771653709633,0.0101861316274437));
#28213=CARTESIAN_POINT('Ctrl Pts',(-0.204883316213314,0.00592592062344288,
0.0102036819517157));
#28214=CARTESIAN_POINT('Ctrl Pts',(-0.204084593180221,0.00592771653709633,
0.0101861316274437));
#28215=CARTESIAN_POINT('',(-0.204196825282865,0.00749983108742957,0.0103226610633396));
#28216=CARTESIAN_POINT('Ctrl Pts',(-0.204084593180221,0.00592771653709633,
0.0101861316274437));
#28217=CARTESIAN_POINT('Ctrl Pts',(-0.204088954952523,0.00602549703428869,
0.0102029698422185));
#28218=CARTESIAN_POINT('Ctrl Pts',(-0.204093930289245,0.00612296943935068,
0.0102181387928113));
#28219=CARTESIAN_POINT('Ctrl Pts',(-0.204099344857712,0.00621696792384513,
0.0102313459157465));
#28220=CARTESIAN_POINT('Ctrl Pts',(-0.204105493253929,0.00632370587167922,
0.0102463429788));
#28221=CARTESIAN_POINT('Ctrl Pts',(-0.204112201386035,0.00642595904684314,
0.0102589347405499));
#28222=CARTESIAN_POINT('Ctrl Pts',(-0.204119539651985,0.00653093717501485,
0.0102701117909915));
#28223=CARTESIAN_POINT('Ctrl Pts',(-0.204123208784961,0.0065834262391007,
0.0102757003162123));
#28224=CARTESIAN_POINT('Ctrl Pts',(-0.204127036788764,0.00663660201222637,
0.0102808758285888));
#28225=CARTESIAN_POINT('Ctrl Pts',(-0.204130483044463,0.00668325954882323,
0.0102850760016559));
#28226=CARTESIAN_POINT('Ctrl Pts',(-0.204133929300162,0.00672991708542009,
0.0102892761747229));
#28227=CARTESIAN_POINT('Ctrl Pts',(-0.204136991852014,0.00677004892262425,
0.0102925877734305));
#28228=CARTESIAN_POINT('Ctrl Pts',(-0.204140414174299,0.00681404637568421,
0.0102959292212381));
#28229=CARTESIAN_POINT('Ctrl Pts',(-0.204154103461852,0.00699003616755132,
0.0103092950109213));
#28230=CARTESIAN_POINT('Ctrl Pts',(-0.204173571820494,0.00722794042724961,
0.0103221305265275));
#28231=CARTESIAN_POINT('Ctrl Pts',(-0.204196825280084,0.00749983108767882,
0.0103226610574747));
#28232=CARTESIAN_POINT('',(-0.204292038138456,0.0123902600478229,0.00893764321216362));
#28233=CARTESIAN_POINT('Ctrl Pts',(-0.20419682528816,0.00749983118210175,
0.010322661057659));
#28234=CARTESIAN_POINT('Ctrl Pts',(-0.204185287994438,0.00763376309286183,
0.0103224027582973));
#28235=CARTESIAN_POINT('Ctrl Pts',(-0.204170161862589,0.00781178846879767,
0.0103179525824367));
#28236=CARTESIAN_POINT('Ctrl Pts',(-0.204153078342857,0.00801977906802176,
0.010307304969565));
#28237=CARTESIAN_POINT('Ctrl Pts',(-0.204144357953895,0.00812805074055648,
0.0103005481704218));
#28238=CARTESIAN_POINT('Ctrl Pts',(-0.204129530124552,0.00832083172535136,
0.0102853561683061));
#28239=CARTESIAN_POINT('Ctrl Pts',(-0.204114093058388,0.00853643222207643,
0.0102635538200186));
#28240=CARTESIAN_POINT('Ctrl Pts',(-0.2040986064084,0.0087713093979552,
0.0102347984868405));
#28241=CARTESIAN_POINT('Ctrl Pts',(-0.204080485546677,0.00912046100820518,
0.0101799103396762));
#28242=CARTESIAN_POINT('Ctrl Pts',(-0.204066152296679,0.00954600523903629,
0.0100960102926049));
#28243=CARTESIAN_POINT('Ctrl Pts',(-0.204061486979092,0.0100343873479205,
0.00997597456805669));
#28244=CARTESIAN_POINT('Ctrl Pts',(-0.204079650090975,0.0105680873423369,
0.00980479049483992));
#28245=CARTESIAN_POINT('Ctrl Pts',(-0.204106639710054,0.010945641344127,
0.00966233015414049));
#28246=CARTESIAN_POINT('Ctrl Pts',(-0.204137681642606,0.0112667974884081,
0.00952805592914953));
#28247=CARTESIAN_POINT('Ctrl Pts',(-0.20416333123174,0.0114831919246611,
0.00942840223806717));
#28248=CARTESIAN_POINT('Ctrl Pts',(-0.204187914714008,0.0116757242786425,
0.00933486309581412));
#28249=CARTESIAN_POINT('Ctrl Pts',(-0.204211557237231,0.0118481462689717,
0.00924628149172132));
#28250=CARTESIAN_POINT('Ctrl Pts',(-0.204223858296622,0.0119339725206118,
0.00920044954244206));
#28251=CARTESIAN_POINT('Ctrl Pts',(-0.204250052390331,0.0121141295177386,
0.00910193095114931));
#28252=CARTESIAN_POINT('Ctrl Pts',(-0.204273707494313,0.0122711889090159,
0.00901070810291783));
#28253=CARTESIAN_POINT('Ctrl Pts',(-0.204292038138456,0.0123902600478229,
0.00893764321216362));
#28254=CARTESIAN_POINT('',(-0.203101390374644,0.0123905784886725,0.00891395760438764));
#28255=CARTESIAN_POINT('',(-0.204292038444341,0.0123902572194587,0.00893763603478656));
#28256=CARTESIAN_POINT('',(-0.203011370131853,0.00751797523340815,0.0102940321261883));
#28257=CARTESIAN_POINT('Ctrl Pts',(-0.203013533411654,0.00751781230923161,
0.0102959004892027));
#28258=CARTESIAN_POINT('Ctrl Pts',(-0.202890705906049,0.00853201876615493,
0.0102911689991259));
#28259=CARTESIAN_POINT('Ctrl Pts',(-0.20286207477571,0.00939893234967562,
0.010121503230433));
#28260=CARTESIAN_POINT('Ctrl Pts',(-0.202882497840241,0.0109708227094279,
0.00967762743988251));
#28261=CARTESIAN_POINT('Ctrl Pts',(-0.202987079475644,0.0117485829910666,
0.00930640625159674));
#28262=CARTESIAN_POINT('Ctrl Pts',(-0.203101360711969,0.0123898923172725,
0.00891437384716674));
#28263=CARTESIAN_POINT('',(-0.202885099445385,0.00593040690138148,0.0101598141695237));
#28264=CARTESIAN_POINT('Ctrl Pts',(-0.202996526590838,0.0074995785670763,
0.0102955332839449));
#28265=CARTESIAN_POINT('Ctrl Pts',(-0.202973024640025,0.00722307829876791,
0.0102949895048917));
#28266=CARTESIAN_POINT('Ctrl Pts',(-0.202943193857677,0.00685288796118912,
0.010275686682386));
#28267=CARTESIAN_POINT('Ctrl Pts',(-0.202918430663541,0.0065100870074686,
0.0102417504832254));
#28268=CARTESIAN_POINT('Ctrl Pts',(-0.202906519367261,0.00632809932186647,
0.0102195321989363));
#28269=CARTESIAN_POINT('Ctrl Pts',(-0.202900436007646,0.0062299981588559,
0.0102066417983168));
#28270=CARTESIAN_POINT('Ctrl Pts',(-0.20289118428028,0.0060609044627119,
0.0101816418860839));
#28271=CARTESIAN_POINT('Ctrl Pts',(-0.202886766832153,0.00596786024350971,
0.0101662602137973));
#28272=CARTESIAN_POINT('Ctrl Pts',(-0.202885099445385,0.00593040690138148,
0.0101598141695237));
#28273=CARTESIAN_POINT('',(-0.202086848594906,0.00593220842806255,0.0101422352280257));
#28274=CARTESIAN_POINT('Ctrl Pts',(-0.202885100231941,0.00593041357433423,
0.0101597751943222));
#28275=CARTESIAN_POINT('Ctrl Pts',(-0.202086848594906,0.00593220842806255,
0.0101422352280257));
#28276=CARTESIAN_POINT('',(-0.20219754174379,0.00749953411020732,0.0102774755667304));
#28277=CARTESIAN_POINT('Ctrl Pts',(-0.202086848594906,0.00593220842806255,
0.0101422352280257));
#28278=CARTESIAN_POINT('Ctrl Pts',(-0.202088519117636,0.00596903688538452,
0.0101485364647982));
#28279=CARTESIAN_POINT('Ctrl Pts',(-0.202090324455866,0.00600648645140127,
0.0101547274732126));
#28280=CARTESIAN_POINT('Ctrl Pts',(-0.202092356858527,0.00604614439339113,
0.0101610181868496));
#28281=CARTESIAN_POINT('Ctrl Pts',(-0.202095367721964,0.00610489488108823,
0.0101703374423528));
#28282=CARTESIAN_POINT('Ctrl Pts',(-0.202098880399795,0.00616851443157102,
0.0101797365089284));
#28283=CARTESIAN_POINT('Ctrl Pts',(-0.202101645600268,0.00621650288703459,
0.0101864571866253));
#28284=CARTESIAN_POINT('Ctrl Pts',(-0.20210441080074,0.00626449134249817,
0.0101931778643221));
#28285=CARTESIAN_POINT('Ctrl Pts',(-0.202106423626697,0.00629681902919462,
0.0101974383451088));
#28286=CARTESIAN_POINT('Ctrl Pts',(-0.202108915349507,0.00633570339411839,
0.0102023833567655));
#28287=CARTESIAN_POINT('Ctrl Pts',(-0.202111407072318,0.00637458775904215,
0.0102073283684222));
#28288=CARTESIAN_POINT('Ctrl Pts',(-0.202114380321182,0.00642004285894188,
0.0102128409478528));
#28289=CARTESIAN_POINT('Ctrl Pts',(-0.202117532890599,0.00646663661792655,
0.0102181065813405));
#28290=CARTESIAN_POINT('Ctrl Pts',(-0.202123838029432,0.00655982413589589,
0.0102286378483159));
#28291=CARTESIAN_POINT('Ctrl Pts',(-0.202130857195231,0.00665755250225107,
0.0102383258202183));
#28292=CARTESIAN_POINT('Ctrl Pts',(-0.202138811348339,0.00676382059618203,
0.010246936229931));
#28293=CARTESIAN_POINT('Ctrl Pts',(-0.202154719654555,0.00697635678404395,
0.0102641570493565));
#28294=CARTESIAN_POINT('Ctrl Pts',(-0.202174370848536,0.00722305320371844,
0.0102769379360553));
#28295=CARTESIAN_POINT('Ctrl Pts',(-0.202197541766043,0.00749953388485717,
0.0102774755490777));
#28296=CARTESIAN_POINT('',(-0.202290696343322,0.0123919560860567,0.00889712716492088));
#28297=CARTESIAN_POINT('Ctrl Pts',(-0.20219754174698,0.0074995341104433,
0.0102774755486583));
#28298=CARTESIAN_POINT('Ctrl Pts',(-0.202174197410107,0.00777578331222019,
0.0102769618592336));
#28299=CARTESIAN_POINT('Ctrl Pts',(-0.202154396477338,0.00802226572456519,
0.0102642230991678));
#28300=CARTESIAN_POINT('Ctrl Pts',(-0.202138363651234,0.00823461651089539,
0.010247050000429));
#28301=CARTESIAN_POINT('Ctrl Pts',(-0.202130347236,0.00834079193296164,
0.0102384634487223));
#28302=CARTESIAN_POINT('Ctrl Pts',(-0.20212327211763,0.00843843476446932,
0.0102288005419976));
#28303=CARTESIAN_POINT('Ctrl Pts',(-0.202116915784324,0.00853153325630933,
0.0102182965579286));
#28304=CARTESIAN_POINT('Ctrl Pts',(-0.20211373761767,0.00857808250222934,
0.0102130445658941));
#28305=CARTESIAN_POINT('Ctrl Pts',(-0.20211073995827,0.00862349223463621,
0.0102075463081249));
#28306=CARTESIAN_POINT('Ctrl Pts',(-0.202108227148492,0.00866234475445357,
0.0102026130993859));
#28307=CARTESIAN_POINT('Ctrl Pts',(-0.202105714338715,0.00870119727427093,
0.0101976798906468));
#28308=CARTESIAN_POINT('Ctrl Pts',(-0.20210368375886,0.0087335065640619,
0.0101934282692858));
#28309=CARTESIAN_POINT('Ctrl Pts',(-0.202100895377743,0.00878143132743709,
0.0101867267582064));
#28310=CARTESIAN_POINT('Ctrl Pts',(-0.202098106996625,0.00882935609081229,
0.0101800252471269));
#28311=CARTESIAN_POINT('Ctrl Pts',(-0.202094565690218,0.0088928668284534,
0.0101706566026742));
#28312=CARTESIAN_POINT('Ctrl Pts',(-0.202091528815688,0.00895153035166877,
0.0101613655220642));
#28313=CARTESIAN_POINT('Ctrl Pts',(-0.202088491941158,0.00901019387488415,
0.0101520744414542));
#28314=CARTESIAN_POINT('Ctrl Pts',(-0.20208595602052,0.00906403531818589,
0.0101430163228177));
#28315=CARTESIAN_POINT('Ctrl Pts',(-0.202083619010167,0.00911818415598467,
0.0101334511154132));
#28316=CARTESIAN_POINT('Ctrl Pts',(-0.202078944989461,0.00922648183158223,
0.0101143207006041));
#28317=CARTESIAN_POINT('Ctrl Pts',(-0.202075070817907,0.00933597511595025,
0.0100929735403107));
#28318=CARTESIAN_POINT('Ctrl Pts',(-0.202072169668726,0.00944105319838383,
0.0100706352896346));
#28319=CARTESIAN_POINT('Ctrl Pts',(-0.202066367370365,0.009651209363251,
0.0100259587882825));
#28320=CARTESIAN_POINT('Ctrl Pts',(-0.202064438475617,0.00984387915731189,
0.00997815759471386));
#28321=CARTESIAN_POINT('Ctrl Pts',(-0.202066752064248,0.0100445919900524,
0.00992154314919459));
#28322=CARTESIAN_POINT('Ctrl Pts',(-0.202069065652879,0.0102453048227928,
0.00986492870367532));
#28323=CARTESIAN_POINT('Ctrl Pts',(-0.202075638665163,0.0104538251381158,
0.00979872593742554));
#28324=CARTESIAN_POINT('Ctrl Pts',(-0.202087420101427,0.0106597907467386,
0.00972506974541213));
#28325=CARTESIAN_POINT('Ctrl Pts',(-0.202088936142116,0.0106862944968907,
0.00971559163242359));
#28326=CARTESIAN_POINT('Ctrl Pts',(-0.202090538475574,0.0107127579251253,
0.0097059932895129));
#28327=CARTESIAN_POINT('Ctrl Pts',(-0.20209222178385,0.0107391503167258,
0.00969628591170712));
#28328=CARTESIAN_POINT('Ctrl Pts',(-0.202103619779601,0.0109178581455779,
0.0096305554376458));
#28329=CARTESIAN_POINT('Ctrl Pts',(-0.202118730388031,0.011093231614691,
0.00955965491820764));
#28330=CARTESIAN_POINT('Ctrl Pts',(-0.202135902640255,0.0112563083096395,
0.00948841915018892));
#28331=CARTESIAN_POINT('Ctrl Pts',(-0.202145756804842,0.0113498886141496,
0.00944754105374905));
#28332=CARTESIAN_POINT('Ctrl Pts',(-0.202156286377539,0.0114394851745847,
0.00940669911095104));
#28333=CARTESIAN_POINT('Ctrl Pts',(-0.202167967182874,0.0115333353934138,
0.00936203130577747));
#28334=CARTESIAN_POINT('Ctrl Pts',(-0.202173807585541,0.0115802605028284,
0.00933969740319068));
#28335=CARTESIAN_POINT('Ctrl Pts',(-0.202179935730716,0.011628248451796,
0.00931640956649808));
#28336=CARTESIAN_POINT('Ctrl Pts',(-0.202186965540118,0.011681172702445,
0.00929007516233768));
#28337=CARTESIAN_POINT('Ctrl Pts',(-0.202193995349519,0.0117340969530941,
0.00926374075817729));
#28338=CARTESIAN_POINT('Ctrl Pts',(-0.202201929887158,0.0117918850794239,
0.00923421185299353));
#28339=CARTESIAN_POINT('Ctrl Pts',(-0.202207941287984,0.0118349233812734,
0.00921180059453036));
#28340=CARTESIAN_POINT('Ctrl Pts',(-0.202213952688811,0.0118779616831228,
0.00918938933606718));
#28341=CARTESIAN_POINT('Ctrl Pts',(-0.202218036500617,0.0119063646643708,
0.00917431357946753));
#28342=CARTESIAN_POINT('Ctrl Pts',(-0.20222336517733,0.0119431275555664,
0.00915455707647552));
#28343=CARTESIAN_POINT('Ctrl Pts',(-0.202228693854044,0.0119798904467619,
0.00913480057348351));
#28344=CARTESIAN_POINT('Ctrl Pts',(-0.202235269863326,0.0120249468234503,
0.00911024162445137));
#28345=CARTESIAN_POINT('Ctrl Pts',(-0.202242299009262,0.0120724598365375,
0.00908373556252275));
#28346=CARTESIAN_POINT('Ctrl Pts',(-0.202256357261165,0.0121674855925353,
0.0090307235893888));
#28347=CARTESIAN_POINT('Ctrl Pts',(-0.202272223951729,0.0122724580287967,
0.0089701285643458));
#28348=CARTESIAN_POINT('Ctrl Pts',(-0.202290696343322,0.0123919560860567,
0.00889712716492088));
#28349=CARTESIAN_POINT('',(-0.20108848344321,0.0123927133101065,0.00887232988670267));
#28350=CARTESIAN_POINT('',(-0.202290696630135,0.0123919530714235,0.0088971199712788));
#28351=CARTESIAN_POINT('',(-0.200997245792689,0.00749926539693365,0.0102503478276375));
#28352=CARTESIAN_POINT('Ctrl Pts',(-0.201088482311616,0.0123930036514002,
0.00887281699432422));
#28353=CARTESIAN_POINT('Ctrl Pts',(-0.201070199293268,0.0122742486992986,
0.00894517069201058));
#28354=CARTESIAN_POINT('Ctrl Pts',(-0.201054452846893,0.0121695861583328,
0.00900546027918073));
#28355=CARTESIAN_POINT('Ctrl Pts',(-0.201040476460977,0.0120745671878803,
0.0090583506901546));
#28356=CARTESIAN_POINT('Ctrl Pts',(-0.201033488268019,0.012027057702654,
0.00908479589564153));
#28357=CARTESIAN_POINT('Ctrl Pts',(-0.201026943578741,0.0119819301252515,
0.00910934169276158));
#28358=CARTESIAN_POINT('Ctrl Pts',(-0.201021605938962,0.0119448472291696,
0.0091292248705987));
#28359=CARTESIAN_POINT('Ctrl Pts',(-0.201016268299182,0.0119077643330876,
0.00914910804843582));
#28360=CARTESIAN_POINT('Ctrl Pts',(-0.201012135299618,0.0118787909044927,
0.0091644475674369));
#28361=CARTESIAN_POINT('Ctrl Pts',(-0.201006157019148,0.0118356171761458,
0.00918687265224561));
#28362=CARTESIAN_POINT('Ctrl Pts',(-0.201000178738679,0.0117924434477989,
0.00920929773705432));
#28363=CARTESIAN_POINT('Ctrl Pts',(-0.200992359495022,0.0117349585664124,
0.00923859690537065));
#28364=CARTESIAN_POINT('Ctrl Pts',(-0.200985418410638,0.0116821788340252,
0.00926479726236227));
#28365=CARTESIAN_POINT('Ctrl Pts',(-0.200978477326255,0.011629399101638,
0.00929099761935389));
#28366=CARTESIAN_POINT('Ctrl Pts',(-0.200972411446029,0.0115813942784893,
0.00931424197335796));
#28367=CARTESIAN_POINT('Ctrl Pts',(-0.200966628185391,0.0115343884230262,
0.00933656306557079));
#28368=CARTESIAN_POINT('Ctrl Pts',(-0.200955061664114,0.0114403767121,0.00938120524999644));
#28369=CARTESIAN_POINT('Ctrl Pts',(-0.200944625932499,0.0113503615239781,
0.00942214177493506));
#28370=CARTESIAN_POINT('Ctrl Pts',(-0.200934892884681,0.011256626007776,
0.00946298870578385));
#28371=CARTESIAN_POINT('Ctrl Pts',(-0.200917744065162,0.0110914718361288,
0.00953495759550671));
#28372=CARTESIAN_POINT('Ctrl Pts',(-0.200902786406862,0.0109145834168858,
0.00960623035823801));
#28373=CARTESIAN_POINT('Ctrl Pts',(-0.200891567611251,0.010734025306428,
0.00967236522966423));
#28374=CARTESIAN_POINT('Ctrl Pts',(-0.200890051644097,0.0107096269508223,
0.0096813018656697));
#28375=CARTESIAN_POINT('Ctrl Pts',(-0.200888603946429,0.0106851628805553,
0.00969014751367443));
#28376=CARTESIAN_POINT('Ctrl Pts',(-0.200887228336966,0.0106606542815155,
0.00969889424409479));
#28377=CARTESIAN_POINT('Ctrl Pts',(-0.200875672637934,0.0104547717241602,
0.00977237046460479));
#28378=CARTESIAN_POINT('Ctrl Pts',(-0.200869202538282,0.0102456202057633,
0.00983864844216689));
#28379=CARTESIAN_POINT('Ctrl Pts',(-0.200866946989291,0.0100445494558891,
0.00989523320289807));
#28380=CARTESIAN_POINT('Ctrl Pts',(-0.2008646914403,0.00984347870601498,
0.00995181796362925));
#28381=CARTESIAN_POINT('Ctrl Pts',(-0.200866632893402,0.00965072981297347,
0.00999951216075563));
#28382=CARTESIAN_POINT('Ctrl Pts',(-0.200872404140185,0.00944057932809876,
0.0100440752795689));
#28383=CARTESIAN_POINT('Ctrl Pts',(-0.200875289763577,0.0093355040856614,
0.0100663568389755));
#28384=CARTESIAN_POINT('Ctrl Pts',(-0.200879137516127,0.00922603513339181,
0.0100876453128725));
#28385=CARTESIAN_POINT('Ctrl Pts',(-0.200883778490859,0.00911775499283436,
0.0101067242803535));
#28386=CARTESIAN_POINT('Ctrl Pts',(-0.200886098978226,0.00906361492255562,
0.0101162637640941));
#28387=CARTESIAN_POINT('Ctrl Pts',(-0.200888616732779,0.00900978039076347,
0.0101252973592866));
#28388=CARTESIAN_POINT('Ctrl Pts',(-0.200891627110003,0.00895118991645648,
0.0101345536484139));
#28389=CARTESIAN_POINT('Ctrl Pts',(-0.200894637487227,0.00889259944214949,
0.0101438099375413));
#28390=CARTESIAN_POINT('Ctrl Pts',(-0.200898143906586,0.00882922837542473,
0.0101531361237415));
#28391=CARTESIAN_POINT('Ctrl Pts',(-0.200900916691685,0.00878122412212321,
0.0101598324166721));
#28392=CARTESIAN_POINT('Ctrl Pts',(-0.200903689476784,0.00873321986882169,
0.0101665287096026));
#28393=CARTESIAN_POINT('Ctrl Pts',(-0.20090572382208,0.00870061144149407,
0.0101708092296612));
#28394=CARTESIAN_POINT('Ctrl Pts',(-0.20090823384213,0.00866155148029748,
0.010175754140507));
#28395=CARTESIAN_POINT('Ctrl Pts',(-0.20091074386218,0.00862249151910088,
0.0101806990513527));
#28396=CARTESIAN_POINT('Ctrl Pts',(-0.200913732147395,0.00857696623911426,
0.0101861931125867));
#28397=CARTESIAN_POINT('Ctrl Pts',(-0.200916900703198,0.00853031734238165,
0.0101914382865752));
#28398=CARTESIAN_POINT('Ctrl Pts',(-0.200923237814804,0.00843701954891641,
0.0102019286345521));
#28399=CARTESIAN_POINT('Ctrl Pts',(-0.200930292809032,0.00833924075920457,
0.0102115654584951));
#28400=CARTESIAN_POINT('Ctrl Pts',(-0.200938283557203,0.00823304991383771,
0.010220115993609));
#28401=CARTESIAN_POINT('Ctrl Pts',(-0.200954265053545,0.00802066822310398,
0.0102372170638366));
#28402=CARTESIAN_POINT('Ctrl Pts',(-0.200973992485866,0.00777463695403748,
0.0102498441003304));
#28403=CARTESIAN_POINT('Ctrl Pts',(-0.200997245792689,0.00749926539693342,
0.0102503478276375));
#28404=CARTESIAN_POINT('',(-0.200887345683122,0.0059348980442802,0.0101159223609127));
#28405=CARTESIAN_POINT('Ctrl Pts',(-0.200997245792689,0.00749926539693344,
0.0102503478276375));
#28406=CARTESIAN_POINT('Ctrl Pts',(-0.200974220810078,0.00722377349386874,
0.0102498056169339));
#28407=CARTESIAN_POINT('Ctrl Pts',(-0.20094492337546,0.00685451096840348,
0.0102306958255404));
#28408=CARTESIAN_POINT('Ctrl Pts',(-0.200920472411397,0.0065119382581388,
0.0101969879151918));
#28409=CARTESIAN_POINT('Ctrl Pts',(-0.200908641045106,0.00632963709598595,
0.0101748447830745));
#28410=CARTESIAN_POINT('Ctrl Pts',(-0.200902595650718,0.0062316418888999,
0.0101620407673395));
#28411=CARTESIAN_POINT('Ctrl Pts',(-0.20089337088145,0.0060629478196754,
0.010137205831809));
#28412=CARTESIAN_POINT('Ctrl Pts',(-0.200888966074273,0.00597085304664883,
0.010122068388625));
#28413=CARTESIAN_POINT('Ctrl Pts',(-0.200887345683122,0.0059348980442802,
0.0101159223609127));
#28414=CARTESIAN_POINT('',(-0.200088157086456,0.00593670244816755,0.0100983180218859));
#28415=CARTESIAN_POINT('Ctrl Pts',(-0.200887346564016,0.00593490548572253,
0.0101158785953323));
#28416=CARTESIAN_POINT('Ctrl Pts',(-0.200088157086456,0.00593670244816755,
0.0100983180218859));
#28417=CARTESIAN_POINT('',(-0.200198400286692,0.00749894756480746,0.0102322932334285));
#28418=CARTESIAN_POINT('Ctrl Pts',(-0.200088157086456,0.00593670244816755,
0.0100983180218859));
#28419=CARTESIAN_POINT('Ctrl Pts',(-0.20008976368105,0.00597187626689402,
0.0101042966301346));
#28420=CARTESIAN_POINT('Ctrl Pts',(-0.200091496143024,0.0060076832085402,
0.0101101856171118));
#28421=CARTESIAN_POINT('Ctrl Pts',(-0.200093434362444,0.00604550028339444,
0.0101161648357467));
#28422=CARTESIAN_POINT('Ctrl Pts',(-0.200096446784859,0.00610427639652141,
0.0101254578662693));
#28423=CARTESIAN_POINT('Ctrl Pts',(-0.200099959719856,0.00616793036557959,
0.0101348314515784));
#28424=CARTESIAN_POINT('Ctrl Pts',(-0.200102723819808,0.00621593654063874,
0.0101415327659766));
#28425=CARTESIAN_POINT('Ctrl Pts',(-0.200105487919759,0.00626394271569789,
0.0101482340803749));
#28426=CARTESIAN_POINT('Ctrl Pts',(-0.200107498298591,0.00629627158481284,
0.0101524808478668));
#28427=CARTESIAN_POINT('Ctrl Pts',(-0.200109986693639,0.00633516002956199,
0.010157410421101));
#28428=CARTESIAN_POINT('Ctrl Pts',(-0.200112475088687,0.00637404847431113,
0.0101623399943352));
#28429=CARTESIAN_POINT('Ctrl Pts',(-0.200115444122225,0.00641951046982536,
0.0101678357074836));
#28430=CARTESIAN_POINT('Ctrl Pts',(-0.200118591478095,0.00646610918157705,
0.0101730851224447));
#28431=CARTESIAN_POINT('Ctrl Pts',(-0.200124886189833,0.00655930660508041,
0.0101835839523668));
#28432=CARTESIAN_POINT('Ctrl Pts',(-0.200131890944902,0.00665703718747477,
0.0101932416757067));
#28433=CARTESIAN_POINT('Ctrl Pts',(-0.200139826778877,0.0067633028814333,
0.0102018259719556));
#28434=CARTESIAN_POINT('Ctrl Pts',(-0.200155698446825,0.00697583426935033,
0.0102189945644533));
#28435=CARTESIAN_POINT('Ctrl Pts',(-0.200175297369914,0.00722250745150977,
0.0102317397242931));
#28436=CARTESIAN_POINT('Ctrl Pts',(-0.200198400307928,0.00749894710515932,
0.0102322932135127));
#28437=CARTESIAN_POINT('',(-0.200288451010882,0.0123939123990367,0.00885652921296301));
#28438=CARTESIAN_POINT('Ctrl Pts',(-0.200198400269183,0.00749894756328928,
0.0102322932126889));
#28439=CARTESIAN_POINT('Ctrl Pts',(-0.200175034204682,0.00777522439535255,
0.0102317964311445));
#28440=CARTESIAN_POINT('Ctrl Pts',(-0.200155209703933,0.00802173299218074,
0.0102191166516208));
#28441=CARTESIAN_POINT('Ctrl Pts',(-0.200139151983605,0.00823411531667132,
0.0102020146145068));
#28442=CARTESIAN_POINT('Ctrl Pts',(-0.200131123119003,0.008340306537613,
0.0101934635912232));
#28443=CARTESIAN_POINT('Ctrl Pts',(-0.200124035223245,0.00843796649754914,
0.0101838390983458));
#28444=CARTESIAN_POINT('Ctrl Pts',(-0.200117665261195,0.00853107942461829,
0.01017337629834));
#28445=CARTESIAN_POINT('Ctrl Pts',(-0.200114480280169,0.00857763588815286,
0.0101681448983371));
#28446=CARTESIAN_POINT('Ctrl Pts',(-0.200111475589978,0.00862305219430565,
0.0101626680823682));
#28447=CARTESIAN_POINT('Ctrl Pts',(-0.200108956259927,0.0086619155983258,
0.0101577533046134));
#28448=CARTESIAN_POINT('Ctrl Pts',(-0.200106436929877,0.00870077900234596,
0.0101528385268586));
#28449=CARTESIAN_POINT('Ctrl Pts',(-0.200104400351822,0.00873310336940028,
0.0101486018214236));
#28450=CARTESIAN_POINT('Ctrl Pts',(-0.200101603498619,0.00878102716460599,
0.0101419270521032));
#28451=CARTESIAN_POINT('Ctrl Pts',(-0.200098806645416,0.00882895095981169,
0.0101352522827829));
#28452=CARTESIAN_POINT('Ctrl Pts',(-0.200095254369762,0.00889244493919518,
0.0101259232194401));
#28453=CARTESIAN_POINT('Ctrl Pts',(-0.200092205971828,0.00895109935058674,
0.010116670426863));
#28454=CARTESIAN_POINT('Ctrl Pts',(-0.200089157573894,0.0090097537619783,
0.0101074176342858));
#28455=CARTESIAN_POINT('Ctrl Pts',(-0.200086609593287,0.00906359351686766,
0.0100983957483952));
#28456=CARTESIAN_POINT('Ctrl Pts',(-0.200084259375412,0.00911774172770745,
0.010088868514949));
#28457=CARTESIAN_POINT('Ctrl Pts',(-0.200079558939661,0.00922603814938702,
0.0100698140480564));
#28458=CARTESIAN_POINT('Ctrl Pts',(-0.200075653739693,0.0093355347325092,
0.0100485508013927));
#28459=CARTESIAN_POINT('Ctrl Pts',(-0.200072718973702,0.00944063469604749,
0.010026295922952));
#28460=CARTESIAN_POINT('Ctrl Pts',(-0.200066849441721,0.00965083462312407,
0.00998178616607069));
#28461=CARTESIAN_POINT('Ctrl Pts',(-0.200064843100723,0.00984362058227625,
0.00993414342631784));
#28462=CARTESIAN_POINT('Ctrl Pts',(-0.200067049334776,0.0100444089630219,
0.00987772837450729));
#28463=CARTESIAN_POINT('Ctrl Pts',(-0.200069255568829,0.0102451973437676,
0.00982131332269675));
#28464=CARTESIAN_POINT('Ctrl Pts',(-0.200075691166784,0.010453755471825,
0.00975535739903431));
#28465=CARTESIAN_POINT('Ctrl Pts',(-0.200087297015736,0.0106597933730671,
0.00968196917157241));
#28466=CARTESIAN_POINT('Ctrl Pts',(-0.200088628878771,0.0106834378531548,
0.00967354729155693));
#28467=CARTESIAN_POINT('Ctrl Pts',(-0.200090028868672,0.0107070506993985,
0.00966503005969394));
#28468=CARTESIAN_POINT('Ctrl Pts',(-0.200091493264414,0.0107306101771093,
0.00965642531582548));
#28469=CARTESIAN_POINT('Ctrl Pts',(-0.20010278960708,0.0109123478902808,
0.0095900483573769));
#28470=CARTESIAN_POINT('Ctrl Pts',(-0.200117918466425,0.0110908281621165,
0.0095182815256283));
#28471=CARTESIAN_POINT('Ctrl Pts',(-0.200135171791351,0.011256666011491,
0.00944614031450078));
#28472=CARTESIAN_POINT('Ctrl Pts',(-0.200144916766895,0.0113503340895811,
0.00940539371399374));
#28473=CARTESIAN_POINT('Ctrl Pts',(-0.200155336031474,0.0114400347331477,
0.00936467528287738));
#28474=CARTESIAN_POINT('Ctrl Pts',(-0.200166896763449,0.0115339917398713,
0.00932014468728363));
#28475=CARTESIAN_POINT('Ctrl Pts',(-0.200172677129437,0.0115809702432331,
0.00929787938948676));
#28476=CARTESIAN_POINT('Ctrl Pts',(-0.200178742796055,0.0116290122849527,
0.00927466360579343));
#28477=CARTESIAN_POINT('Ctrl Pts',(-0.200185701217565,0.0116819926846841,
0.00924841301065489));
#28478=CARTESIAN_POINT('Ctrl Pts',(-0.200192659639076,0.0117349730844156,
0.00922216241551634));
#28479=CARTESIAN_POINT('Ctrl Pts',(-0.200200513864588,0.0117928199715147,
0.00919272958044644));
#28480=CARTESIAN_POINT('Ctrl Pts',(-0.200206466983726,0.0118359189361975,
0.00917038274469422));
#28481=CARTESIAN_POINT('Ctrl Pts',(-0.200212420102864,0.0118790179008803,
0.00914803590894199));
#28482=CARTESIAN_POINT('Ctrl Pts',(-0.200216467684153,0.0119074826106276,
0.00913299227818158));
#28483=CARTESIAN_POINT('Ctrl Pts',(-0.200221747414023,0.0119443129647354,
0.00911328442399996));
#28484=CARTESIAN_POINT('Ctrl Pts',(-0.200227027143894,0.0119811433188431,
0.00909357656981834));
#28485=CARTESIAN_POINT('Ctrl Pts',(-0.200233541479317,0.0120262733482081,
0.00906908309913212));
#28486=CARTESIAN_POINT('Ctrl Pts',(-0.200240504920934,0.012073865662999,
0.00904264723468476));
#28487=CARTESIAN_POINT('Ctrl Pts',(-0.200254431765176,0.0121690500260711,
0.00898977565382692));
#28488=CARTESIAN_POINT('Ctrl Pts',(-0.200270150944277,0.0122742028687716,
0.00892933943482924));
#28489=CARTESIAN_POINT('Ctrl Pts',(-0.200288451010882,0.0123939123990367,
0.00885652921296301));
#28490=CARTESIAN_POINT('',(-0.19908556181331,0.0123952967315942,0.00883206936057618));
#28491=CARTESIAN_POINT('',(-0.20028845129905,0.0123939092169457,0.00885652174964775));
#28492=CARTESIAN_POINT('',(-0.198998259704992,0.0074982742183944,0.0102051689206332));
#28493=CARTESIAN_POINT('Ctrl Pts',(-0.199085562115416,0.0123952939201688,
0.00883206023608842));
#28494=CARTESIAN_POINT('Ctrl Pts',(-0.199067470452782,0.0122762676185759,
0.00890426489238289));
#28495=CARTESIAN_POINT('Ctrl Pts',(-0.199051890543392,0.0121713830788781,
0.00896442147583353));
#28496=CARTESIAN_POINT('Ctrl Pts',(-0.199038064980175,0.0120761788114213,
0.0090171873028811));
#28497=CARTESIAN_POINT('Ctrl Pts',(-0.199031152179298,0.012028576545002,
0.00904357028994718));
#28498=CARTESIAN_POINT('Ctrl Pts',(-0.199024678952974,0.0119833655290427,
0.00906805600834903));
#28499=CARTESIAN_POINT('Ctrl Pts',(-0.199019399757912,0.0119462147288482,
0.00908789030800503));
#28500=CARTESIAN_POINT('Ctrl Pts',(-0.19901412056285,0.0119090639286538,
0.00910772460766103));
#28501=CARTESIAN_POINT('Ctrl Pts',(-0.19901003299821,0.0118800377414823,
0.00912302625132981));
#28502=CARTESIAN_POINT('Ctrl Pts',(-0.199004123482984,0.0118367997345112,
0.00914538891032673));
#28503=CARTESIAN_POINT('Ctrl Pts',(-0.198998213967757,0.0117935617275401,
0.00916775156932366));
#28504=CARTESIAN_POINT('Ctrl Pts',(-0.198990486803648,0.0117360017473575,
0.00919696418540885));
#28505=CARTESIAN_POINT('Ctrl Pts',(-0.198983628961391,0.0116831543854901,
0.00922308703443275));
#28506=CARTESIAN_POINT('Ctrl Pts',(-0.198976771119134,0.0116303070236227,
0.00924920988345665));
#28507=CARTESIAN_POINT('Ctrl Pts',(-0.198970779654378,0.0115822415967694,
0.00927238546542428));
#28508=CARTESIAN_POINT('Ctrl Pts',(-0.198965068227769,0.0115351728563396,
0.00929464241602615));
#28509=CARTESIAN_POINT('Ctrl Pts',(-0.198953645374551,0.01144103537548,
0.00933915631722987));
#28510=CARTESIAN_POINT('Ctrl Pts',(-0.198943343001692,0.0113508848199434,
0.00937998227748156));
#28511=CARTESIAN_POINT('Ctrl Pts',(-0.198933748124436,0.011257069527313,
0.00942069391882997));
#28512=CARTESIAN_POINT('Ctrl Pts',(-0.198916567779573,0.0110890862339493,
0.00949359115551921));
#28513=CARTESIAN_POINT('Ctrl Pts',(-0.198901665630765,0.0109091651201766,
0.00956569424943081));
#28514=CARTESIAN_POINT('Ctrl Pts',(-0.198890623754789,0.0107254842476422,
0.00963250034361427));
#28515=CARTESIAN_POINT('Ctrl Pts',(-0.198889332299217,0.0107040009700714,
0.00964031397083064));
#28516=CARTESIAN_POINT('Ctrl Pts',(-0.198888093650609,0.0106824672530659,
0.00964805732130372));
#28517=CARTESIAN_POINT('Ctrl Pts',(-0.198886910340231,0.0106608970216631,
0.00965572517693894));
#28518=CARTESIAN_POINT('Ctrl Pts',(-0.198875609789499,0.0104549024671198,
0.00972895278754657));
#28519=CARTESIAN_POINT('Ctrl Pts',(-0.198869355171845,0.0102454484024135,
0.00979506721264478));
#28520=CARTESIAN_POINT('Ctrl Pts',(-0.198867277759337,0.0100442901244564,
0.0098514531584819));
#28521=CARTESIAN_POINT('Ctrl Pts',(-0.198865200346828,0.00984313184649926,
0.00990783910431903));
#28522=CARTESIAN_POINT('Ctrl Pts',(-0.198867282268461,0.00965051324536303,
0.00995531424483447));
#28523=CARTESIAN_POINT('Ctrl Pts',(-0.198873165980298,0.00944032859203435,
0.00999971204990802));
#28524=CARTESIAN_POINT('Ctrl Pts',(-0.198876107836217,0.00933523626537001,
0.0100219109524448));
#28525=CARTESIAN_POINT('Ctrl Pts',(-0.19888000485948,0.0092257090094105,
0.0100431284145762));
#28526=CARTESIAN_POINT('Ctrl Pts',(-0.19888468657262,0.00911736588760557,
0.0100621429764505));
#28527=CARTESIAN_POINT('Ctrl Pts',(-0.198887027429189,0.0090631943267031,
0.0100716502573876));
#28528=CARTESIAN_POINT('Ctrl Pts',(-0.198889563419655,0.00900932709267297,
0.0100806533178575));
#28529=CARTESIAN_POINT('Ctrl Pts',(-0.19889259098924,0.00895069447560245,
0.0100898787764111));
#28530=CARTESIAN_POINT('Ctrl Pts',(-0.198895618558826,0.00889206185853193,
0.0100991042349646));
#28531=CARTESIAN_POINT('Ctrl Pts',(-0.198899141120948,0.00882863935187035,
0.0101083995418997));
#28532=CARTESIAN_POINT('Ctrl Pts',(-0.198901924819502,0.00878059702204565,
0.0101150730859184));
#28533=CARTESIAN_POINT('Ctrl Pts',(-0.198904708518055,0.00873255469222094,
0.0101217466299372));
#28534=CARTESIAN_POINT('Ctrl Pts',(-0.198906748557306,0.00869992137052802,
0.0101260121169608));
#28535=CARTESIAN_POINT('Ctrl Pts',(-0.198909264339861,0.00866083550968477,
0.010130938969545));
#28536=CARTESIAN_POINT('Ctrl Pts',(-0.198911780122415,0.00862174964884151,
0.0101358658221292));
#28537=CARTESIAN_POINT('Ctrl Pts',(-0.198914774232609,0.00857619755678408,
0.0101413390608318));
#28538=CARTESIAN_POINT('Ctrl Pts',(-0.198917947386027,0.00852952442602086,
0.0101465635597709));
#28539=CARTESIAN_POINT('Ctrl Pts',(-0.198924293692863,0.00843617816449441,
0.010157012557649));
#28540=CARTESIAN_POINT('Ctrl Pts',(-0.198931352981443,0.00833836111898063,
0.0101666082468319));
#28541=CARTESIAN_POINT('Ctrl Pts',(-0.198939344055784,0.00823214024472807,
0.0101751192122635));
#28542=CARTESIAN_POINT('Ctrl Pts',(-0.198955326204467,0.00801969849622294,
0.0101921411431267));
#28543=CARTESIAN_POINT('Ctrl Pts',(-0.198975038419768,0.00777364006771175,
0.010204695155617));
#28544=CARTESIAN_POINT('Ctrl Pts',(-0.198998259704992,0.00749827421839462,
0.0102051689206332));
#28545=CARTESIAN_POINT('',(-0.198888606651639,0.00593939180859995,0.0100720065732061));
#28546=CARTESIAN_POINT('Ctrl Pts',(-0.198998259704992,0.00749827421839462,
0.0102051689206332));
#28547=CARTESIAN_POINT('Ctrl Pts',(-0.198975256733037,0.00722282626960612,
0.0102045979631378));
#28548=CARTESIAN_POINT('Ctrl Pts',(-0.198945979827808,0.00685361694055798,
0.0101855256812312));
#28549=CARTESIAN_POINT('Ctrl Pts',(-0.198921532147383,0.00651107764630125,
0.0101519141152692));
#28550=CARTESIAN_POINT('Ctrl Pts',(-0.198909695399112,0.00632878155323742,
0.0101298367493766));
#28551=CARTESIAN_POINT('Ctrl Pts',(-0.198903646060906,0.0062308013688519,
0.0101170734658568));
#28552=CARTESIAN_POINT('Ctrl Pts',(-0.198894518754158,0.00606415358536155,
0.010092615312019));
#28553=CARTESIAN_POINT('Ctrl Pts',(-0.198890163386274,0.00597361763698084,
0.0100778157362859));
#28554=CARTESIAN_POINT('Ctrl Pts',(-0.198888606651639,0.00593939180859995,
0.0100720065732061));
#28555=CARTESIAN_POINT('',(-0.198089410867419,0.00594119659128827,0.0100543996135915));
#28556=CARTESIAN_POINT('Ctrl Pts',(-0.198888607579108,0.00593939961257745,
0.0100719603459932));
#28557=CARTESIAN_POINT('Ctrl Pts',(-0.198089410867419,0.00594119659128827,
0.0100543996135915));
#28558=CARTESIAN_POINT('',(-0.198199413892123,0.00749784490164266,0.0101871142630232));
#28559=CARTESIAN_POINT('Ctrl Pts',(-0.198089410867419,0.00594119659128827,
0.0100543996135915));
#28560=CARTESIAN_POINT('Ctrl Pts',(-0.198090952098397,0.0059746271363879,
0.0100600442196936));
#28561=CARTESIAN_POINT('Ctrl Pts',(-0.198092609970194,0.0060086916375095,
0.0100656179332038));
#28562=CARTESIAN_POINT('Ctrl Pts',(-0.198094452783454,0.00604456647828324,
0.0100712724478378));
#28563=CARTESIAN_POINT('Ctrl Pts',(-0.198097472408025,0.00610335081255558,
0.0100805379071742));
#28564=CARTESIAN_POINT('Ctrl Pts',(-0.198100992073415,0.00616701774472966,
0.0100898846297762));
#28565=CARTESIAN_POINT('Ctrl Pts',(-0.198103760284483,0.00621502726683673,
0.0100965660669984));
#28566=CARTESIAN_POINT('Ctrl Pts',(-0.19810652849555,0.00626303678894381,
0.0101032475042207));
#28567=CARTESIAN_POINT('Ctrl Pts',(-0.198108540381426,0.00629535956821877,
0.0101074807298124));
#28568=CARTESIAN_POINT('Ctrl Pts',(-0.198111030365065,0.00633424346512967,
0.0101123951528504));
#28569=CARTESIAN_POINT('Ctrl Pts',(-0.198113520348705,0.00637312736204057,
0.0101173095758883));
#28570=CARTESIAN_POINT('Ctrl Pts',(-0.198116491043605,0.0064185862647321,
0.0101227889096156));
#28571=CARTESIAN_POINT('Ctrl Pts',(-0.198119639481253,0.00646518065693026,
0.0101280228980885));
#28572=CARTESIAN_POINT('Ctrl Pts',(-0.198125936356551,0.00655836944132657,
0.0101384908750344));
#28573=CARTESIAN_POINT('Ctrl Pts',(-0.198132940968095,0.00665608656171364,
0.010148121066479));
#28574=CARTESIAN_POINT('Ctrl Pts',(-0.198140874820444,0.00676233559324092,
0.010156683054696));
#28575=CARTESIAN_POINT('Ctrl Pts',(-0.198156742525141,0.00697483365629548,
0.0101738070311301));
#28576=CARTESIAN_POINT('Ctrl Pts',(-0.198176330129256,0.0072214607371163,
0.0101865286206563));
#28577=CARTESIAN_POINT('Ctrl Pts',(-0.198199413926082,0.00749784439333545,
0.010187114241221));
#28578=CARTESIAN_POINT('',(-0.198286007594511,0.0123960164106601,0.00881593489558765));
#28579=CARTESIAN_POINT('Ctrl Pts',(-0.198199413883263,0.00749784490085718,
0.0101871142403706));
#28580=CARTESIAN_POINT('Ctrl Pts',(-0.198176103477868,0.00777413486843259,
0.0101866512761317));
#28581=CARTESIAN_POINT('Ctrl Pts',(-0.198156318254055,0.00802067698994559,
0.0101740470863644));
#28582=CARTESIAN_POINT('Ctrl Pts',(-0.19814028359857,0.00823311616486342,
0.0101570274772293));
#28583=CARTESIAN_POINT('Ctrl Pts',(-0.198132266265918,0.00833933581736117,
0.0101485176674511));
#28584=CARTESIAN_POINT('Ctrl Pts',(-0.198125185849937,0.00843703003828308,
0.0101389360636091));
#28585=CARTESIAN_POINT('Ctrl Pts',(-0.198118819143145,0.00853018215640962,
0.0101285171408901));
#28586=CARTESIAN_POINT('Ctrl Pts',(-0.198115635789749,0.00857675821547287,
0.0101233076795306));
#28587=CARTESIAN_POINT('Ctrl Pts',(-0.198112631668245,0.00862219537792419,
0.0101178531725202));
#28588=CARTESIAN_POINT('Ctrl Pts',(-0.198110112092516,0.00866108138839014,
0.0101129574980669));
#28589=CARTESIAN_POINT('Ctrl Pts',(-0.198107592516787,0.00869996739885609,
0.0101080618236135));
#28590=CARTESIAN_POINT('Ctrl Pts',(-0.198105554887214,0.00873231601502186,
0.0101038406457708));
#28591=CARTESIAN_POINT('Ctrl Pts',(-0.198102755159942,0.0087802636455589,
0.0100971915835399));
#28592=CARTESIAN_POINT('Ctrl Pts',(-0.19809995543267,0.00882821127609593,
0.010090542521309));
#28593=CARTESIAN_POINT('Ctrl Pts',(-0.19809639844434,0.00889172889943068,
0.0100812500372814));
#28594=CARTESIAN_POINT('Ctrl Pts',(-0.198093343481625,0.00895040621919025,
0.0100720328458692));
#28595=CARTESIAN_POINT('Ctrl Pts',(-0.198090288518909,0.00900908353894982,
0.0100628156544569));
#28596=CARTESIAN_POINT('Ctrl Pts',(-0.198087732132926,0.00906294528084993,
0.0100538279006226));
#28597=CARTESIAN_POINT('Ctrl Pts',(-0.198085371573665,0.00911711565823163,
0.0100443363717712));
#28598=CARTESIAN_POINT('Ctrl Pts',(-0.198080650455144,0.00922545641299502,
0.0100253533140684));
#28599=CARTESIAN_POINT('Ctrl Pts',(-0.198076716817448,0.0093349982870547,
0.0100041682240223));
#28600=CARTESIAN_POINT('Ctrl Pts',(-0.198073747068821,0.00944013375262981,
0.0099819961171781));
#28601=CARTESIAN_POINT('Ctrl Pts',(-0.198067807571566,0.00965040468378001,
0.00993765190348967));
#28602=CARTESIAN_POINT('Ctrl Pts',(-0.198065705080381,0.00984322172765309,
0.00989019358358982));
#28603=CARTESIAN_POINT('Ctrl Pts',(-0.198067775303428,0.0100441274792667,
0.00983397148392325));
#28604=CARTESIAN_POINT('Ctrl Pts',(-0.198069845526475,0.0102450332308803,
0.00977774938425667));
#28605=CARTESIAN_POINT('Ctrl Pts',(-0.198076105322089,0.0104537951798029,
0.00971199140777644));
#28606=CARTESIAN_POINT('Ctrl Pts',(-0.198087491404007,0.0106599840281665,
0.00963884205248109));
#28607=CARTESIAN_POINT('Ctrl Pts',(-0.198088635894388,0.0106807094326789,
0.00963148932710166));
#28608=CARTESIAN_POINT('Ctrl Pts',(-0.198089832205802,0.0107014100382362,
0.00962406390124972));
#28609=CARTESIAN_POINT('Ctrl Pts',(-0.198091077878136,0.0107220713741063,
0.00961657095850853));
#28610=CARTESIAN_POINT('Ctrl Pts',(-0.198102224906933,0.0109069614930296,
0.00954951957890682));
#28611=CARTESIAN_POINT('Ctrl Pts',(-0.198117324635717,0.0110886212795307,
0.00947686846080482));
#28612=CARTESIAN_POINT('Ctrl Pts',(-0.198134614191499,0.0112572894281296,
0.00940379951023843));
#28613=CARTESIAN_POINT('Ctrl Pts',(-0.198144225017011,0.011351047773691,
0.00936318233400258));
#28614=CARTESIAN_POINT('Ctrl Pts',(-0.198154509073741,0.0114408574485988,
0.00932258431859022));
#28615=CARTESIAN_POINT('Ctrl Pts',(-0.19816592275737,0.0115349254228497,
0.00927818801413299));
#28616=CARTESIAN_POINT('Ctrl Pts',(-0.198171629599184,0.0115819594099751,
0.00925598986190438));
#28617=CARTESIAN_POINT('Ctrl Pts',(-0.198177618780531,0.0116300574555616,
0.00923284473727326));
#28618=CARTESIAN_POINT('Ctrl Pts',(-0.198184490318301,0.0116830979811874,
0.00920667541869562));
#28619=CARTESIAN_POINT('Ctrl Pts',(-0.198191361856072,0.0117361385068132,
0.00918050610011798));
#28620=CARTESIAN_POINT('Ctrl Pts',(-0.198199118785794,0.0117940501595618,
0.00915116559653516));
#28621=CARTESIAN_POINT('Ctrl Pts',(-0.198205000064564,0.0118372091942293,
0.00912888306599363));
#28622=CARTESIAN_POINT('Ctrl Pts',(-0.198210881343333,0.0118803682288967,
0.00910660053545211));
#28623=CARTESIAN_POINT('Ctrl Pts',(-0.198214882559401,0.0119088875112645,
0.00909159258929125));
#28624=CARTESIAN_POINT('Ctrl Pts',(-0.198220100259032,0.0119457768970234,
0.00907193770317756));
#28625=CARTESIAN_POINT('Ctrl Pts',(-0.198225317958663,0.0119826662827822,
0.00905228281706388));
#28626=CARTESIAN_POINT('Ctrl Pts',(-0.198231754588115,0.0120278602541438,
0.00902785990193314));
#28627=CARTESIAN_POINT('Ctrl Pts',(-0.198238634937554,0.0120755196795865,
0.0090015009955941));
#28628=CARTESIAN_POINT('Ctrl Pts',(-0.198252395597808,0.0121708382629281,
0.00894878333088588));
#28629=CARTESIAN_POINT('Ctrl Pts',(-0.198267927067132,0.0122761371757607,
0.00888852612430001));
#28630=CARTESIAN_POINT('Ctrl Pts',(-0.198286007594511,0.0123960164106601,
0.00881593489558765));
#28631=CARTESIAN_POINT('',(-0.197086979519691,0.0123971201193948,0.00879177325798805));
#28632=CARTESIAN_POINT('',(-0.198286007879611,0.0123960132910725,0.00881592749813436));
#28633=CARTESIAN_POINT('',(-0.196999270591198,0.00749728421803852,0.010159989841476));
#28634=CARTESIAN_POINT('Ctrl Pts',(-0.197086976737809,0.0123971189185158,
0.00879177056663458));
#28635=CARTESIAN_POINT('Ctrl Pts',(-0.197068794899013,0.0122778890515698,
0.00886376427758092));
#28636=CARTESIAN_POINT('Ctrl Pts',(-0.197045310518113,0.0121203981355003,
0.00895382276837131));
#28637=CARTESIAN_POINT('Ctrl Pts',(-0.19701930346749,0.0119393127272318,
0.00905133624140467));
#28638=CARTESIAN_POINT('Ctrl Pts',(-0.197006993671684,0.0118522429931005,
0.0090971191097409));
#28639=CARTESIAN_POINT('Ctrl Pts',(-0.19698370828621,0.0116794024840158,
0.00918453494617847));
#28640=CARTESIAN_POINT('Ctrl Pts',(-0.196959653037427,0.011486887794521,
0.00927674502930554));
#28641=CARTESIAN_POINT('Ctrl Pts',(-0.196923454455795,0.0111710535502845,
0.00941943933573583));
#28642=CARTESIAN_POINT('Ctrl Pts',(-0.196882607614813,0.0106654311014493,
0.00961961998668078));
#28643=CARTESIAN_POINT('Ctrl Pts',(-0.196864002095244,0.0100351435763335,
0.0098170164219494));
#28644=CARTESIAN_POINT('Ctrl Pts',(-0.196869375982058,0.00955457285278419,
0.00993489875212199));
#28645=CARTESIAN_POINT('Ctrl Pts',(-0.196883083155349,0.00917085742961943,
0.0100090632638723));
#28646=CARTESIAN_POINT('Ctrl Pts',(-0.196893255927463,0.00895513606961216,
0.010045064644907));
#28647=CARTESIAN_POINT('Ctrl Pts',(-0.196903850141088,0.00876446023912426,
0.0100728505475419));
#28648=CARTESIAN_POINT('Ctrl Pts',(-0.196909966763981,0.00866656949678343,
0.010085504284038));
#28649=CARTESIAN_POINT('Ctrl Pts',(-0.196921934611565,0.00848426778298676,
0.0101074108318155));
#28650=CARTESIAN_POINT('Ctrl Pts',(-0.19694660867882,0.00814179776041215,
0.0101407229405312));
#28651=CARTESIAN_POINT('Ctrl Pts',(-0.196976109231857,0.00777266281110438,
0.0101595464069006));
#28652=CARTESIAN_POINT('Ctrl Pts',(-0.196999270591198,0.00749728421803852,
0.010159989841476));
#28653=CARTESIAN_POINT('',(-0.196889861047832,0.00594388566779889,0.0100280902017948));
#28654=CARTESIAN_POINT('Ctrl Pts',(-0.196999270581664,0.00749728410378425,
0.0101599898412273));
#28655=CARTESIAN_POINT('Ctrl Pts',(-0.196976289970089,0.00722188673154521,
0.0101593904194489));
#28656=CARTESIAN_POINT('Ctrl Pts',(-0.196947033468888,0.00685273767299148,
0.0101403579352097));
#28657=CARTESIAN_POINT('Ctrl Pts',(-0.196922587915481,0.00651023541354164,
0.0101068459602804));
#28658=CARTESIAN_POINT('Ctrl Pts',(-0.196910744693017,0.00632794452775094,
0.0100848361630135));
#28659=CARTESIAN_POINT('Ctrl Pts',(-0.196904690767546,0.00622998027451274,
0.0100721147663665));
#28660=CARTESIAN_POINT('Ctrl Pts',(-0.196895659032348,0.00606536557185553,
0.0100480314473845));
#28661=CARTESIAN_POINT('Ctrl Pts',(-0.19689135334592,0.00597639027351646,
0.010033567696482));
#28662=CARTESIAN_POINT('Ctrl Pts',(-0.196889861047832,0.00594388566779889,
0.0100280902017948));
#28663=CARTESIAN_POINT('',(-0.196090558152439,0.0059456909738631,0.0100104788652639));
#28664=CARTESIAN_POINT('Ctrl Pts',(-0.196889862013759,0.00594389375422837,
0.0100280419520622));
#28665=CARTESIAN_POINT('Ctrl Pts',(-0.196090558152439,0.00594569097386311,
0.0100104788652639));
#28666=CARTESIAN_POINT('',(-0.196200534255837,0.00749682943752911,0.0101419375996538));
#28667=CARTESIAN_POINT('Ctrl Pts',(-0.196090558152439,0.0059456909738631,
0.0100104788652639));
#28668=CARTESIAN_POINT('Ctrl Pts',(-0.196092036966744,0.00597743019073511,
0.0100158019567583));
#28669=CARTESIAN_POINT('Ctrl Pts',(-0.196093623627043,0.00600979364775697,
0.0100210696180627));
#28670=CARTESIAN_POINT('Ctrl Pts',(-0.19609537642288,0.00604378231372989,
0.0100264093026737));
#28671=CARTESIAN_POINT('Ctrl Pts',(-0.196098407576924,0.00610255977097751,
0.0100356433539364));
#28672=CARTESIAN_POINT('Ctrl Pts',(-0.196101939030964,0.00616621904611668,
0.0100449588622492));
#28673=CARTESIAN_POINT('Ctrl Pts',(-0.196104715665148,0.00621422025408268,
0.0100516179388472));
#28674=CARTESIAN_POINT('Ctrl Pts',(-0.196107492299332,0.00626222146204868,
0.0100582770154452));
#28675=CARTESIAN_POINT('Ctrl Pts',(-0.196109509262426,0.00629453547881922,
0.0100624958862634));
#28676=CARTESIAN_POINT('Ctrl Pts',(-0.196112005272899,0.0063334107959747,
0.0100673940802161));
#28677=CARTESIAN_POINT('Ctrl Pts',(-0.196114501283371,0.00637228611313019,
0.0100722922741689));
#28678=CARTESIAN_POINT('Ctrl Pts',(-0.196117478944139,0.00641773652099083,
0.0100777539636736));
#28679=CARTESIAN_POINT('Ctrl Pts',(-0.196120634241672,0.00646432235999981,
0.0100829714859763));
#28680=CARTESIAN_POINT('Ctrl Pts',(-0.196126944836739,0.00655749403801779,
0.0100934065305818));
#28681=CARTESIAN_POINT('Ctrl Pts',(-0.196133962757214,0.00665519391160338,
0.010103007929413));
#28682=CARTESIAN_POINT('Ctrl Pts',(-0.196141910262291,0.00676142536250142,
0.0101115466471449));
#28683=CARTESIAN_POINT('Ctrl Pts',(-0.196157805269417,0.00697388822379259,
0.010128624079353));
#28684=CARTESIAN_POINT('Ctrl Pts',(-0.196177421541099,0.00722047876700838,
0.0101413216007707));
#28685=CARTESIAN_POINT('Ctrl Pts',(-0.196200534622597,0.00749682940687443,
0.0101419375907076));
#28686=CARTESIAN_POINT('',(-0.196289694237227,0.0123980179824918,0.00877562173246871));
#28687=CARTESIAN_POINT('Ctrl Pts',(-0.196200534635816,0.00749682956492873,
0.0101419375910599));
#28688=CARTESIAN_POINT('Ctrl Pts',(-0.196177276589334,0.00777317637202428,
0.0101415055483995));
#28689=CARTESIAN_POINT('Ctrl Pts',(-0.196157531423872,0.00801978727065713,
0.0101289709947919));
#28690=CARTESIAN_POINT('Ctrl Pts',(-0.196141525528564,0.00823228920837771,
0.0101120304784238));
#28691=CARTESIAN_POINT('Ctrl Pts',(-0.196133522580911,0.008338540177238,
0.0101035602202398));
#28692=CARTESIAN_POINT('Ctrl Pts',(-0.196126453718094,0.00843626423202327,
0.0100940208040487));
#28693=CARTESIAN_POINT('Ctrl Pts',(-0.196120094749083,0.00852946486601058,
0.0100836436364289));
#28694=CARTESIAN_POINT('Ctrl Pts',(-0.196116915264578,0.00857606518300422,
0.0100784550526191));
#28695=CARTESIAN_POINT('Ctrl Pts',(-0.196113914059311,0.00862153128516846,
0.0100730212605219));
#28696=CARTESIAN_POINT('Ctrl Pts',(-0.196111397802879,0.00866042255792442,
0.0100681464772229));
#28697=CARTESIAN_POINT('Ctrl Pts',(-0.196108881546448,0.00869931383068038,
0.010063271693924));
#28698=CARTESIAN_POINT('Ctrl Pts',(-0.196106847634349,0.00873164399457394,
0.0100590718101258));
#28699=CARTESIAN_POINT('Ctrl Pts',(-0.196104046485699,0.00877966529198083,
0.0100524412147516));
#28700=CARTESIAN_POINT('Ctrl Pts',(-0.196101245337049,0.00882768658938773,
0.0100458106193774));
#28701=CARTESIAN_POINT('Ctrl Pts',(-0.196097681806366,0.0088913700220046,
0.0100365329555621));
#28702=CARTESIAN_POINT('Ctrl Pts',(-0.196094621587336,0.00895016935677664,
0.0100273336378995));
#28703=CARTESIAN_POINT('Ctrl Pts',(-0.196091561368305,0.00900896869154867,
0.0100181343202368));
#28704=CARTESIAN_POINT('Ctrl Pts',(-0.196089000994026,0.00906290867838897,
0.0100091683225499));
#28705=CARTESIAN_POINT('Ctrl Pts',(-0.196086636460145,0.00911715513908172,
0.00999969989365157));
#28706=CARTESIAN_POINT('Ctrl Pts',(-0.196081907392384,0.00922564806046722,
0.00998076303585484));
#28707=CARTESIAN_POINT('Ctrl Pts',(-0.196077965906811,0.00933533335161433,
0.00995962741549134));
#28708=CARTESIAN_POINT('Ctrl Pts',(-0.196074985519283,0.00944047383056635,
0.0099375364402495));
#28709=CARTESIAN_POINT('Ctrl Pts',(-0.196069024744227,0.0096507547884704,
0.0098933544897658));
#28710=CARTESIAN_POINT('Ctrl Pts',(-0.196066889138433,0.00984303266291651,
0.00984621534378884));
#28711=CARTESIAN_POINT('Ctrl Pts',(-0.196068960891635,0.0100440889418934,
0.00979017784857315));
#28712=CARTESIAN_POINT('Ctrl Pts',(-0.196071032644837,0.0102451452208703,
0.00973414035335747));
#28713=CARTESIAN_POINT('Ctrl Pts',(-0.196077329814913,0.0104547341212989,
0.00966837753257755));
#28714=CARTESIAN_POINT('Ctrl Pts',(-0.196088794234009,0.0106610878249387,
0.00959544953614604));
#28715=CARTESIAN_POINT('Ctrl Pts',(-0.196089766942066,0.0106785960744598,
0.00958926190037273));
#28716=CARTESIAN_POINT('Ctrl Pts',(-0.196090776858213,0.0106960819662541,
0.00958302432059695));
#28717=CARTESIAN_POINT('Ctrl Pts',(-0.19609182253648,0.0107135375227711,
0.00957673971280791));
#28718=CARTESIAN_POINT('Ctrl Pts',(-0.196103101310356,0.0109018146257095,
0.00950895340381963));
#28719=CARTESIAN_POINT('Ctrl Pts',(-0.196118540635543,0.0110864784082488,
0.00943550685500762));
#28720=CARTESIAN_POINT('Ctrl Pts',(-0.196136326039856,0.0112581063636262,
0.00936147409591625));
#28721=CARTESIAN_POINT('Ctrl Pts',(-0.196146043202675,0.011351876331258,
0.00932102585187333));
#28722=CARTESIAN_POINT('Ctrl Pts',(-0.196156457446536,0.0114418177297387,
0.00928054563720497));
#28723=CARTESIAN_POINT('Ctrl Pts',(-0.196168015734873,0.0115359797763114,
0.00923629917301674));
#28724=CARTESIAN_POINT('Ctrl Pts',(-0.196173794879042,0.0115830607995978,
0.00921417594092263));
#28725=CARTESIAN_POINT('Ctrl Pts',(-0.196179859956068,0.0116311967773508,
0.00919111429181154));
#28726=CARTESIAN_POINT('Ctrl Pts',(-0.196186821829453,0.0116842943055095,
0.00916503255320362));
#28727=CARTESIAN_POINT('Ctrl Pts',(-0.196193783702839,0.0117373918336683,
0.00913895081459569));
#28728=CARTESIAN_POINT('Ctrl Pts',(-0.196201645404458,0.0117953798276383,
0.00910970194449075));
#28729=CARTESIAN_POINT('Ctrl Pts',(-0.196207602088749,0.011838565397306,
0.00908750520708496));
#28730=CARTESIAN_POINT('Ctrl Pts',(-0.196213558773039,0.0118817509669737,
0.00906530846967916));
#28731=CARTESIAN_POINT('Ctrl Pts',(-0.196217606038112,0.0119102464348559,
0.00905038037191789));
#28732=CARTESIAN_POINT('Ctrl Pts',(-0.196222889321542,0.0119471453490749,
0.00903080940373713));
#28733=CARTESIAN_POINT('Ctrl Pts',(-0.196228172604971,0.0119840442632939,
0.00901123843555637));
#28734=CARTESIAN_POINT('Ctrl Pts',(-0.196234694346225,0.0120292814575428,
0.00898690361769893));
#28735=CARTESIAN_POINT('Ctrl Pts',(-0.196241667116672,0.0120769974006122,
0.00896063422923547));
#28736=CARTESIAN_POINT('Ctrl Pts',(-0.196255612617835,0.0121724290148659,
0.00890809560199133));
#28737=CARTESIAN_POINT('Ctrl Pts',(-0.196271358170245,0.012277893677688,
0.00884802326661943));
#28738=CARTESIAN_POINT('Ctrl Pts',(-0.196289694237227,0.0123980179824918,
0.00877562173246871));
#28739=CARTESIAN_POINT('',(-0.195088692557014,0.012399858493754,0.00875103165054581));
#28740=CARTESIAN_POINT('',(-0.196289694536967,0.0123980145734612,0.00877561378979003));
#28741=CARTESIAN_POINT('',(-0.195000270973505,0.00749643710195729,0.0101148104777022));
#28742=CARTESIAN_POINT('Ctrl Pts',(-0.195088686761518,0.0123998593307978,
0.0087510315654015));
#28743=CARTESIAN_POINT('Ctrl Pts',(-0.195070524157984,0.012280426500865,
0.00882282829312997));
#28744=CARTESIAN_POINT('Ctrl Pts',(-0.195047066286106,0.0121226970251309,
0.00891262811377333));
#28745=CARTESIAN_POINT('Ctrl Pts',(-0.195021091927219,0.011941375725594,
0.00900984723560098));
#28746=CARTESIAN_POINT('Ctrl Pts',(-0.195008801086326,0.0118542212625203,
0.00905547838632326));
#28747=CARTESIAN_POINT('Ctrl Pts',(-0.19498554606785,0.011681164348149,
0.00914263187491693));
#28748=CARTESIAN_POINT('Ctrl Pts',(-0.194961527649185,0.0114884416080279,
0.00923455510442664));
#28749=CARTESIAN_POINT('Ctrl Pts',(-0.194925387021228,0.0111721758540357,
0.00937684361623232));
#28750=CARTESIAN_POINT('Ctrl Pts',(-0.19488468173109,0.0106667894376668,
0.00957614827161772));
#28751=CARTESIAN_POINT('Ctrl Pts',(-0.194866009785313,0.0100353625144586,
0.00977316795720429));
#28752=CARTESIAN_POINT('Ctrl Pts',(-0.194871255332421,0.00955436493404818,
0.0098906602441633));
#28753=CARTESIAN_POINT('Ctrl Pts',(-0.194884823298476,0.00917052629843446,
0.00996454232337369));
#28754=CARTESIAN_POINT('Ctrl Pts',(-0.194894908669353,0.00895478347064921,
0.010000396236686));
#28755=CARTESIAN_POINT('Ctrl Pts',(-0.194905417808874,0.00876415090922611,
0.0100280594449763));
#28756=CARTESIAN_POINT('Ctrl Pts',(-0.194911493249848,0.00866621227369239,
0.0100406662862808));
#28757=CARTESIAN_POINT('Ctrl Pts',(-0.194923381164897,0.0084838614482423,
0.010062484755121));
#28758=CARTESIAN_POINT('Ctrl Pts',(-0.194947903272857,0.00814125774315901,
0.0100956622885852));
#28759=CARTESIAN_POINT('Ctrl Pts',(-0.194977236161783,0.00777195597507231,
0.0101143944992188));
#28760=CARTESIAN_POINT('Ctrl Pts',(-0.195000270973505,0.00749643710195729,
0.0101148104777022));
#28761=CARTESIAN_POINT('',(-0.194890827700361,0.00594838029502342,0.00998416681136753));
#28762=CARTESIAN_POINT('Ctrl Pts',(-0.195000270970932,0.00749643707118917,
0.0101148104776324));
#28763=CARTESIAN_POINT('Ctrl Pts',(-0.194977245972861,0.00722106026275752,
0.0101141855185706));
#28764=CARTESIAN_POINT('Ctrl Pts',(-0.194947928951926,0.0068519599252208,
0.0100951947060793));
#28765=CARTESIAN_POINT('Ctrl Pts',(-0.194923425325342,0.00650953030717665,
0.0100617907603107));
#28766=CARTESIAN_POINT('Ctrl Pts',(-0.194911550293609,0.00632728904432808,
0.010039858086659));
#28767=CARTESIAN_POINT('Ctrl Pts',(-0.194905479264634,0.00622935798919421,
0.0100271829557886));
#28768=CARTESIAN_POINT('Ctrl Pts',(-0.194896524007881,0.00606673866737475,
0.010003472786475));
#28769=CARTESIAN_POINT('Ctrl Pts',(-0.194892260299988,0.00597926531552397,
0.00998933372937761));
#28770=CARTESIAN_POINT('Ctrl Pts',(-0.194890827700361,0.00594838029502342,
0.00998416681136753));
#28771=CARTESIAN_POINT('',(-0.194091473879223,0.00595018587709226,0.00996655302891216));
#28772=CARTESIAN_POINT('Ctrl Pts',(-0.194890828691577,0.00594838854289509,
0.00998411723525648));
#28773=CARTESIAN_POINT('Ctrl Pts',(-0.194091473879223,0.00595018587709227,
0.00996655302891217));
#28774=CARTESIAN_POINT('',(-0.194201348312574,0.00749635098887472,0.0100967541335085));
#28775=CARTESIAN_POINT('Ctrl Pts',(-0.194091473879223,0.00595018587709226,
0.00996655302891216));
#28776=CARTESIAN_POINT('Ctrl Pts',(-0.194092893260719,0.00598038565548873,
0.00997158348733984));
#28777=CARTESIAN_POINT('Ctrl Pts',(-0.1940944124127,0.0060111935220733,
0.00997657056587733));
#28778=CARTESIAN_POINT('Ctrl Pts',(-0.194096081351887,0.00604346677041894,
0.00998162208136269));
#28779=CARTESIAN_POINT('Ctrl Pts',(-0.194099120690989,0.00610224023943114,
0.00999082149896281));
#28780=CARTESIAN_POINT('Ctrl Pts',(-0.194102660243686,0.00616589483843443,
0.0100001022695497));
#28781=CARTESIAN_POINT('Ctrl Pts',(-0.194105442536318,0.00621389063753854,
0.0100067364108301));
#28782=CARTESIAN_POINT('Ctrl Pts',(-0.194108224828951,0.00626188643664265,
0.0100133705521104));
#28783=CARTESIAN_POINT('Ctrl Pts',(-0.194110245029893,0.00629419453290709,
0.0100175734425098));
#28784=CARTESIAN_POINT('Ctrl Pts',(-0.19411274481096,0.00633306407823682,
0.0100224533522769));
#28785=CARTESIAN_POINT('Ctrl Pts',(-0.194115244592027,0.00637193362356654,
0.010027333262044));
#28786=CARTESIAN_POINT('Ctrl Pts',(-0.19411822654559,0.0064173783039094,
0.0100327748217541));
#28787=CARTESIAN_POINT('Ctrl Pts',(-0.194121385941165,0.00646395830510856,
0.0100379733009625));
#28788=CARTESIAN_POINT('Ctrl Pts',(-0.194127704732313,0.00655711830750687,
0.0100483702593794));
#28789=CARTESIAN_POINT('Ctrl Pts',(-0.194134730082943,0.00665480616567737,
0.0100579373457575));
#28790=CARTESIAN_POINT('Ctrl Pts',(-0.194142684768261,0.00676102501734502,
0.0100664466792698));
#28791=CARTESIAN_POINT('Ctrl Pts',(-0.194158594136303,0.00697346268606376,
0.0100834653435213));
#28792=CARTESIAN_POINT('Ctrl Pts',(-0.194178223760992,0.00722002570874856,
0.0100961241872306));
#28793=CARTESIAN_POINT('Ctrl Pts',(-0.194201348677899,0.00749635095831825,
0.0100967541262211));
#28794=CARTESIAN_POINT('',(-0.194290135517151,0.0124010358448944,0.00873473146705155));
#28795=CARTESIAN_POINT('Ctrl Pts',(-0.194201348689204,0.00749635109339938,
0.010096754126529));
#28796=CARTESIAN_POINT('Ctrl Pts',(-0.19417839809719,0.00777274162232543,
0.0100963427415159));
#28797=CARTESIAN_POINT('Ctrl Pts',(-0.194158914654811,0.00801941390229902,
0.0100838710831682));
#28798=CARTESIAN_POINT('Ctrl Pts',(-0.194143121423411,0.00823199987814832,
0.0100670009474999));
#28799=CARTESIAN_POINT('Ctrl Pts',(-0.194135224807711,0.00833829286607297,
0.0100585658796657));
#28800=CARTESIAN_POINT('Ctrl Pts',(-0.194128250013288,0.00843606460448117,
0.0100490634695762));
#28801=CARTESIAN_POINT('Ctrl Pts',(-0.194121976173201,0.00852931596995155,
0.0100387245100895));
#28802=CARTESIAN_POINT('Ctrl Pts',(-0.194118839253157,0.00857594165268673,
0.0100335550303461));
#28803=CARTESIAN_POINT('Ctrl Pts',(-0.194115878374334,0.00862143390960432,
0.0100281407808191));
#28804=CARTESIAN_POINT('Ctrl Pts',(-0.194113395643768,0.00866035501257453,
0.0100232823451317));
#28805=CARTESIAN_POINT('Ctrl Pts',(-0.194110912913201,0.00869927611554473,
0.0100184239094444));
#28806=CARTESIAN_POINT('Ctrl Pts',(-0.194108905736036,0.00873163968044151,
0.0100142367594833));
#28807=CARTESIAN_POINT('Ctrl Pts',(-0.194106143178116,0.00877968609643283,
0.010007629394791));
#28808=CARTESIAN_POINT('Ctrl Pts',(-0.194103380620196,0.00882773251242415,
0.0100010220300988));
#28809=CARTESIAN_POINT('Ctrl Pts',(-0.194099867516978,0.00889143300494494,
0.00999177891797512));
#28810=CARTESIAN_POINT('Ctrl Pts',(-0.194096850970845,0.0089502520280375,
0.0099826130467189));
#28811=CARTESIAN_POINT('Ctrl Pts',(-0.194093834424713,0.00900907105113006,
0.00997344717546269));
#28812=CARTESIAN_POINT('Ctrl Pts',(-0.194091310982932,0.00906303316147349,
0.00996451291131835));
#28813=CARTESIAN_POINT('Ctrl Pts',(-0.194088981155853,0.00911730215254522,
0.00995507773633089));
#28814=CARTESIAN_POINT('Ctrl Pts',(-0.194084321501694,0.00922584013468866,
0.00993620738635599));
#28815=CARTESIAN_POINT('Ctrl Pts',(-0.19408044051176,0.00933557236943365,
0.00991514499932196));
#28816=CARTESIAN_POINT('Ctrl Pts',(-0.194077508702697,0.00944075777199428,
0.00989313016091075));
#28817=CARTESIAN_POINT('Ctrl Pts',(-0.194071645084572,0.00965112857711557,
0.00984910048408833));
#28818=CARTESIAN_POINT('Ctrl Pts',(-0.194069559001171,0.00984348716114984,
0.00980212389481556));
#28819=CARTESIAN_POINT('Ctrl Pts',(-0.194071632503713,0.0100446831425687,
0.00974626273392905));
#28820=CARTESIAN_POINT('Ctrl Pts',(-0.194073706006256,0.0102458791239875,
0.00969040157304254));
#28821=CARTESIAN_POINT('Ctrl Pts',(-0.194079957172833,0.0104556674988114,
0.0096248275184175));
#28822=CARTESIAN_POINT('Ctrl Pts',(-0.194091310588948,0.0106621736514585,
0.00955212697861027));
#28823=CARTESIAN_POINT('Ctrl Pts',(-0.194092096501302,0.0106764685328405,
0.00954709446224389));
#28824=CARTESIAN_POINT('Ctrl Pts',(-0.194092906868285,0.0106907483068779,
0.00954202890043225));
#28825=CARTESIAN_POINT('Ctrl Pts',(-0.194093740917631,0.0107050086814893,
0.00953693185123461));
#28826=CARTESIAN_POINT('Ctrl Pts',(-0.194104955679111,0.0108967559691738,
0.00946839610897852));
#28827=CARTESIAN_POINT('Ctrl Pts',(-0.194120452193851,0.0110849074006952,
0.00939396682608216));
#28828=CARTESIAN_POINT('Ctrl Pts',(-0.194138353045008,0.0112596343946404,
0.00931890116882885));
#28829=CARTESIAN_POINT('Ctrl Pts',(-0.19414796911975,0.0113534951735784,
0.00927857699852063));
#28830=CARTESIAN_POINT('Ctrl Pts',(-0.19415827580787,0.011443544814752,
0.00923821296413418));
#28831=CARTESIAN_POINT('Ctrl Pts',(-0.194169714563209,0.0115378191763271,
0.00919409524759436));
#28832=CARTESIAN_POINT('Ctrl Pts',(-0.194175433940879,0.0115849563571147,
0.00917203638932445));
#28833=CARTESIAN_POINT('Ctrl Pts',(-0.194181436256656,0.0116331495330089,
0.00914904227575429));
#28834=CARTESIAN_POINT('Ctrl Pts',(-0.19418832529866,0.0116863066725952,
0.00912303927144579));
#28835=CARTESIAN_POINT('Ctrl Pts',(-0.194195214340665,0.0117394638121814,
0.0090970362671373));
#28836=CARTESIAN_POINT('Ctrl Pts',(-0.194202993125362,0.0117975143746339,
0.0090678778462092));
#28837=CARTESIAN_POINT('Ctrl Pts',(-0.194208889351679,0.0118407646400332,
0.00904574078869874));
#28838=CARTESIAN_POINT('Ctrl Pts',(-0.194214785577995,0.0118840149054326,
0.00902360373118828));
#28839=CARTESIAN_POINT('Ctrl Pts',(-0.194218794866063,0.0119125763632006,
0.00900870385309618));
#28840=CARTESIAN_POINT('Ctrl Pts',(-0.194224025749138,0.0119495408514585,
0.00898918035970167));
#28841=CARTESIAN_POINT('Ctrl Pts',(-0.194229256632214,0.0119865053397165,
0.00896965686630715));
#28842=CARTESIAN_POINT('Ctrl Pts',(-0.194235711537924,0.0120318081568371,
0.00894538912837073));
#28843=CARTESIAN_POINT('Ctrl Pts',(-0.194242612268476,0.0120795910204617,
0.00891919414592734));
#28844=CARTESIAN_POINT('Ctrl Pts',(-0.194256413690112,0.012175156474426,
0.00886680433085772));
#28845=CARTESIAN_POINT('Ctrl Pts',(-0.194271994367652,0.0122807592863758,
0.00880690946492122));
#28846=CARTESIAN_POINT('Ctrl Pts',(-0.194290135517151,0.0124010358448944,
0.00873473146705154));
#28847=CARTESIAN_POINT('',(-0.193089361378644,0.0124020596755973,0.00871070447764098));
#28848=CARTESIAN_POINT('',(-0.194290135807019,0.0124010327218338,0.00873472395739432));
#28849=CARTESIAN_POINT('',(-0.193001273707137,0.00749669443297029,0.0100696315455101));
#28850=CARTESIAN_POINT('Ctrl Pts',(-0.193089358767972,0.0124020584333727,
0.00871070174821093));
#28851=CARTESIAN_POINT('Ctrl Pts',(-0.193071463321464,0.0122825687629352,
0.00878220102527336));
#28852=CARTESIAN_POINT('Ctrl Pts',(-0.193048338632269,0.0121247155490339,
0.00887166876060142));
#28853=CARTESIAN_POINT('Ctrl Pts',(-0.193022710464114,0.0119431553320592,
0.00896858691283708));
#28854=CARTESIAN_POINT('Ctrl Pts',(-0.193010556294765,0.0118556966153157,
0.00901417351058592));
#28855=CARTESIAN_POINT('Ctrl Pts',(-0.192987610729991,0.0116825316742599,
0.00910099721599476));
#28856=CARTESIAN_POINT('Ctrl Pts',(-0.192963877510663,0.0114895941408424,
0.00919262043208103));
#28857=CARTESIAN_POINT('Ctrl Pts',(-0.192928147068825,0.0111733485297158,
0.00933431543839347));
#28858=CARTESIAN_POINT('Ctrl Pts',(-0.192887506351826,0.010665479443791,
0.00953365685024814));
#28859=CARTESIAN_POINT('Ctrl Pts',(-0.192868616421275,0.0100366274996396,
0.00972901949957174));
#28860=CARTESIAN_POINT('Ctrl Pts',(-0.192873471399313,0.00955372558207172,
0.00984654890078579));
#28861=CARTESIAN_POINT('Ctrl Pts',(-0.192886770773999,0.00917022211560873,
0.00992002607284564));
#28862=CARTESIAN_POINT('Ctrl Pts',(-0.192896701545223,0.00895471565908591,
0.00995569170294781));
#28863=CARTESIAN_POINT('Ctrl Pts',(-0.192907068941763,0.00876450992109302,
0.00998318410436103));
#28864=CARTESIAN_POINT('Ctrl Pts',(-0.19291308785454,0.00866655446820109,
0.00999574754872156));
#28865=CARTESIAN_POINT('Ctrl Pts',(-0.192924866870832,0.00848429967818722,
0.0100174729609137));
#28866=CARTESIAN_POINT('Ctrl Pts',(-0.192949204804265,0.00814172016512548,
0.0100505317675662));
#28867=CARTESIAN_POINT('Ctrl Pts',(-0.192978361376715,0.00777233514591411,
0.0100692104249619));
#28868=CARTESIAN_POINT('Ctrl Pts',(-0.193001273707137,0.00749669443297029,
0.0100696315455101));
#28869=CARTESIAN_POINT('',(-0.192891760060441,0.00595287508888906,0.00994024214377629));
#28870=CARTESIAN_POINT('Ctrl Pts',(-0.193001273760643,0.00749669378927915,
0.0100696315464935));
#28871=CARTESIAN_POINT('Ctrl Pts',(-0.192978205734294,0.00722129220356709,
0.0100690135372334));
#28872=CARTESIAN_POINT('Ctrl Pts',(-0.192948829052146,0.00685217164030578,
0.0100501026422024));
#28873=CARTESIAN_POINT('Ctrl Pts',(-0.192924266441674,0.00650973865669913,
0.0100168357684943));
#28874=CARTESIAN_POINT('Ctrl Pts',(-0.192912358362987,0.00632750117293093,
0.00999499336760895));
#28875=CARTESIAN_POINT('Ctrl Pts',(-0.192906269413198,0.00622957857896456,
0.00998237122778532));
#28876=CARTESIAN_POINT('Ctrl Pts',(-0.192897372796077,0.00606860775490319,
0.0099589975389574));
#28877=CARTESIAN_POINT('Ctrl Pts',(-0.192893142125076,0.00598239332744973,
0.00994514452605578));
#28878=CARTESIAN_POINT('Ctrl Pts',(-0.192891760060441,0.00595287508888906,
0.00994024214377629));
#28879=CARTESIAN_POINT('',(-0.192094713079881,0.0059546755560343,0.0099226782462026));
#28880=CARTESIAN_POINT('Ctrl Pts',(-0.192891761067258,0.00595288340868952,
0.00994019176473061));
#28881=CARTESIAN_POINT('Ctrl Pts',(-0.192094713079881,0.00595467555603431,
0.00992267824620261));
#28882=CARTESIAN_POINT('',(-0.192177628746443,0.00719873229308102,0.0100462148679757));
#28883=CARTESIAN_POINT('Ctrl Pts',(-0.192177628746443,0.00719873229308102,
0.0100462148679757));
#28884=CARTESIAN_POINT('Ctrl Pts',(-0.192167980406568,0.00707953718124289,
0.01004222928847));
#28885=CARTESIAN_POINT('Ctrl Pts',(-0.192158471548071,0.00695723555078092,
0.0100358498652635));
#28886=CARTESIAN_POINT('Ctrl Pts',(-0.192149223388019,0.00683104810276648,
0.0100267199468337));
#28887=CARTESIAN_POINT('Ctrl Pts',(-0.192140662013969,0.0067142315752879,
0.0100182680335577));
#28888=CARTESIAN_POINT('Ctrl Pts',(-0.192132326398386,0.00659409211459482,
0.01000735549836));
#28889=CARTESIAN_POINT('Ctrl Pts',(-0.19212465062001,0.00647606086168701,
0.00999439458421457));
#28890=CARTESIAN_POINT('Ctrl Pts',(-0.192120812730822,0.0064170452352331,
0.00998791412714188));
#28891=CARTESIAN_POINT('Ctrl Pts',(-0.192117138346337,0.00635855104574488,
0.00998098610549107));
#28892=CARTESIAN_POINT('Ctrl Pts',(-0.192113265796624,0.00629325645586128,
0.00997255046049252));
#28893=CARTESIAN_POINT('Ctrl Pts',(-0.192109393246911,0.00622796186597769,
0.00996411481549397));
#28894=CARTESIAN_POINT('Ctrl Pts',(-0.192105328079181,0.00615589765055839,
0.00995392449603349));
#28895=CARTESIAN_POINT('Ctrl Pts',(-0.192102653944682,0.00610736421817033,
0.00994668951150614));
#28896=CARTESIAN_POINT('Ctrl Pts',(-0.192099979810182,0.00605883078578226,
0.0099394545269788));
#28897=CARTESIAN_POINT('Ctrl Pts',(-0.19209868952615,0.00603377873850918,
0.00993549588664673));
#28898=CARTESIAN_POINT('Ctrl Pts',(-0.192096922039073,0.00599881098332664,
0.00992987630703842));
#28899=CARTESIAN_POINT('Ctrl Pts',(-0.192096246446119,0.00598544513227643,
0.00992772831487772));
#28900=CARTESIAN_POINT('Ctrl Pts',(-0.19209550159305,0.00597063393719339,
0.00992531890744154));
#28901=CARTESIAN_POINT('Ctrl Pts',(-0.192094713079881,0.00595467555603429,
0.0099226782462026));
#28902=CARTESIAN_POINT('',(-0.192202394110733,0.00749688548776383,0.0100515763031989));
#28903=CARTESIAN_POINT('Ctrl Pts',(-0.19220250029781,0.00749685985592344,
0.0100515786483995));
#28904=CARTESIAN_POINT('Ctrl Pts',(-0.192194158548644,0.0073994198253338,
0.0100513576997749));
#28905=CARTESIAN_POINT('Ctrl Pts',(-0.192185843096806,0.00730020111470772,
0.010049657533291));
#28906=CARTESIAN_POINT('Ctrl Pts',(-0.192177628746443,0.00719873229308102,
0.0100462148679757));
#28907=CARTESIAN_POINT('',(-0.192248245628462,0.0121622160293808,0.00883352570391155));
#28908=CARTESIAN_POINT('Ctrl Pts',(-0.192202393318722,0.00749691043568044,
0.0100515762472776));
#28909=CARTESIAN_POINT('Ctrl Pts',(-0.192180228518616,0.0077593291150696,
0.0100511612228246));
#28910=CARTESIAN_POINT('Ctrl Pts',(-0.192161385886692,0.00799320657152351,
0.0100399281001668));
#28911=CARTESIAN_POINT('Ctrl Pts',(-0.19214608376665,0.00819447813377408,
0.01002481001183));
#28912=CARTESIAN_POINT('Ctrl Pts',(-0.19213843270663,0.00829511391489936,
0.0100172509676615));
#28913=CARTESIAN_POINT('Ctrl Pts',(-0.19213166614736,0.00838759844388116,
0.010008748362129));
#28914=CARTESIAN_POINT('Ctrl Pts',(-0.192125567626799,0.00847569269532253,
0.00999951868732737));
#28915=CARTESIAN_POINT('Ctrl Pts',(-0.192122518366519,0.00851973982104321,
0.00999490384992657));
#28916=CARTESIAN_POINT('Ctrl Pts',(-0.192119636826805,0.00856268658865227,
0.0099900756945606));
#28917=CARTESIAN_POINT('Ctrl Pts',(-0.19211721921592,0.00859941695979594,
0.00998574630260704));
#28918=CARTESIAN_POINT('Ctrl Pts',(-0.192114801605036,0.00863614733093961,
0.00998141691065349));
#28919=CARTESIAN_POINT('Ctrl Pts',(-0.192112845631441,0.00866667265043585,
0.00997768820603295));
#28920=CARTESIAN_POINT('Ctrl Pts',(-0.192110143911072,0.00871191896280949,
0.009971817222549));
#28921=CARTESIAN_POINT('Ctrl Pts',(-0.192107442190704,0.00875716527518314,
0.00996594623906505));
#28922=CARTESIAN_POINT('Ctrl Pts',(-0.192103998979885,0.00881710870440329,
0.00995774338022245));
#28923=CARTESIAN_POINT('Ctrl Pts',(-0.192101021701336,0.00887251825317918,
0.00994960527259644));
#28924=CARTESIAN_POINT('Ctrl Pts',(-0.192098044422788,0.00892792780195507,
0.00994146716497044));
#28925=CARTESIAN_POINT('Ctrl Pts',(-0.192095530045259,0.00897882377973813,
0.00993352920721947));
#28926=CARTESIAN_POINT('Ctrl Pts',(-0.192093186612127,0.00903002074062252,
0.00992514684629181));
#28927=CARTESIAN_POINT('Ctrl Pts',(-0.192088499745864,0.00913241466239132,
0.00990838212443648));
#28928=CARTESIAN_POINT('Ctrl Pts',(-0.192084500273023,0.00923598513733071,
0.0098896779208332));
#28929=CARTESIAN_POINT('Ctrl Pts',(-0.192081377795291,0.00933565028455126,
0.00987005703892966));
#28930=CARTESIAN_POINT('Ctrl Pts',(-0.192075132839828,0.00953498057899234,
0.00983081527512258));
#28931=CARTESIAN_POINT('Ctrl Pts',(-0.19207238078893,0.00971882360254878,
0.00978858457889742));
#28932=CARTESIAN_POINT('Ctrl Pts',(-0.192073205607948,0.00990902730152387,
0.00973897536808205));
#28933=CARTESIAN_POINT('Ctrl Pts',(-0.192074030426965,0.010099231000499,
0.00968936615726668));
#28934=CARTESIAN_POINT('Ctrl Pts',(-0.192078443750876,0.0102956373022703,
0.00963184480374686));
#28935=CARTESIAN_POINT('Ctrl Pts',(-0.19208744368846,0.010493041239175,
0.00956677871270986));
#28936=CARTESIAN_POINT('Ctrl Pts',(-0.192090542834519,0.0105610176698445,
0.00954437307736307));
#28937=CARTESIAN_POINT('Ctrl Pts',(-0.192094186834636,0.0106291184315858,
0.00952107554338757));
#28938=CARTESIAN_POINT('Ctrl Pts',(-0.192098268361286,0.0106964909770299,
0.00949717597011999));
#28939=CARTESIAN_POINT('Ctrl Pts',(-0.192106039610979,0.0108247686824003,
0.00945167104822796));
#28940=CARTESIAN_POINT('Ctrl Pts',(-0.192115396998233,0.0109503823502024,
0.00940393032371728));
#28941=CARTESIAN_POINT('Ctrl Pts',(-0.192125599697784,0.0110677442694379,
0.00935672263646901));
#28942=CARTESIAN_POINT('Ctrl Pts',(-0.192133380319991,0.0111572449697668,
0.00932072185276375));
#28943=CARTESIAN_POINT('Ctrl Pts',(-0.192141648232579,0.0112420070490703,
0.00928517282558984));
#28944=CARTESIAN_POINT('Ctrl Pts',(-0.192150895106228,0.0113318344768315,
0.00924587766023839));
#28945=CARTESIAN_POINT('Ctrl Pts',(-0.192155518543052,0.0113767481907121,
0.00922623007756266));
#28946=CARTESIAN_POINT('Ctrl Pts',(-0.192160386727942,0.0114229260324994,
0.00920564494416717));
#28947=CARTESIAN_POINT('Ctrl Pts',(-0.192166015780157,0.0114742829902484,
0.00918217302365252));
#28948=CARTESIAN_POINT('Ctrl Pts',(-0.192171644832372,0.0115256399479974,
0.00915870110313788));
#28949=CARTESIAN_POINT('Ctrl Pts',(-0.1921780377212,0.0115821118763141,
0.00913219959862655));
#28950=CARTESIAN_POINT('Ctrl Pts',(-0.192182785100559,0.0116233971300319,
0.00911246411289596));
#28951=CARTESIAN_POINT('Ctrl Pts',(-0.192187532479917,0.0116646823837497,
0.00909272862716538));
#28952=CARTESIAN_POINT('Ctrl Pts',(-0.192190630073563,0.0116908814352336,
0.00907996747514309));
#28953=CARTESIAN_POINT('Ctrl Pts',(-0.192194774678747,0.0117257245369188,
0.00906279949863401));
#28954=CARTESIAN_POINT('Ctrl Pts',(-0.192198919283931,0.0117605676386041,
0.00904563152212493));
#28955=CARTESIAN_POINT('Ctrl Pts',(-0.192204113235252,0.0118039975259787,
0.00902394217457035));
#28956=CARTESIAN_POINT('Ctrl Pts',(-0.192209681331023,0.0118500055934258,
0.00900043329314138));
#28957=CARTESIAN_POINT('Ctrl Pts',(-0.192220817465032,0.011942021252934,
0.00895341577319288));
#28958=CARTESIAN_POINT('Ctrl Pts',(-0.19223344616902,0.0120444558358653,
0.00889931899870446));
#28959=CARTESIAN_POINT('Ctrl Pts',(-0.192248245628462,0.0121622160293808,
0.00883352570391155));
#28960=CARTESIAN_POINT('',(-0.191554125307806,0.0118883026303221,0.00896741436455696));
#28961=CARTESIAN_POINT('Ctrl Pts',(-0.19224824585784,0.0121622178545567,
0.00883352468417506));
#28962=CARTESIAN_POINT('Ctrl Pts',(-0.192159518863803,0.0121296845027705,
0.00885002244467388));
#28963=CARTESIAN_POINT('Ctrl Pts',(-0.192051956961713,0.0120900338487957,
0.00886978569799122));
#28964=CARTESIAN_POINT('Ctrl Pts',(-0.191942470283334,0.0120490970867389,
0.00888990055962757));
#28965=CARTESIAN_POINT('Ctrl Pts',(-0.191911575843803,0.0120376351952446,
0.00889551572980783));
#28966=CARTESIAN_POINT('Ctrl Pts',(-0.191794878078659,0.0119925045909905,
0.00891747933582714));
#28967=CARTESIAN_POINT('Ctrl Pts',(-0.191680025579849,0.0119451674942562,
0.00894028684644732));
#28968=CARTESIAN_POINT('Ctrl Pts',(-0.191608665025318,0.0119142953286677,
0.0089550645765395));
#28969=CARTESIAN_POINT('Ctrl Pts',(-0.191554125307806,0.011888302630322,
0.00896741436455696));
#28970=CARTESIAN_POINT('',(-0.190961084118303,0.0114685865085303,0.00915978503157149));
#28971=CARTESIAN_POINT('Ctrl Pts',(-0.191554125307806,0.011888302630322,
0.00896741436455696));
#28972=CARTESIAN_POINT('Ctrl Pts',(-0.191553768718147,0.0118881326857775,
0.00896749510950585));
#28973=CARTESIAN_POINT('Ctrl Pts',(-0.191498468995547,0.0118617639595744,
0.00898002307501838));
#28974=CARTESIAN_POINT('Ctrl Pts',(-0.191373580637263,0.0117979333855556,
0.00901020026221204));
#28975=CARTESIAN_POINT('Ctrl Pts',(-0.191231902181779,0.0117097408939042,
0.00905123150723658));
#28976=CARTESIAN_POINT('Ctrl Pts',(-0.191109961893247,0.0116176746087238,
0.009093426564697));
#28977=CARTESIAN_POINT('Ctrl Pts',(-0.19101676606608,0.0115308722382138,
0.00913229805935754));
#28978=CARTESIAN_POINT('Ctrl Pts',(-0.19098601401332,0.0114982365429277,
0.0091467926911297));
#28979=CARTESIAN_POINT('Ctrl Pts',(-0.190959787032258,0.0114700741135794,
0.00915912665052349));
#28980=CARTESIAN_POINT('',(-0.191002065707968,0.00749708279836952,0.0100253807384898));
#28981=CARTESIAN_POINT('Ctrl Pts',(-0.19100206665356,0.0074971335629277,
0.0100244479210457));
#28982=CARTESIAN_POINT('Ctrl Pts',(-0.190986683760753,0.00767397789806786,
0.0100241538388789));
#28983=CARTESIAN_POINT('Ctrl Pts',(-0.190971218918847,0.00785819622901983,
0.0100189885523563));
#28984=CARTESIAN_POINT('Ctrl Pts',(-0.190956182171111,0.00805343011906291,
0.0100072581408944));
#28985=CARTESIAN_POINT('Ctrl Pts',(-0.190948663797244,0.00815104706408445,
0.0100013929351634));
#28986=CARTESIAN_POINT('Ctrl Pts',(-0.190941253875676,0.00825141510217649,
0.00999382328925438));
#28987=CARTESIAN_POINT('Ctrl Pts',(-0.190934286441721,0.00835059160622239,
0.00998476935492619));
#28988=CARTESIAN_POINT('Ctrl Pts',(-0.190930802724744,0.00840017985824532,
0.0099802423877621));
#28989=CARTESIAN_POINT('Ctrl Pts',(-0.190927428745033,0.00844947295853139,
0.00997538355317677));
#28990=CARTESIAN_POINT('Ctrl Pts',(-0.190923860389269,0.00850380681690841,
0.00996954702725766));
#28991=CARTESIAN_POINT('Ctrl Pts',(-0.190920292033504,0.00855814067528543,
0.00996371050133854));
#28992=CARTESIAN_POINT('Ctrl Pts',(-0.190916532851425,0.00861749920453185,
0.00995673852077294));
#28993=CARTESIAN_POINT('Ctrl Pts',(-0.190914005462433,0.0086580952751689,
0.00995171459185508));
#28994=CARTESIAN_POINT('Ctrl Pts',(-0.190911478073442,0.00869869134580596,
0.00994669066293722));
#28995=CARTESIAN_POINT('Ctrl Pts',(-0.190910177721542,0.00872055166708246,
0.00994382666834577));
#28996=CARTESIAN_POINT('Ctrl Pts',(-0.190908423243387,0.00875052923422294,
0.00993982342290933));
#28997=CARTESIAN_POINT('Ctrl Pts',(-0.190906668765231,0.00878050680136342,
0.00993582017747289));
#28998=CARTESIAN_POINT('Ctrl Pts',(-0.190904462326314,0.00881858795112804,
0.00993058103832489));
#28999=CARTESIAN_POINT('Ctrl Pts',(-0.190902180272689,0.00886036900673494,
0.00992451324510244));
#29000=CARTESIAN_POINT('Ctrl Pts',(-0.190897616165437,0.00894393111794873,
0.00991237765865754));
#29001=CARTESIAN_POINT('Ctrl Pts',(-0.190892753455369,0.00904227178739623,
0.00989675575918558));
#29002=CARTESIAN_POINT('Ctrl Pts',(-0.190888956462199,0.00913131048889955,
0.00988124033834146));
#29003=CARTESIAN_POINT('Ctrl Pts',(-0.19088515946903,0.00922034919040288,
0.00986572491749735));
#29004=CARTESIAN_POINT('Ctrl Pts',(-0.190882423438742,0.00930012282878565,
0.00985052905346753));
#29005=CARTESIAN_POINT('Ctrl Pts',(-0.190880507454492,0.00936698017388253,
0.00983717231909918));
#29006=CARTESIAN_POINT('Ctrl Pts',(-0.190878591470243,0.00943383751897941,
0.00982381558473084));
#29007=CARTESIAN_POINT('Ctrl Pts',(-0.190877495133955,0.00948778150108325,
0.00981231581913288));
#29008=CARTESIAN_POINT('Ctrl Pts',(-0.190876883399623,0.00952450165897181,
0.00980434732239747));
#29009=CARTESIAN_POINT('Ctrl Pts',(-0.190876271665291,0.00956122181686037,
0.00979637882566207));
#29010=CARTESIAN_POINT('Ctrl Pts',(-0.190876141741644,0.00958074470783384,
0.00979206747310957));
#29011=CARTESIAN_POINT('Ctrl Pts',(-0.190876061499207,0.00962245794566154,
0.00978257098913304));
#29012=CARTESIAN_POINT('Ctrl Pts',(-0.19087598125677,0.00966417118348925,
0.0097730745051565));
#29013=CARTESIAN_POINT('Ctrl Pts',(-0.190875954631328,0.00972803631233191,
0.00975821523746728));
#29014=CARTESIAN_POINT('Ctrl Pts',(-0.190876427965958,0.00980145036407707,
0.00974002553962839));
#29015=CARTESIAN_POINT('Ctrl Pts',(-0.190876901300588,0.00987486441582223,
0.00972183584178949));
#29016=CARTESIAN_POINT('Ctrl Pts',(-0.190877870777047,0.00995786507123561,
0.0097004880049227));
#29017=CARTESIAN_POINT('Ctrl Pts',(-0.190880285373099,0.0100602485747828,
0.00967209531717562));
#29018=CARTESIAN_POINT('Ctrl Pts',(-0.190882699969151,0.0101626320783299,
0.00964370262942855));
#29019=CARTESIAN_POINT('Ctrl Pts',(-0.190886570246384,0.0102842736444069,
0.00960778445427251));
#29020=CARTESIAN_POINT('Ctrl Pts',(-0.19089094525052,0.0103959644833041,
0.00957237684338193));
#29021=CARTESIAN_POINT('Ctrl Pts',(-0.19089510761836,0.0105022268642017,
0.00953869013216839));
#29022=CARTESIAN_POINT('Ctrl Pts',(-0.190899716336516,0.0105996034892998,
0.00950582546699569));
#29023=CARTESIAN_POINT('Ctrl Pts',(-0.190904641056022,0.0106913959610204,
0.00947339528464159));
#29024=CARTESIAN_POINT('Ctrl Pts',(-0.190910068938224,0.0107925669460626,
0.00943765168353396));
#29025=CARTESIAN_POINT('Ctrl Pts',(-0.190915880692719,0.0108869575165467,
0.00940243567738127));
#29026=CARTESIAN_POINT('Ctrl Pts',(-0.190921901795841,0.0109788179154417,
0.00936661769722615));
#29027=CARTESIAN_POINT('Ctrl Pts',(-0.190933385848026,0.0111540232878415,
0.00929830205057994));
#29028=CARTESIAN_POINT('Ctrl Pts',(-0.190945647941777,0.0113198121677733,
0.00922750758659213));
#29029=CARTESIAN_POINT('Ctrl Pts',(-0.190957452801276,0.0114675275550143,
0.00916024243452467));
#29030=CARTESIAN_POINT('',(-0.190890340272952,0.00595738356554221,0.00989621458805049));
#29031=CARTESIAN_POINT('Ctrl Pts',(-0.190890340272952,0.00595738356554221,
0.00989621458805049));
#29032=CARTESIAN_POINT('Ctrl Pts',(-0.190894915404536,0.00606113469594346,
0.0099132975649711));
#29033=CARTESIAN_POINT('Ctrl Pts',(-0.190900653165076,0.00616984093714869,
0.00992921711480411));
#29034=CARTESIAN_POINT('Ctrl Pts',(-0.190905948052378,0.00626017147666541,
0.00994117671185138));
#29035=CARTESIAN_POINT('Ctrl Pts',(-0.190908643320577,0.00630615263107193,
0.0099472645319996));
#29036=CARTESIAN_POINT('Ctrl Pts',(-0.190911222687648,0.00634736641256037,
0.00995237514057524));
#29037=CARTESIAN_POINT('Ctrl Pts',(-0.190913290364573,0.00637989510476361,
0.00995626995284936));
#29038=CARTESIAN_POINT('Ctrl Pts',(-0.190915358041499,0.00641242379696684,
0.00996016476512347));
#29039=CARTESIAN_POINT('Ctrl Pts',(-0.190916911969626,0.0064362557549028,
0.0099629355045932));
#29040=CARTESIAN_POINT('Ctrl Pts',(-0.190919652594268,0.0064763503677113,
0.00996732930590072));
#29041=CARTESIAN_POINT('Ctrl Pts',(-0.19092239321891,0.00651644498051981,
0.00997172310720824));
#29042=CARTESIAN_POINT('Ctrl Pts',(-0.190926324857418,0.00657282358380945,
0.00997754791989819));
#29043=CARTESIAN_POINT('Ctrl Pts',(-0.190930015220125,0.00662397847503081,
0.00998235767785981));
#29044=CARTESIAN_POINT('Ctrl Pts',(-0.190933705582833,0.00667513336625216,
0.00998716743582143));
#29045=CARTESIAN_POINT('Ctrl Pts',(-0.190937151568628,0.00672105240954706,
0.00999109980941678));
#29046=CARTESIAN_POINT('Ctrl Pts',(-0.190940660503065,0.00676673498668278,
0.0099947106672863));
#29047=CARTESIAN_POINT('Ctrl Pts',(-0.19094767837194,0.00685810014095424,
0.0100019323830254));
#29048=CARTESIAN_POINT('Ctrl Pts',(-0.19095495110437,0.0069485273983888,
0.0100077320996249));
#29049=CARTESIAN_POINT('Ctrl Pts',(-0.190962073245139,0.00703432837724492,
0.0100121057353759));
#29050=CARTESIAN_POINT('Ctrl Pts',(-0.190976316751223,0.00720592099300054,
0.0100208525306791));
#29051=CARTESIAN_POINT('Ctrl Pts',(-0.190989952613009,0.00735900406038744,
0.0100241318856088));
#29052=CARTESIAN_POINT('Ctrl Pts',(-0.191002105392592,0.00749710580794768,
0.01002444878813));
#29053=CARTESIAN_POINT('',(-0.186240951883218,0.00596786139892776,0.00979390672266723));
#29054=CARTESIAN_POINT('Ctrl Pts',(-0.190890340272952,0.00595738356554221,
0.00989621458805049));
#29055=CARTESIAN_POINT('Ctrl Pts',(-0.186240948602376,0.00596783763489472,
0.00979405360344712));
#29056=CARTESIAN_POINT('',(-0.186116972251352,0.00692238523863633,0.0098966261734716));
#29057=CARTESIAN_POINT('Ctrl Pts',(-0.186240951883218,0.00596786139892777,
0.00979390672266723));
#29058=CARTESIAN_POINT('Ctrl Pts',(-0.18618127827554,0.00628331776306349,
0.00984332128605338));
#29059=CARTESIAN_POINT('Ctrl Pts',(-0.186139877348579,0.00660240075550953,
0.00987785878236367));
#29060=CARTESIAN_POINT('Ctrl Pts',(-0.186117379209483,0.00692241345077483,
0.00989663789032303));
#29061=CARTESIAN_POINT('',(-0.186100495909817,0.00706118611434217,0.00990361595894344));
#29062=CARTESIAN_POINT('Ctrl Pts',(-0.186100495909817,0.00706118611434217,
0.00990361595894344));
#29063=CARTESIAN_POINT('Ctrl Pts',(-0.18610727117329,0.00701742533621366,
0.0099017649716299));
#29064=CARTESIAN_POINT('Ctrl Pts',(-0.186113922382522,0.00696643159218044,
0.00989921281268404));
#29065=CARTESIAN_POINT('Ctrl Pts',(-0.186116958514757,0.00692241191146765,
0.00989662830553491));
#29066=CARTESIAN_POINT('',(-0.185999364351488,0.00750000000238413,0.00991138348459431));
#29067=CARTESIAN_POINT('Ctrl Pts',(-0.18599946985063,0.00750001264944467,
0.00991138543689015));
#29068=CARTESIAN_POINT('Ctrl Pts',(-0.186001386963565,0.0074922177442551,
0.00991142880243267));
#29069=CARTESIAN_POINT('Ctrl Pts',(-0.186009183053014,0.00746314578508971,
0.00991164535693259));
#29070=CARTESIAN_POINT('Ctrl Pts',(-0.186021064239623,0.00741696715879665,
0.00991151314847068));
#29071=CARTESIAN_POINT('Ctrl Pts',(-0.18602700643212,0.00739387163006314,
0.00991144702644463));
#29072=CARTESIAN_POINT('Ctrl Pts',(-0.186033970262415,0.00736649702883345,
0.00991130192321211));
#29073=CARTESIAN_POINT('Ctrl Pts',(-0.186042754012062,0.00733038060627387,
0.0099108605130772));
#29074=CARTESIAN_POINT('Ctrl Pts',(-0.186051537761709,0.00729426418371429,
0.00991041910294229));
#29075=CARTESIAN_POINT('Ctrl Pts',(-0.186062143508568,0.00724940808696103,
0.00990958946141067));
#29076=CARTESIAN_POINT('Ctrl Pts',(-0.186070367192256,0.00721342297553624,
0.00990869861220074));
#29077=CARTESIAN_POINT('Ctrl Pts',(-0.186086814559632,0.00714145275268665,
0.00990691691378087));
#29078=CARTESIAN_POINT('Ctrl Pts',(-0.186093720646345,0.00710494689247067,
0.00990546694625697));
#29079=CARTESIAN_POINT('Ctrl Pts',(-0.186100495909817,0.00706118611434217,
0.00990361595894344));
#29080=CARTESIAN_POINT('',(-0.186096189557052,0.00791857507561077,0.00990442417341608));
#29081=CARTESIAN_POINT('Ctrl Pts',(-0.186096189557052,0.00791857507561077,
0.00990442417341608));
#29082=CARTESIAN_POINT('Ctrl Pts',(-0.18607770875607,0.00781175464853721,
0.00990892132930148));
#29083=CARTESIAN_POINT('Ctrl Pts',(-0.186046718548287,0.00767179620115901,
0.00991245356955209));
#29084=CARTESIAN_POINT('Ctrl Pts',(-0.185999469365137,0.00749998520788652,
0.00991138542591451));
#29085=CARTESIAN_POINT('',(-0.186116972833414,0.0080776147210469,0.0098966261914198));
#29086=CARTESIAN_POINT('Ctrl Pts',(-0.18611695911767,0.00807758801254939,
0.00989662832371766));
#29087=CARTESIAN_POINT('Ctrl Pts',(-0.186114180673599,0.00803730371254755,
0.0098989935180196));
#29088=CARTESIAN_POINT('Ctrl Pts',(-0.18610754762937,0.00798419117485202,
0.00990194617345709));
#29089=CARTESIAN_POINT('Ctrl Pts',(-0.186096189557052,0.00791857507561077,
0.00990442417341608));
#29090=CARTESIAN_POINT('',(-0.192768467995089,0.0155311216351573,0.0056536625113424));
#29091=CARTESIAN_POINT('Ctrl Pts',(-0.186117379209481,0.00807758654919004,
0.0098966378903251));
#29092=CARTESIAN_POINT('Ctrl Pts',(-0.186150545225195,0.00854933872546041,
0.00986895434783201));
#29093=CARTESIAN_POINT('Ctrl Pts',(-0.186261919503042,0.0092539535920186,
0.0097760582598693));
#29094=CARTESIAN_POINT('Ctrl Pts',(-0.186527601389658,0.0101614599702767,
0.00955792650929634));
#29095=CARTESIAN_POINT('Ctrl Pts',(-0.18679758954749,0.0108464676001627,
0.00933806715709752));
#29096=CARTESIAN_POINT('Ctrl Pts',(-0.187089763175687,0.011436922039813,
0.00910207381557108));
#29097=CARTESIAN_POINT('Ctrl Pts',(-0.187448533491602,0.0120332237854272,
0.00881682178178802));
#29098=CARTESIAN_POINT('Ctrl Pts',(-0.187826342609042,0.012557792726591,
0.00852178580869477));
#29099=CARTESIAN_POINT('Ctrl Pts',(-0.18840556546863,0.0132382397543376,
0.00808059549680021));
#29100=CARTESIAN_POINT('Ctrl Pts',(-0.189013583658982,0.0138007773072184,
0.00763500415641499));
#29101=CARTESIAN_POINT('Ctrl Pts',(-0.18972487030737,0.0143170911390719,
0.00715050345499707));
#29102=CARTESIAN_POINT('Ctrl Pts',(-0.190247984426023,0.0146379596486388,
0.0068153101803706));
#29103=CARTESIAN_POINT('Ctrl Pts',(-0.190863684275869,0.0149488034885615,
0.00645469056019629));
#29104=CARTESIAN_POINT('Ctrl Pts',(-0.191418393853279,0.0151762816431142,
0.0061643508478786));
#29105=CARTESIAN_POINT('Ctrl Pts',(-0.192123222073703,0.0153998088983173,
0.00585357929219802));
#29106=CARTESIAN_POINT('Ctrl Pts',(-0.19255235159128,0.015492619926808,
0.00571282248164196));
#29107=CARTESIAN_POINT('Ctrl Pts',(-0.192768462908894,0.0155311208402429,
0.00565366372878435));
#29108=CARTESIAN_POINT('',(-0.214999728175217,0.0156143085563526,0.00564621407322209));
#29109=CARTESIAN_POINT('Ctrl Pts',(-0.214999727535667,0.0156143027716101,
0.00564622516979127));
#29110=CARTESIAN_POINT('Ctrl Pts',(-0.20758929868895,0.0155894973834204,
0.00565023637807664));
#29111=CARTESIAN_POINT('Ctrl Pts',(-0.200178876390433,0.0155616813952821,
0.00565299213563701));
#29112=CARTESIAN_POINT('Ctrl Pts',(-0.192768468030038,0.015531113584314,
0.00565367517106059));
#29113=CARTESIAN_POINT('Ctrl Pts',(-0.214999728175217,0.0156143085563526,
0.00564621407322209));
#29114=CARTESIAN_POINT('Ctrl Pts',(-0.215340072574214,0.0156154113571772,
0.00564609976598468));
#29115=CARTESIAN_POINT('Ctrl Pts',(-0.215681165557661,0.0156337701167024,
0.00561327712279368));
#29116=CARTESIAN_POINT('Ctrl Pts',(-0.216016169200434,0.0156661766377763,
0.00555035271376907));
#29117=CARTESIAN_POINT('Ctrl Pts',(-0.216408346438714,0.0157041138370015,
0.00547668927313487));
#29118=CARTESIAN_POINT('Ctrl Pts',(-0.21679217849177,0.0157612870617016,
0.00536172046298686));
#29119=CARTESIAN_POINT('Ctrl Pts',(-0.217156694948461,0.0158297441906165,
0.00520865424064648));
#29120=CARTESIAN_POINT('Ctrl Pts',(-0.21783258679598,0.0159566784194797,
0.00492483656956197));
#29121=CARTESIAN_POINT('Ctrl Pts',(-0.21844207919684,0.0161219310071257,
0.00450934047096636));
#29122=CARTESIAN_POINT('Ctrl Pts',(-0.218954689895408,0.0162629602056725,
0.00399196702471092));
#29123=CARTESIAN_POINT('Ctrl Pts',(-0.219210995244691,0.0163334748049458,
0.00373328030158321));
#29124=CARTESIAN_POINT('Ctrl Pts',(-0.219443075431225,0.0163979734266596,
0.00344928409231887));
#29125=CARTESIAN_POINT('Ctrl Pts',(-0.219646842623798,0.01644956204799,
0.0031433958631618));
#29126=CARTESIAN_POINT('Ctrl Pts',(-0.219815132048998,0.0164921686095318,
0.00289076562563261));
#29127=CARTESIAN_POINT('Ctrl Pts',(-0.219964093926562,0.0165258943750711,
0.00262368966702913));
#29128=CARTESIAN_POINT('Ctrl Pts',(-0.220090794747946,0.0165472343306677,
0.00234431717574848));
#29129=CARTESIAN_POINT('Ctrl Pts',(-0.224903047769934,0.0163974953490442,
0.00232527569536224));
#29130=CARTESIAN_POINT('Ctrl Pts',(-0.228003678801843,0.0163652528946496,
0.00231821622721085));
#29131=CARTESIAN_POINT('Ctrl Pts',(-0.23110431006382,0.0163330357098684,
0.00231114482972889));
#29132=CARTESIAN_POINT('Ctrl Pts',(-0.234204941533998,0.0163008422866106,
0.00230405918705812));
#29133=CARTESIAN_POINT('Ctrl Pts',(-0.224902923051373,0.016421905903896,
0.001999690061282));
#29134=CARTESIAN_POINT('Ctrl Pts',(-0.228003554472057,0.0163857948128496,
0.00199154431614981));
#29135=CARTESIAN_POINT('Ctrl Pts',(-0.231104186130884,0.0163497065102629,
0.00198339075959686));
#29136=CARTESIAN_POINT('Ctrl Pts',(-0.23420481801057,0.0163136399270852,
0.00197522735965944));
#29137=CARTESIAN_POINT('Ctrl Pts',(-0.224902686634519,0.0164496060066283,
0.00134999605462854));
#29138=CARTESIAN_POINT('Ctrl Pts',(-0.228003316903349,0.0164061218898441,
0.00134119319572166));
#29139=CARTESIAN_POINT('Ctrl Pts',(-0.231103947348719,0.0163626446434222,
0.00133240817680761));
#29140=CARTESIAN_POINT('Ctrl Pts',(-0.234204577993315,0.0163191760221561,
0.00132364096404516));
#29141=CARTESIAN_POINT('Ctrl Pts',(-0.22490247733934,0.0164891827557564,
8.48946422705292E-5));
#29142=CARTESIAN_POINT('Ctrl Pts',(-0.2280031047451,0.0164387037966636,
8.36968421714054E-5));
#29143=CARTESIAN_POINT('Ctrl Pts',(-0.231103732057188,0.01638822192355,
8.25020821930779E-5));
#29144=CARTESIAN_POINT('Ctrl Pts',(-0.234204359262361,0.016337735996471,
8.13110569434896E-5));
#29145=CARTESIAN_POINT('Ctrl Pts',(-0.224902601832635,0.0164577305274795,
-0.00116946331798178));
#29146=CARTESIAN_POINT('Ctrl Pts',(-0.22800323228218,0.0164115731563456,
-0.00115947279336496));
#29147=CARTESIAN_POINT('Ctrl Pts',(-0.231103862912676,0.016365419418937,
-0.00114950763219157));
#29148=CARTESIAN_POINT('Ctrl Pts',(-0.234204493754791,0.0163192718567599,
-0.00113956819841304));
#29149=CARTESIAN_POINT('Ctrl Pts',(-0.2249031047193,0.016401050271707,-0.00247428944274167));
#29150=CARTESIAN_POINT('Ctrl Pts',(-0.228003735976318,0.016370691448232,
-0.00246735407024901));
#29151=CARTESIAN_POINT('Ctrl Pts',(-0.231104367476673,0.0163403620163895,
-0.00246039974613875));
#29152=CARTESIAN_POINT('Ctrl Pts',(-0.234204999188339,0.0163100597051565,
-0.00245342363871553));
#29153=CARTESIAN_POINT('Ctrl Pts',(-0.224903620482978,0.0162331344936927,
-0.00377581649114323));
#29154=CARTESIAN_POINT('Ctrl Pts',(-0.228004247053984,0.0162183248288798,
-0.00377611183675602));
#29155=CARTESIAN_POINT('Ctrl Pts',(-0.231104873706723,0.0162035348039987,
-0.00377640360674382));
#29156=CARTESIAN_POINT('Ctrl Pts',(-0.23420550044494,0.0161887639228305,
-0.00377669038870648));
#29157=CARTESIAN_POINT('Ctrl Pts',(-0.224904244439412,0.0157454055087051,
-0.00535508843351867));
#29158=CARTESIAN_POINT('Ctrl Pts',(-0.228004869356698,0.015745877431058,
-0.00536654194974573));
#29159=CARTESIAN_POINT('Ctrl Pts',(-0.231105494288016,0.0157463686608469,
-0.00537798949180189));
#29160=CARTESIAN_POINT('Ctrl Pts',(-0.234206119236561,0.0157468784277487,
-0.00538942975580705));
#29161=CARTESIAN_POINT('Ctrl Pts',(-0.224904927056323,0.014756116525245,
-0.0070809462510311));
#29162=CARTESIAN_POINT('Ctrl Pts',(-0.228005551277712,0.0147682738612367,
-0.00710847555851588));
#29163=CARTESIAN_POINT('Ctrl Pts',(-0.231106175457583,0.0147804448844733,
-0.00713600323790223));
#29164=CARTESIAN_POINT('Ctrl Pts',(-0.234206799604821,0.014792629252247,
-0.00716352865861212));
#29165=CARTESIAN_POINT('Ctrl Pts',(-0.224905705935764,0.0129587456084716,
-0.00904270204015799));
#29166=CARTESIAN_POINT('Ctrl Pts',(-0.228006331471737,0.0129775263446935,
-0.00909152831654588));
#29167=CARTESIAN_POINT('Ctrl Pts',(-0.231106956961612,0.0129963155259409,
-0.00914035417356039));
#29168=CARTESIAN_POINT('Ctrl Pts',(-0.234207582410669,0.0130151128918419,
-0.00918917939755658));
#29169=CARTESIAN_POINT('Ctrl Pts',(-0.224906344901157,0.00996717482975785,
-0.0106558172504251));
#29170=CARTESIAN_POINT('Ctrl Pts',(-0.228006973196984,0.00997888641244874,
-0.0107253416344494));
#29171=CARTESIAN_POINT('Ctrl Pts',(-0.23110760149003,0.00999060093234777,
-0.0107948661290257));
#29172=CARTESIAN_POINT('Ctrl Pts',(-0.234208229780548,0.0100023182636535,
-0.010864390745125));
#29173=CARTESIAN_POINT('Ctrl Pts',(-0.224906421473904,0.00588448586822914,
-0.0108495989887083));
#29174=CARTESIAN_POINT('Ctrl Pts',(-0.228007050197119,0.00587660352368733,
-0.0109217704181749));
#29175=CARTESIAN_POINT('Ctrl Pts',(-0.231107678925808,0.00586871925150363,
-0.0109939418074081));
#29176=CARTESIAN_POINT('Ctrl Pts',(-0.23420830765933,0.00586083314294305,
-0.0110661131658069));
#29177=CARTESIAN_POINT('Ctrl Pts',(-0.224905896797368,0.00275206275993148,
-0.00952499259309634));
#29178=CARTESIAN_POINT('Ctrl Pts',(-0.22800652301585,0.00273399542249794,
-0.00957977151548));
#29179=CARTESIAN_POINT('Ctrl Pts',(-0.231107149196805,0.00271592133715538,
-0.00963455045765119));
#29180=CARTESIAN_POINT('Ctrl Pts',(-0.234207775344483,0.00269784071003669,
-0.00968932931015458));
#29181=CARTESIAN_POINT('Ctrl Pts',(-0.224905188461513,0.000775386387695849,
-0.00774097724716007));
#29182=CARTESIAN_POINT('Ctrl Pts',(-0.228005812987761,0.000760338332521188,
-0.0077754138708565));
#29183=CARTESIAN_POINT('Ctrl Pts',(-0.231106437467874,0.000745278047377309,
-0.00780984908461508));
#29184=CARTESIAN_POINT('Ctrl Pts',(-0.234207061909447,0.000730205873823641,
-0.00784428237662763));
#29185=CARTESIAN_POINT('Ctrl Pts',(-0.224904545212544,-0.00037433699893992,
-0.00611286595312136));
#29186=CARTESIAN_POINT('Ctrl Pts',(-0.228005169500613,-0.000380655003703386,
-0.00613103039787742));
#29187=CARTESIAN_POINT('Ctrl Pts',(-0.231105793767721,-0.000386989095479687,
-0.00614919200572512));
#29188=CARTESIAN_POINT('Ctrl Pts',(-0.234206418022201,-0.000393338834079428,
-0.00616734988680402));
#29189=CARTESIAN_POINT('Ctrl Pts',(-0.224903937950997,-0.00100476933014151,
-0.00458381173225385));
#29190=CARTESIAN_POINT('Ctrl Pts',(-0.228004563842973,-0.000997949740617374,
-0.00458943898701532));
#29191=CARTESIAN_POINT('Ctrl Pts',(-0.231105189790958,-0.000991151361328939,
-0.00459505880592969));
#29192=CARTESIAN_POINT('Ctrl Pts',(-0.234205815794275,-0.000984373265027772,
-0.00460066961067425));
#29193=CARTESIAN_POINT('Ctrl Pts',(-0.224903434943426,-0.00130314167877163,
-0.00330350941820122));
#29194=CARTESIAN_POINT('Ctrl Pts',(-0.228004062879574,-0.00128286930948369,
-0.00330122419140405));
#29195=CARTESIAN_POINT('Ctrl Pts',(-0.231104690943801,-0.00126261869681616,
-0.0032989320974583));
#29196=CARTESIAN_POINT('Ctrl Pts',(-0.234205319131308,-0.00124238896138437,
-0.00329663139924215));
#29197=CARTESIAN_POINT('Ctrl Pts',(-0.224903041260456,-0.00140805611840559,
-0.00232453718253355));
#29198=CARTESIAN_POINT('Ctrl Pts',(-0.228003673257076,-0.0013756315595115,
-0.00231672000225054));
#29199=CARTESIAN_POINT('Ctrl Pts',(-0.231104305522642,-0.00134323774830377,
-0.00230888218475535));
#29200=CARTESIAN_POINT('Ctrl Pts',(-0.234204938019884,-0.00131087220379368,
-0.00230102069899992));
#29201=CARTESIAN_POINT('Ctrl Pts',(-0.224902686634356,-0.00144960594189391,
-0.00134999602285112));
#29202=CARTESIAN_POINT('Ctrl Pts',(-0.228003316903184,-0.00140612182039602,
-0.00134119316178982));
#29203=CARTESIAN_POINT('Ctrl Pts',(-0.23110394734855,-0.00136264456921374,
-0.00133240814074275));
#29204=CARTESIAN_POINT('Ctrl Pts',(-0.234204577993143,-0.00131917594314456,
-0.00132364092587474));
#29205=CARTESIAN_POINT('Ctrl Pts',(-0.22490247733939,-0.0014891827680679,
-8.48946648711828E-5));
#29206=CARTESIAN_POINT('Ctrl Pts',(-0.228003104745152,-0.00143870380997731,
-8.36968663193096E-5));
#29207=CARTESIAN_POINT('Ctrl Pts',(-0.231103732057244,-0.00138822193789455,
-8.25021078797203E-5));
#29208=CARTESIAN_POINT('Ctrl Pts',(-0.23420435926242,-0.00133773601187166,
-8.1311084157012E-5));
#29209=CARTESIAN_POINT('Ctrl Pts',(-0.22490260183294,-0.0014577307002292,
0.00116946334942344));
#29210=CARTESIAN_POINT('Ctrl Pts',(-0.228003232282475,-0.00141157334093523,
0.00115947282708936));
#29211=CARTESIAN_POINT('Ctrl Pts',(-0.231103862912961,-0.00136541961535455,
0.00114950766822477));
#29212=CARTESIAN_POINT('Ctrl Pts',(-0.234204493755065,-0.001319272064998,
0.00113956823678177));
#29213=CARTESIAN_POINT('Ctrl Pts',(-0.224903104718753,-0.00140104996632292,
0.00247428939345485));
#29214=CARTESIAN_POINT('Ctrl Pts',(-0.228003735975788,-0.00137069112187628,
0.00246735401736931));
#29215=CARTESIAN_POINT('Ctrl Pts',(-0.231104367476161,-0.0013403616690761,
0.00246039968961847));
#29216=CARTESIAN_POINT('Ctrl Pts',(-0.234204999187845,-0.00131005933689176,
0.00245342357850486));
#29217=CARTESIAN_POINT('Ctrl Pts',(-0.224903620487317,-0.00123313642614889,
0.00377581720335721));
#29218=CARTESIAN_POINT('Ctrl Pts',(-0.228004247058324,-0.00121832689931329,
0.00377611259775251));
#29219=CARTESIAN_POINT('Ctrl Pts',(-0.231104873711069,-0.00120353701330459,
0.00377640441621043));
#29220=CARTESIAN_POINT('Ctrl Pts',(-0.234205500449294,-0.00118876627184354,
0.00377669124621538));
#29221=CARTESIAN_POINT('Ctrl Pts',(-0.224904244452509,-0.000745411287960432,
0.00535508951527424));
#29222=CARTESIAN_POINT('Ctrl Pts',(-0.228004869369835,-0.000745883603517816,
0.00536654310520161));
#29223=CARTESIAN_POINT('Ctrl Pts',(-0.231105494301186,-0.000746375225293753,
0.00537799072107391));
#29224=CARTESIAN_POINT('Ctrl Pts',(-0.234206119249757,-0.000746885383007411,
0.00538943105918803));
#29225=CARTESIAN_POINT('Ctrl Pts',(-0.224904927022406,0.000243903830950042,
0.00708094602779947));
#29226=CARTESIAN_POINT('Ctrl Pts',(-0.22800555124417,0.000231747907332828,
0.00710847531073915));
#29227=CARTESIAN_POINT('Ctrl Pts',(-0.231106175424446,0.00021957829815924,
0.00713600296412369));
#29228=CARTESIAN_POINT('Ctrl Pts',(-0.234206799572117,0.000207395346249357,
0.0071635283576419));
#29229=CARTESIAN_POINT('Ctrl Pts',(-0.224905705882564,0.00204129536417242,
0.00904270545084878));
#29230=CARTESIAN_POINT('Ctrl Pts',(-0.228006331417495,0.00202251745037019,
0.00909153197079319));
#29231=CARTESIAN_POINT('Ctrl Pts',(-0.231106956906316,0.00200373108991613,
0.00914035807264341));
#29232=CARTESIAN_POINT('Ctrl Pts',(-0.234207582354303,0.00198493654309014,
0.00918918354252649));
#29233=CARTESIAN_POINT('Ctrl Pts',(-0.224906344934492,0.00503279669879239,
0.0106558220281949));
#29234=CARTESIAN_POINT('Ctrl Pts',(-0.228006973230644,0.00502108315461209,
0.0107253467403358));
#29235=CARTESIAN_POINT('Ctrl Pts',(-0.231107601524016,0.00500936667421796,
0.0107948715627757));
#29236=CARTESIAN_POINT('Ctrl Pts',(-0.234208229814862,0.00499764738343722,
0.0108643965065502));
#29237=CARTESIAN_POINT('Ctrl Pts',(-0.22490642148267,0.00911553811978304,
0.0108495997280891));
#29238=CARTESIAN_POINT('Ctrl Pts',(-0.22800705020616,0.00912342211753167,
0.0109217712057851));
#29239=CARTESIAN_POINT('Ctrl Pts',(-0.231107678935135,0.0091313080421625,
0.0109939426427322));
#29240=CARTESIAN_POINT('Ctrl Pts',(-0.234208307668951,0.00913919580236395,
0.0110661140483708));
#29241=CARTESIAN_POINT('Ctrl Pts',(-0.224905896781363,0.0122479140000228,
0.00952499840433065));
#29242=CARTESIAN_POINT('Ctrl Pts',(-0.228006522998932,0.0122659797356893,
0.00957977773742142));
#29243=CARTESIAN_POINT('Ctrl Pts',(-0.231107149178945,0.012284052220171,
0.00963455709198015));
#29244=CARTESIAN_POINT('Ctrl Pts',(-0.234207775325653,0.0123021312474762,
0.00968933635838273));
#29245=CARTESIAN_POINT('Ctrl Pts',(-0.224905188406661,0.0142245802852993,
0.00774097735435126));
#29246=CARTESIAN_POINT('Ctrl Pts',(-0.228005812932864,0.014239626038719,
0.0077754139801973));
#29247=CARTESIAN_POINT('Ctrl Pts',(-0.231106437412959,0.0142546840218181,
0.00780984919513146));
#29248=CARTESIAN_POINT('Ctrl Pts',(-0.234207061854539,0.014269753892948,
0.00784428248742507));
#29249=CARTESIAN_POINT('Ctrl Pts',(-0.224904545213284,0.0153743354777482,
0.00611286639462737));
#29250=CARTESIAN_POINT('Ctrl Pts',(-0.228005169501712,0.0153806533667306,
0.00613103086359291));
#29251=CARTESIAN_POINT('Ctrl Pts',(-0.231105793769188,0.0153869873403304,
0.0061491924949429));
#29252=CARTESIAN_POINT('Ctrl Pts',(-0.234206418024041,0.0153933369583363,
0.00616735039916125));
#29253=CARTESIAN_POINT('Ctrl Pts',(-0.224903937959543,0.0160047733300576,
0.00458381273421664));
#29254=CARTESIAN_POINT('Ctrl Pts',(-0.228004563851456,0.015997954017428,
0.00458944005855562));
#29255=CARTESIAN_POINT('Ctrl Pts',(-0.231105189799372,0.0159911559151915,
0.00459505994710943));
#29256=CARTESIAN_POINT('Ctrl Pts',(-0.234205815802617,0.0159843780961064,
0.00460067082154373));
#29257=CARTESIAN_POINT('Ctrl Pts',(-0.224903434945887,0.0163031426775171,
0.00330350985910996));
#29258=CARTESIAN_POINT('Ctrl Pts',(-0.228004062882068,0.0162828703806443,
0.0033012246620879));
#29259=CARTESIAN_POINT('Ctrl Pts',(-0.231104690946332,0.0162626198410551,
0.00329893259759974));
#29260=CARTESIAN_POINT('Ctrl Pts',(-0.23420531913388,0.0162423901793082,
0.00329663192843727));
#29261=CARTESIAN_POINT('Ctrl Pts',(-0.224903172488496,0.0163730847941923,
0.00265086132944247));
#29262=CARTESIAN_POINT('Ctrl Pts',(-0.22800380313163,0.0163447109764496,
0.00264488813827189));
#29263=CARTESIAN_POINT('Ctrl Pts',(-0.231104433996755,0.0163163649094739,
0.00263889889986091));
#29264=CARTESIAN_POINT('Ctrl Pts',(-0.234205065057425,0.0162880446461359,
0.00263289101445681));
#29265=CARTESIAN_POINT('Ctrl Pts',(-0.224903047769934,0.0163974953490442,
0.00232527569536224));
#29266=CARTESIAN_POINT('Ctrl Pts',(-0.228003678801843,0.0163652528946496,
0.00231821622721085));
#29267=CARTESIAN_POINT('Ctrl Pts',(-0.23110431006382,0.0163330357098684,
0.00231114482972889));
#29268=CARTESIAN_POINT('Ctrl Pts',(-0.234204941533998,0.0163008422866106,
0.00230405918705812));
#29269=CARTESIAN_POINT('',(-0.228104649974285,0.0163642118483275,0.00231798200374012));
#29270=CARTESIAN_POINT('',(-0.225870784240265,0.0163857105469993,0.002322957879709));
#29271=CARTESIAN_POINT('Ctrl Pts',(-0.228104649974285,0.0163642118483275,
0.00231798200374011));
#29272=CARTESIAN_POINT('Ctrl Pts',(-0.227360035832473,0.0163719507139063,
0.00231967936742506));
#29273=CARTESIAN_POINT('Ctrl Pts',(-0.226615421703495,0.0163796910068899,
0.00232137599715635));
#29274=CARTESIAN_POINT('Ctrl Pts',(-0.225870807587654,0.0163874327481649,
0.00232307192500813));
#29275=CARTESIAN_POINT('',(-0.230598290824789,0.00749145062540444,0.0108193267850442));
#29276=CARTESIAN_POINT('Ctrl Pts',(-0.230598338270789,0.00749148676553765,
0.0108179004527726));
#29277=CARTESIAN_POINT('Ctrl Pts',(-0.231075709301529,0.0080180520759082,
0.0108293962485369));
#29278=CARTESIAN_POINT('Ctrl Pts',(-0.231557645328989,0.00854079758906138,
0.0107959726164992));
#29279=CARTESIAN_POINT('Ctrl Pts',(-0.232015464789001,0.00907681658494018,
0.010708872070951));
#29280=CARTESIAN_POINT('Ctrl Pts',(-0.232075029452916,0.00914655541024208,
0.0106975398424733));
#29281=CARTESIAN_POINT('Ctrl Pts',(-0.232134185876658,0.00921651233077271,
0.0106852715763912));
#29282=CARTESIAN_POINT('Ctrl Pts',(-0.232192870888001,0.00928671955653243,
0.0106720330949619));
#29283=CARTESIAN_POINT('Ctrl Pts',(-0.232447746520514,0.00959163746764531,
0.0106145368748788));
#29284=CARTESIAN_POINT('Ctrl Pts',(-0.232693736801378,0.00990130138696256,
0.0105389619391001));
#29285=CARTESIAN_POINT('Ctrl Pts',(-0.232918888539751,0.0102190020370645,
0.0104406042903564));
#29286=CARTESIAN_POINT('Ctrl Pts',(-0.233144040278124,0.0105367026871664,
0.0103422466416127));
#29287=CARTESIAN_POINT('Ctrl Pts',(-0.233348352430801,0.0108624519973364,
0.0102211499069169));
#29288=CARTESIAN_POINT('Ctrl Pts',(-0.233508739760675,0.0111978248649097,
0.0100695900518698));
#29289=CARTESIAN_POINT('Ctrl Pts',(-0.23366912709055,0.011533197732483,
0.00991803019682276));
#29290=CARTESIAN_POINT('Ctrl Pts',(-0.233785605808925,0.0118778624208235,
0.00973525367538941));
#29291=CARTESIAN_POINT('Ctrl Pts',(-0.233833346895058,0.0122149827284696,
0.00952313657254382));
#29292=CARTESIAN_POINT('Ctrl Pts',(-0.233858854995816,0.0123951063802632,
0.00940980223371623));
#29293=CARTESIAN_POINT('Ctrl Pts',(-0.233864744317832,0.0125731343241547,
0.00928811633672739));
#29294=CARTESIAN_POINT('Ctrl Pts',(-0.233851336158348,0.0127452593029888,
0.00916045586438089));
#29295=CARTESIAN_POINT('Ctrl Pts',(-0.233839649540966,0.01289528427637,
0.00904918637232152));
#29296=CARTESIAN_POINT('Ctrl Pts',(-0.233813302729673,0.0130408301132514,
0.00893339848908481));
#29297=CARTESIAN_POINT('Ctrl Pts',(-0.233772508743751,0.0131799182240714,
0.00881533220150123));
#29298=CARTESIAN_POINT('Ctrl Pts',(-0.233684911456983,0.0134785833545798,
0.00856180741795297));
#29299=CARTESIAN_POINT('Ctrl Pts',(-0.233530684540018,0.0137474510773739,
0.00829768449632733));
#29300=CARTESIAN_POINT('Ctrl Pts',(-0.233333723716297,0.0139829954115555,
0.00803862781489455));
#29301=CARTESIAN_POINT('Ctrl Pts',(-0.233268591230206,0.0140608869829865,
0.00795296100369058));
#29302=CARTESIAN_POINT('Ctrl Pts',(-0.233198784817145,0.0141351725004418,
0.00786786509877418));
#29303=CARTESIAN_POINT('Ctrl Pts',(-0.233125029661844,0.0142061824254741,
0.00778346848116448));
#29304=CARTESIAN_POINT('Ctrl Pts',(-0.232975749017138,0.014349906716285,
0.00761264948639352));
#29305=CARTESIAN_POINT('Ctrl Pts',(-0.232810292019128,0.0144802373306716,
0.00744474134059401));
#29306=CARTESIAN_POINT('Ctrl Pts',(-0.232634671293171,0.0145996931398721,
0.00728027181219894));
#29307=CARTESIAN_POINT('Ctrl Pts',(-0.232372281556117,0.0147781685344756,
0.00703454274990358));
#29308=CARTESIAN_POINT('Ctrl Pts',(-0.232087200057163,0.0149326947045112,
0.00679688383923861));
#29309=CARTESIAN_POINT('Ctrl Pts',(-0.231801872342179,0.0150754733334955,
0.00655540940052881));
#29310=CARTESIAN_POINT('Ctrl Pts',(-0.231631035659178,0.0151609603931055,
0.00641082936160338));
#29311=CARTESIAN_POINT('Ctrl Pts',(-0.23146011161664,0.0152420740677067,
0.00626478376969512));
#29312=CARTESIAN_POINT('Ctrl Pts',(-0.231289702355054,0.0153194156731576,
0.00611622994638233));
#29313=CARTESIAN_POINT('Ctrl Pts',(-0.231175497771615,0.0153712483361878,
0.00601667240266783));
#29314=CARTESIAN_POINT('Ctrl Pts',(-0.231061524394753,0.0154213809749297,
0.00591598467855481));
#29315=CARTESIAN_POINT('Ctrl Pts',(-0.230947963472988,0.015469955354092,
0.00581382564276621));
#29316=CARTESIAN_POINT('Ctrl Pts',(-0.230417408077528,0.0156968943269831,
0.00533653973498424));
#29317=CARTESIAN_POINT('Ctrl Pts',(-0.229895853940728,0.0158913130140226,
0.00482791912667798));
#29318=CARTESIAN_POINT('Ctrl Pts',(-0.229425773391357,0.0160470074394846,
0.00426455622278852));
#29319=CARTESIAN_POINT('Ctrl Pts',(-0.229394351628951,0.0160574145776897,
0.00422689915457296));
#29320=CARTESIAN_POINT('Ctrl Pts',(-0.229363159852714,0.0160676398558769,
0.00418899687521678));
#29321=CARTESIAN_POINT('Ctrl Pts',(-0.229332210744518,0.01607767331279,
0.00415084139727865));
#29322=CARTESIAN_POINT('Ctrl Pts',(-0.229110485079378,0.0161495550256201,
0.00387748784308456));
#29323=CARTESIAN_POINT('Ctrl Pts',(-0.228901208712299,0.0162114615840728,
0.00359107867848368));
#29324=CARTESIAN_POINT('Ctrl Pts',(-0.228703844969547,0.0162580746565335,
0.00329766208763771));
#29325=CARTESIAN_POINT('Ctrl Pts',(-0.228681366063252,0.0162633836908746,
0.00326424316297096));
#29326=CARTESIAN_POINT('Ctrl Pts',(-0.228659041690429,0.0162684961078405,
0.00323073414136287));
#29327=CARTESIAN_POINT('Ctrl Pts',(-0.22863687106733,0.0162734193664932,
0.00319714803077916));
#29328=CARTESIAN_POINT('Ctrl Pts',(-0.228447731836008,0.0163154200514998,
0.00291062242838303));
#29329=CARTESIAN_POINT('Ctrl Pts',(-0.228269796174735,0.0163437143844762,
0.00261818156401676));
#29330=CARTESIAN_POINT('Ctrl Pts',(-0.228104649974285,0.0163642118483275,
0.00231798200374011));
#29331=CARTESIAN_POINT('',(-0.227106092853892,-0.00144162713113215,-4.25945305502357E-13));
#29332=CARTESIAN_POINT('Ctrl Pts',(-0.230598290824789,0.00749145062540444,
0.0108193267850442));
#29333=CARTESIAN_POINT('Ctrl Pts',(-0.231137836558405,0.00690031499117376,
0.0108309420867985));
#29334=CARTESIAN_POINT('Ctrl Pts',(-0.231682656491661,0.00631350273122054,
0.0107850743940513));
#29335=CARTESIAN_POINT('Ctrl Pts',(-0.232703657130117,0.00510282767464983,
0.0105570407887783));
#29336=CARTESIAN_POINT('Ctrl Pts',(-0.233184403552031,0.00447117767383195,
0.0103741673526736));
#29337=CARTESIAN_POINT('Ctrl Pts',(-0.233827791930478,0.0031373542154347,
0.0097711747197396));
#29338=CARTESIAN_POINT('Ctrl Pts',(-0.233942287932662,0.0024255222673528,
0.00932750132739732));
#29339=CARTESIAN_POINT('Ctrl Pts',(-0.233597340137198,0.0012312754121852,
0.00831720595736921));
#29340=CARTESIAN_POINT('Ctrl Pts',(-0.233162895208997,0.000765896829771336,
0.00778165408574167));
#29341=CARTESIAN_POINT('Ctrl Pts',(-0.232120497057948,5.30358000006855E-5,
0.00680295301175275));
#29342=CARTESIAN_POINT('Ctrl Pts',(-0.231523946961238,-0.000221033348423707,
0.0063348547730625));
#29343=CARTESIAN_POINT('Ctrl Pts',(-0.2303894174303,-0.000708453126336253,
0.00531619348403926));
#29344=CARTESIAN_POINT('Ctrl Pts',(-0.229838118249783,-0.000912401449299848,
0.00477583518142244));
#29345=CARTESIAN_POINT('Ctrl Pts',(-0.228861523205001,-0.00122893765634945,
0.00357768912857529));
#29346=CARTESIAN_POINT('Ctrl Pts',(-0.228422516777517,-0.00133275751547238,
0.00291658072635947));
#29347=CARTESIAN_POINT('Ctrl Pts',(-0.22766666238982,-0.00140726267608253,
0.00150192904840282));
#29348=CARTESIAN_POINT('Ctrl Pts',(-0.227382852307235,-0.00143731421920346,
0.000752971789795249));
#29349=CARTESIAN_POINT('Ctrl Pts',(-0.227106092853892,-0.00144162713113215,
-4.25945305518629E-13));
#29350=CARTESIAN_POINT('',(-0.230713724481977,0.00748904929732134,-0.0108219320073967));
#29351=CARTESIAN_POINT('Ctrl Pts',(-0.227106121514272,-0.00144104810369251,
-1.02597508904584E-7));
#29352=CARTESIAN_POINT('Ctrl Pts',(-0.227155693329604,-0.00144058004175401,
-0.000133357544037));
#29353=CARTESIAN_POINT('Ctrl Pts',(-0.227205192185135,-0.00143930885807063,
-0.000266817081085626));
#29354=CARTESIAN_POINT('Ctrl Pts',(-0.227255433548676,-0.00143710688843238,
-0.000399941268947333));
#29355=CARTESIAN_POINT('Ctrl Pts',(-0.227349644824292,-0.00143297781322698,
-0.000649572223793228));
#29356=CARTESIAN_POINT('Ctrl Pts',(-0.227446467189041,-0.00142558282116148,
-0.000898063096286006));
#29357=CARTESIAN_POINT('Ctrl Pts',(-0.227551278208355,-0.00141727302005574,
-0.00114210175313649));
#29358=CARTESIAN_POINT('Ctrl Pts',(-0.227580845424984,-0.00141492882293749,
-0.00121094512361562));
#29359=CARTESIAN_POINT('Ctrl Pts',(-0.227611049598159,-0.00141251265768409,
-0.00127939207005976));
#29360=CARTESIAN_POINT('Ctrl Pts',(-0.227641897465485,-0.0014100715425958,
-0.00134749262536686));
#29361=CARTESIAN_POINT('Ctrl Pts',(-0.227778730077697,-0.00139924343085938,
-0.00164956786373419));
#29362=CARTESIAN_POINT('Ctrl Pts',(-0.227928226950739,-0.00138769770517313,
-0.00194470860115159));
#29363=CARTESIAN_POINT('Ctrl Pts',(-0.228090954362009,-0.00136955019749903,
-0.00223115768111268));
#29364=CARTESIAN_POINT('Ctrl Pts',(-0.228107429541393,-0.00136771287063466,
-0.00226015894119409));
#29365=CARTESIAN_POINT('Ctrl Pts',(-0.228124040407681,-0.00136580989150037,
-0.00228907248515574));
#29366=CARTESIAN_POINT('Ctrl Pts',(-0.228140785043584,-0.00136383629327108,
-0.00231789963233035));
#29367=CARTESIAN_POINT('Ctrl Pts',(-0.228326714931641,-0.00134192175897111,
-0.00263799188624149));
#29368=CARTESIAN_POINT('Ctrl Pts',(-0.228529137687204,-0.00131121851168663,
-0.00294734231443703));
#29369=CARTESIAN_POINT('Ctrl Pts',(-0.228745449586204,-0.00126531502200679,
-0.00324782568531596));
#29370=CARTESIAN_POINT('Ctrl Pts',(-0.228757414188977,-0.00126277601688286,
-0.00326444596459402));
#29371=CARTESIAN_POINT('Ctrl Pts',(-0.2287694212518,-0.00126019050384389,
-0.00328103996521208));
#29372=CARTESIAN_POINT('Ctrl Pts',(-0.228781470464013,-0.00125755773271125,
-0.00329760590338844));
#29373=CARTESIAN_POINT('Ctrl Pts',(-0.229006881398939,-0.00120830510175236,
-0.00360751360078454));
#29374=CARTESIAN_POINT('Ctrl Pts',(-0.229247043436343,-0.00114232304878351,
-0.00390750717283466));
#29375=CARTESIAN_POINT('Ctrl Pts',(-0.229499929863164,-0.00106702408187035,
-0.00418927640242565));
#29376=CARTESIAN_POINT('Ctrl Pts',(-0.229522633013788,-0.00106026403622785,
-0.0042145725376951));
#29377=CARTESIAN_POINT('Ctrl Pts',(-0.229545438774004,-0.00105343027253221,
-0.00423972250785708));
#29378=CARTESIAN_POINT('Ctrl Pts',(-0.229568343811177,-0.00104652599570539,
-0.00426473093900274));
#29379=CARTESIAN_POINT('Ctrl Pts',(-0.230082985397726,-0.000891397324517587,
-0.00482663261088408));
#29380=CARTESIAN_POINT('Ctrl Pts',(-0.230647745298193,-0.000704074407847329,
-0.00531755702186263));
#29381=CARTESIAN_POINT('Ctrl Pts',(-0.231224812138477,-0.000484699658335017,
-0.00578481572901948));
#29382=CARTESIAN_POINT('Ctrl Pts',(-0.231363643146476,-0.000431922379381618,
-0.00589722904543737));
#29383=CARTESIAN_POINT('Ctrl Pts',(-0.231503186860206,-0.000377137686368691,
-0.00600819219499035));
#29384=CARTESIAN_POINT('Ctrl Pts',(-0.231642644775951,-0.000320010544310574,
-0.00611831970598614));
#29385=CARTESIAN_POINT('Ctrl Pts',(-0.231805922867053,-0.000253125773693158,
-0.00624725759866292));
#29386=CARTESIAN_POINT('Ctrl Pts',(-0.231969083349277,-0.000183034363518878,
-0.0063750542300276));
#29387=CARTESIAN_POINT('Ctrl Pts',(-0.232130844677489,-0.000109068387591157,
-0.00650260226534622));
#29388=CARTESIAN_POINT('Ctrl Pts',(-0.232430768434771,2.80728788441698E-5,
-0.00673909071663125));
#29389=CARTESIAN_POINT('Ctrl Pts',(-0.232725879386454,0.000178054062844723,
-0.00697503327306245));
#29390=CARTESIAN_POINT('Ctrl Pts',(-0.232995079390541,0.000354507597007201,
-0.00722285002535608));
#29391=CARTESIAN_POINT('Ctrl Pts',(-0.233193492774877,0.000484562360601881,
-0.00740550292198027));
#29392=CARTESIAN_POINT('Ctrl Pts',(-0.23337783274223,0.000629180229882582,
-0.00759438076149401));
#29393=CARTESIAN_POINT('Ctrl Pts',(-0.233537670556691,0.000791923770424381,
-0.00778802745486344));
#29394=CARTESIAN_POINT('Ctrl Pts',(-0.23359469482767,0.00084998469791584,
-0.00785711349407122));
#29395=CARTESIAN_POINT('Ctrl Pts',(-0.233648600459144,0.00091035749609578,
-0.00792679521495199));
#29396=CARTESIAN_POINT('Ctrl Pts',(-0.233698913878109,0.000973215124293755,
-0.00799697080557788));
#29397=CARTESIAN_POINT('Ctrl Pts',(-0.233890254736577,0.00121226134273606,
-0.00826384707894346));
#29398=CARTESIAN_POINT('Ctrl Pts',(-0.234029653034362,0.00148782950287383,
-0.00853756246098401));
#29399=CARTESIAN_POINT('Ctrl Pts',(-0.234097409173442,0.001791730240335,
-0.00879751626456002));
#29400=CARTESIAN_POINT('Ctrl Pts',(-0.234130392260149,0.00193966642014468,
-0.0089240594672824));
#29401=CARTESIAN_POINT('Ctrl Pts',(-0.234146401069839,0.00209427982761353,
-0.00904742046654428));
#29402=CARTESIAN_POINT('Ctrl Pts',(-0.234145973735161,0.00225315437049859,
-0.00916512267717759));
#29403=CARTESIAN_POINT('Ctrl Pts',(-0.234145523209371,0.00242065090741761,
-0.00928921249239144));
#29404=CARTESIAN_POINT('Ctrl Pts',(-0.234126804174283,0.00259287994874721,
-0.00940699897382431));
#29405=CARTESIAN_POINT('Ctrl Pts',(-0.234090447596687,0.00276628068025388,
-0.00951652399136892));
#29406=CARTESIAN_POINT('Ctrl Pts',(-0.234019605920159,0.00310415622694662,
-0.00972993615438505));
#29407=CARTESIAN_POINT('Ctrl Pts',(-0.233881780562192,0.00344657603079677,
-0.00991199840598362));
#29408=CARTESIAN_POINT('Ctrl Pts',(-0.233704476049298,0.00377932616870677,
-0.0100631762672343));
#29409=CARTESIAN_POINT('Ctrl Pts',(-0.233527171536405,0.00411207630661675,
-0.010214354128485));
#29410=CARTESIAN_POINT('Ctrl Pts',(-0.233310373291621,0.0044348431974112,
-0.0103353281859855));
#29411=CARTESIAN_POINT('Ctrl Pts',(-0.233075995771984,0.00475136497202466,
-0.010434359257892));
#29412=CARTESIAN_POINT('Ctrl Pts',(-0.232841618252347,0.00506788674663812,
-0.0105333903297984));
#29413=CARTESIAN_POINT('Ctrl Pts',(-0.232589665495774,0.00537823114335763,
-0.0106102967675239));
#29414=CARTESIAN_POINT('Ctrl Pts',(-0.232329965345587,0.00568405166373154,
-0.0106689815317353));
#29415=CARTESIAN_POINT('Ctrl Pts',(-0.232262092790211,0.00576397776384801,
-0.0106843187770383));
#29416=CARTESIAN_POINT('Ctrl Pts',(-0.232193690473423,0.0058435951715305,
-0.0106984007232942));
#29417=CARTESIAN_POINT('Ctrl Pts',(-0.232124836546004,0.00592295531648019,
-0.0107112767769113));
#29418=CARTESIAN_POINT('Ctrl Pts',(-0.231666783618184,0.00645090118840314,
-0.0107969351304606));
#29419=CARTESIAN_POINT('Ctrl Pts',(-0.231188744745006,0.0069671170222193,
-0.0108308057086929));
#29420=CARTESIAN_POINT('Ctrl Pts',(-0.230713726037419,0.00748903819150086,
-0.0108205087422449));
#29421=CARTESIAN_POINT('',(-0.234023415843097,0.0119530144195835,-0.00968754222491457));
#29422=CARTESIAN_POINT('Ctrl Pts',(-0.234023415843097,0.0119530144195835,
-0.00968754222491458));
#29423=CARTESIAN_POINT('Ctrl Pts',(-0.233998683723066,0.0118727846179345,
-0.00973406438791556));
#29424=CARTESIAN_POINT('Ctrl Pts',(-0.23397056860494,0.0117925041061299,
-0.00977883091294268));
#29425=CARTESIAN_POINT('Ctrl Pts',(-0.233939459378908,0.011712360700619,
-0.00982184594259534));
#29426=CARTESIAN_POINT('Ctrl Pts',(-0.233906531720292,0.0116275326597581,
-0.00986737533668266));
#29427=CARTESIAN_POINT('Ctrl Pts',(-0.233870251248877,0.0115428629938598,
-0.00991093971570111));
#29428=CARTESIAN_POINT('Ctrl Pts',(-0.233831092791455,0.0114585911001557,
-0.0099525457345314));
#29429=CARTESIAN_POINT('Ctrl Pts',(-0.233791934334034,0.0113743192064516,
-0.0099941517533617));
#29430=CARTESIAN_POINT('Ctrl Pts',(-0.233749898049093,0.0112904464442962,
-0.0100337987227811));
#29431=CARTESIAN_POINT('Ctrl Pts',(-0.233705465063116,0.0112072604761169,
-0.0100716075304163));
#29432=CARTESIAN_POINT('Ctrl Pts',(-0.233699173834174,0.0111954822451664,
-0.0100769608475446));
#29433=CARTESIAN_POINT('Ctrl Pts',(-0.233692834401958,0.0111837168196184,
-0.0100822762601016));
#29434=CARTESIAN_POINT('Ctrl Pts',(-0.233686447950412,0.0111719644848117,
-0.0100875538720711));
#29435=CARTESIAN_POINT('Ctrl Pts',(-0.233602623374971,0.0110177106760192,
-0.0101568245115666));
#29436=CARTESIAN_POINT('Ctrl Pts',(-0.233510718268797,0.0108657049951045,
-0.0102195982119736));
#29437=CARTESIAN_POINT('Ctrl Pts',(-0.233412688278746,0.0107154377630033,
-0.0102766354386831));
#29438=CARTESIAN_POINT('Ctrl Pts',(-0.233333564232802,0.0105941508856854,
-0.0103226725355387));
#29439=CARTESIAN_POINT('Ctrl Pts',(-0.233250441725231,0.0104739963145191,
-0.0103649693346423));
#29440=CARTESIAN_POINT('Ctrl Pts',(-0.233164241243107,0.0103547247161384,
-0.0104038910053084));
#29441=CARTESIAN_POINT('Ctrl Pts',(-0.233148078652709,0.010332361291442,
-0.0104111888185583));
#29442=CARTESIAN_POINT('Ctrl Pts',(-0.233131807676021,0.0103100289856585,
-0.0104183679101736));
#29443=CARTESIAN_POINT('Ctrl Pts',(-0.233115434172931,0.0102877262655216,
-0.0104254306152962));
#29444=CARTESIAN_POINT('Ctrl Pts',(-0.233100084013784,0.0102668174653932,
-0.0104320519013487));
#29445=CARTESIAN_POINT('Ctrl Pts',(-0.233084643742608,0.0102459346686751,
-0.0104385708941842));
#29446=CARTESIAN_POINT('Ctrl Pts',(-0.233069118157046,0.0102250766398245,
-0.0104449895109426));
#29447=CARTESIAN_POINT('Ctrl Pts',(-0.233060689266457,0.0102137527485372,
-0.0104484741987291));
#29448=CARTESIAN_POINT('Ctrl Pts',(-0.23305223484736,0.0102024356442983,
-0.0104519294538125));
#29449=CARTESIAN_POINT('Ctrl Pts',(-0.233043755972735,0.0101911255930563,
-0.0104553555826644));
#29450=CARTESIAN_POINT('Ctrl Pts',(-0.232817970043332,0.00988994760137852,
-0.0105465907667275));
#29451=CARTESIAN_POINT('Ctrl Pts',(-0.232574738474408,0.00959387094466128,
-0.0106170019038402));
#29452=CARTESIAN_POINT('Ctrl Pts',(-0.232325841945328,0.00930178982792201,
-0.0106719485881545));
#29453=CARTESIAN_POINT('Ctrl Pts',(-0.232311113206488,0.00928450559135841,
-0.010675200121498));
#29454=CARTESIAN_POINT('Ctrl Pts',(-0.232296365216068,0.00926723529665681,
-0.0106783970891451));
#29455=CARTESIAN_POINT('Ctrl Pts',(-0.232281599593838,0.00924997750557925,
-0.0106815404822746));
#29456=CARTESIAN_POINT('Ctrl Pts',(-0.232165449998461,0.00911422396810377,
-0.0107062670961898));
#29457=CARTESIAN_POINT('Ctrl Pts',(-0.232048211199567,0.00897924268871302,
-0.0107276812960103));
#29458=CARTESIAN_POINT('Ctrl Pts',(-0.231930153270517,0.00884477586957425,
-0.0107458524092826));
#29459=CARTESIAN_POINT('Ctrl Pts',(-0.231530959771025,0.008390098402932,
-0.0108072950447345));
#29460=CARTESIAN_POINT('Ctrl Pts',(-0.231122467023115,0.00794125511677842,
-0.010831736494172));
#29461=CARTESIAN_POINT('Ctrl Pts',(-0.230713724481977,0.00748904929732134,
-0.0108219320073967));
#29462=CARTESIAN_POINT('',(-0.231901468479132,0.0119424667401788,-0.00964990277379924));
#29463=CARTESIAN_POINT('Ctrl Pts',(-0.234023433762422,0.0119524819221575,
-0.00968663343302877));
#29464=CARTESIAN_POINT('Ctrl Pts',(-0.233316123319583,0.0119489346689107,
-0.00967403592336861));
#29465=CARTESIAN_POINT('Ctrl Pts',(-0.232608812875373,0.0119453877511959,
-0.00966143839039684));
#29466=CARTESIAN_POINT('Ctrl Pts',(-0.231901502429748,0.0119418411715371,
-0.00964884083595424));
#29467=CARTESIAN_POINT('',(-0.229385993393222,0.00897975235454292,-0.0106669748894047));
#29468=CARTESIAN_POINT('Ctrl Pts',(-0.229385993393222,0.00897975235454292,
-0.0106669748894047));
#29469=CARTESIAN_POINT('Ctrl Pts',(-0.229637801997236,0.00925253156900348,
-0.0106263784371995));
#29470=CARTESIAN_POINT('Ctrl Pts',(-0.230143566989202,0.00979324393307198,
-0.0105200797848502));
#29471=CARTESIAN_POINT('Ctrl Pts',(-0.230877045355225,0.0106009051517507,
-0.0102792296753082));
#29472=CARTESIAN_POINT('Ctrl Pts',(-0.231476239279836,0.0113059241165943,
-0.00998938196234091));
#29473=CARTESIAN_POINT('Ctrl Pts',(-0.231800050197011,0.0117639008386206,
-0.00975185034792822));
#29474=CARTESIAN_POINT('Ctrl Pts',(-0.231901468479132,0.0119424667401788,
-0.00964990277379923));
#29475=CARTESIAN_POINT('',(-0.227310930575325,0.0119192283365604,-0.00956777733553798));
#29476=CARTESIAN_POINT('Ctrl Pts',(-0.229385995664121,0.00897975213139759,
-0.0106669749755967));
#29477=CARTESIAN_POINT('Ctrl Pts',(-0.229355006960483,0.0090179060614615,
-0.0106598121462576));
#29478=CARTESIAN_POINT('Ctrl Pts',(-0.2293240394562,0.00905602083052721,
-0.0106524155099456));
#29479=CARTESIAN_POINT('Ctrl Pts',(-0.229293106141903,0.0090941017672963,
-0.0106447797757962));
#29480=CARTESIAN_POINT('Ctrl Pts',(-0.229177106213288,0.00923690528018039,
-0.010616145772736));
#29481=CARTESIAN_POINT('Ctrl Pts',(-0.229061589290613,0.00937923436170777,
-0.0105841480216996));
#29482=CARTESIAN_POINT('Ctrl Pts',(-0.228947224677079,0.00952135862731606,
-0.0105485174003977));
#29483=CARTESIAN_POINT('Ctrl Pts',(-0.228861451216929,0.00962795182652228,
-0.0105217944344212));
#29484=CARTESIAN_POINT('Ctrl Pts',(-0.228776325494406,0.00973442928749065,
-0.0104930283924105));
#29485=CARTESIAN_POINT('Ctrl Pts',(-0.22869211714611,0.00984090006277285,
-0.0104621132231097));
#29486=CARTESIAN_POINT('Ctrl Pts',(-0.228679702108351,0.00985659730327293,
-0.0104575553259184));
#29487=CARTESIAN_POINT('Ctrl Pts',(-0.228667307031986,0.00987229430785859,
-0.0104529506167934));
#29488=CARTESIAN_POINT('Ctrl Pts',(-0.228654932681678,0.00988799157762058,
-0.0104482989585942));
#29489=CARTESIAN_POINT('Ctrl Pts',(-0.228635832391485,0.00991222092301825,
-0.0104411189435412));
#29490=CARTESIAN_POINT('Ctrl Pts',(-0.228616781482349,0.00993645090019369,
-0.010433827071427));
#29491=CARTESIAN_POINT('Ctrl Pts',(-0.228597784506831,0.00996068343972998,
-0.0104264214928838));
#29492=CARTESIAN_POINT('Ctrl Pts',(-0.228378653761545,0.0102402065903429,
-0.010340997897746));
#29493=CARTESIAN_POINT('Ctrl Pts',(-0.228166673055731,0.0105201209803018,
-0.0102404785070309));
#29494=CARTESIAN_POINT('Ctrl Pts',(-0.227968690415889,0.0108036788995433,
-0.0101224755697179));
#29495=CARTESIAN_POINT('Ctrl Pts',(-0.22796299351652,0.0108118382054919,
-0.0101190800656497));
#29496=CARTESIAN_POINT('Ctrl Pts',(-0.227957308339109,0.0108200003027273,
-0.0101156700705878));
#29497=CARTESIAN_POINT('Ctrl Pts',(-0.227951635015369,0.0108281652984639,
-0.0101122454794729));
#29498=CARTESIAN_POINT('Ctrl Pts',(-0.227850485459292,0.0109737388161945,
-0.0100511885247029));
#29499=CARTESIAN_POINT('Ctrl Pts',(-0.227753100523097,0.011120233530301,
-0.0099854970956529));
#29500=CARTESIAN_POINT('Ctrl Pts',(-0.227661892781027,0.011267846672996,
-0.00991438783483416));
#29501=CARTESIAN_POINT('Ctrl Pts',(-0.227565569336343,0.0114237392108692,
-0.00983929016444434));
#29502=CARTESIAN_POINT('Ctrl Pts',(-0.227476121499233,0.0115808747436384,
-0.00975815798534802));
#29503=CARTESIAN_POINT('Ctrl Pts',(-0.227396458999089,0.0117396983195354,
-0.00967000980079083));
#29504=CARTESIAN_POINT('Ctrl Pts',(-0.227386884764274,0.0117587865254929,
-0.00965941571428886));
#29505=CARTESIAN_POINT('Ctrl Pts',(-0.227377452040833,0.0117778998428984,
-0.00964872059403839));
#29506=CARTESIAN_POINT('Ctrl Pts',(-0.227368166621285,0.0117970380862449,
-0.00963792287468519));
#29507=CARTESIAN_POINT('Ctrl Pts',(-0.227348451517957,0.0118376730239714,
-0.00961499680746148));
#29508=CARTESIAN_POINT('Ctrl Pts',(-0.227329400560137,0.0118784203858247,
-0.00959160817866039));
#29509=CARTESIAN_POINT('Ctrl Pts',(-0.227310930575325,0.0119192283365604,
-0.00956777733553797));
#29510=CARTESIAN_POINT('',(-0.225106030640403,0.0119077779586431,-0.00952780946947742));
#29511=CARTESIAN_POINT('Ctrl Pts',(-0.227310944993972,0.0119188280769467,
-0.00956708041891526));
#29512=CARTESIAN_POINT('Ctrl Pts',(-0.226575973544427,0.0119151443323247,
-0.00955399012063065));
#29513=CARTESIAN_POINT('Ctrl Pts',(-0.225841002093253,0.0119114609586129,
-0.00954089980346294));
#29514=CARTESIAN_POINT('Ctrl Pts',(-0.225106030640403,0.0119077779586431,
-0.00952780946947742));
#29515=CARTESIAN_POINT('',(-0.22509230219787,0.00750490891545138,-0.0106935438270112));
#29516=CARTESIAN_POINT('Ctrl Pts',(-0.225106030640403,0.0119077779586431,
-0.00952780946947742));
#29517=CARTESIAN_POINT('Ctrl Pts',(-0.225003294965764,0.0112735761688805,
-0.00988629126619056));
#29518=CARTESIAN_POINT('Ctrl Pts',(-0.224964958507158,0.0105924278097438,
-0.0101704206208673));
#29519=CARTESIAN_POINT('Ctrl Pts',(-0.224967573052356,0.0098852358922856,
-0.0103667934727557));
#29520=CARTESIAN_POINT('Ctrl Pts',(-0.224967640189741,0.00986707632239798,
-0.0103718360169928));
#29521=CARTESIAN_POINT('Ctrl Pts',(-0.224967734329484,0.00984889964653936,
-0.0103768207544314));
#29522=CARTESIAN_POINT('Ctrl Pts',(-0.224967855074635,0.00983070628477451,
-0.010381747639153));
#29523=CARTESIAN_POINT('Ctrl Pts',(-0.224972881642603,0.00907332457073518,
-0.0105868517009247));
#29524=CARTESIAN_POINT('Ctrl Pts',(-0.225024020919892,0.00828816777677607,
-0.0106912747006324));
#29525=CARTESIAN_POINT('Ctrl Pts',(-0.22509230219787,0.00750490891545138,
-0.0106935438270112));
#29526=CARTESIAN_POINT('',(-0.22512339082026,0.00302752783129386,-0.00949179287466226));
#29527=CARTESIAN_POINT('Ctrl Pts',(-0.225092302193471,0.00750490886465332,
-0.010693543826959));
#29528=CARTESIAN_POINT('Ctrl Pts',(-0.225046870204233,0.00698064601573159,
-0.0106930042825971));
#29529=CARTESIAN_POINT('Ctrl Pts',(-0.225008961521983,0.00645533295426021,
-0.0106467019987212));
#29530=CARTESIAN_POINT('Ctrl Pts',(-0.224987521850832,0.0059382751191565,
-0.0105541685444992));
#29531=CARTESIAN_POINT('Ctrl Pts',(-0.224976996951193,0.00568444744690854,
-0.0105087431593767));
#29532=CARTESIAN_POINT('Ctrl Pts',(-0.224970440928504,0.00543260917693936,
-0.0104521853841945));
#29533=CARTESIAN_POINT('Ctrl Pts',(-0.224968912294139,0.00518375239436985,
-0.010384946549299));
#29534=CARTESIAN_POINT('Ctrl Pts',(-0.224964269823687,0.00442797306195466,
-0.0101807418608635));
#29535=CARTESIAN_POINT('Ctrl Pts',(-0.225005941234088,0.00370066390407666,
-0.00987820272963985));
#29536=CARTESIAN_POINT('Ctrl Pts',(-0.22512331575626,0.00302780787790367,
-0.00949128794938887));
#29537=CARTESIAN_POINT('',(-0.225017273462258,0.00228350670705836,-0.00900753387751742));
#29538=CARTESIAN_POINT('Ctrl Pts',(-0.225016552084744,0.00228362488138197,
-0.00900760247763402));
#29539=CARTESIAN_POINT('Ctrl Pts',(-0.22504874328166,0.00240252866617142,
-0.00909390486499722));
#29540=CARTESIAN_POINT('Ctrl Pts',(-0.225073793197746,0.00252475423756348,
-0.00917795515386039));
#29541=CARTESIAN_POINT('Ctrl Pts',(-0.225101157805034,0.00271695196711039,
-0.00930284738549845));
#29542=CARTESIAN_POINT('Ctrl Pts',(-0.225108617894573,0.00278472801619829,
-0.00934556621454342));
#29543=CARTESIAN_POINT('Ctrl Pts',(-0.225118522059823,0.00291094688437005,
-0.00942268118093157));
#29544=CARTESIAN_POINT('Ctrl Pts',(-0.225121568541063,0.00296915254795865,
-0.00945731247850366));
#29545=CARTESIAN_POINT('Ctrl Pts',(-0.22512312969261,0.00302779944139895,
-0.00949127923732032));
#29546=CARTESIAN_POINT('',(-0.225277037624834,0.00232818316358624,-0.00904462761620701));
#29547=CARTESIAN_POINT('Ctrl Pts',(-0.225276566204441,0.00232796030677252,
-0.00904445642067167));
#29548=CARTESIAN_POINT('Ctrl Pts',(-0.22523775196089,0.00230950230683335,
-0.00903055888584819));
#29549=CARTESIAN_POINT('Ctrl Pts',(-0.225195493315447,0.00229628530974549,
-0.00902022639715284));
#29550=CARTESIAN_POINT('Ctrl Pts',(-0.225107254455047,0.00228121212563282,
-0.00900764771093501));
#29551=CARTESIAN_POINT('Ctrl Pts',(-0.225061856391577,0.00227945979119184,
-0.00900548999868191));
#29552=CARTESIAN_POINT('Ctrl Pts',(-0.225016908981005,0.00228354087081739,
-0.00900754894665053));
#29553=CARTESIAN_POINT('',(-0.225398032236364,0.00187965741570819,-0.00870574455337625));
#29554=CARTESIAN_POINT('Ctrl Pts',(-0.225398012644317,0.00187968458752203,
-0.00870571095552509));
#29555=CARTESIAN_POINT('Ctrl Pts',(-0.225377108190577,0.00195288094167168,
-0.00876479409570467));
#29556=CARTESIAN_POINT('Ctrl Pts',(-0.225356430217593,0.00202706411817278,
-0.00882273457646027));
#29557=CARTESIAN_POINT('Ctrl Pts',(-0.225315794003022,0.00217643669042039,
-0.00893557398364217));
#29558=CARTESIAN_POINT('Ctrl Pts',(-0.225295825541299,0.00225161976744987,
-0.00899051371721635));
#29559=CARTESIAN_POINT('Ctrl Pts',(-0.225276087777197,0.0023277455613394,
-0.00904429419962185));
#29560=CARTESIAN_POINT('',(-0.226396396172104,0.00188100664625559,-0.00872574966728709));
#29561=CARTESIAN_POINT('Ctrl Pts',(-0.225398022753316,0.00187968462648945,
-0.00870571117852498));
#29562=CARTESIAN_POINT('Ctrl Pts',(-0.225564669450736,0.00187995036891675,
-0.00870908127754952));
#29563=CARTESIAN_POINT('Ctrl Pts',(-0.225731316227715,0.00188021543557644,
-0.00871245219588737));
#29564=CARTESIAN_POINT('Ctrl Pts',(-0.226064095893355,0.00188074340384874,
-0.00871918526255622));
#29565=CARTESIAN_POINT('Ctrl Pts',(-0.226230228908158,0.00188100630981627,
-0.00872254740843019));
#29566=CARTESIAN_POINT('Ctrl Pts',(-0.226396361723287,0.00188126854571656,
-0.00872591035494955));
#29567=CARTESIAN_POINT('',(-0.226275854855421,0.00233713586297991,-0.0090706994431196));
#29568=CARTESIAN_POINT('Ctrl Pts',(-0.226275826299596,0.00233714530094412,
-0.00907068034054895));
#29569=CARTESIAN_POINT('Ctrl Pts',(-0.226295295393397,0.00225911649706514,
-0.00901557814944029));
#29570=CARTESIAN_POINT('Ctrl Pts',(-0.22631507768356,0.00218209886260719,
-0.00895927286362518));
#29571=CARTESIAN_POINT('Ctrl Pts',(-0.226355247076649,0.0020301452459405,
-0.00884433828949768));
#29572=CARTESIAN_POINT('Ctrl Pts',(-0.226375636754673,0.00195519562172708,
-0.00878570253700721));
#29573=CARTESIAN_POINT('Ctrl Pts',(-0.226396330981692,0.00188126708771283,
-0.00872590858518578));
#29574=CARTESIAN_POINT('',(-0.227050813062771,0.00230629182834679,-0.00906389588700253));
#29575=CARTESIAN_POINT('Ctrl Pts',(-0.227050802694897,0.00230590961093097,
-0.00906362093448274));
#29576=CARTESIAN_POINT('Ctrl Pts',(-0.226921324130421,0.00229945469111778,
-0.0090564308441887));
#29577=CARTESIAN_POINT('Ctrl Pts',(-0.226791421429502,0.00229884660704338,
-0.00905343747495934));
#29578=CARTESIAN_POINT('Ctrl Pts',(-0.226532505026649,0.00230931135191709,
-0.0090558621977966));
#29579=CARTESIAN_POINT('Ctrl Pts',(-0.226403693609709,0.00232032762959314,
-0.00906124325580749));
#29580=CARTESIAN_POINT('Ctrl Pts',(-0.226275841324095,0.00233714970144879,
-0.00907068376606783));
#29581=CARTESIAN_POINT('',(-0.229392048724075,0.00598507781155818,-0.0106610739775155));
#29582=CARTESIAN_POINT('Ctrl Pts',(-0.229392039407141,0.00598506674127622,
-0.0106610718294251));
#29583=CARTESIAN_POINT('Ctrl Pts',(-0.229376263879727,0.00596635918551221,
-0.0106574720776792));
#29584=CARTESIAN_POINT('Ctrl Pts',(-0.229360518248087,0.00594764474891851,
-0.0106538089624593));
#29585=CARTESIAN_POINT('Ctrl Pts',(-0.229344803135537,0.00592892334569771,
-0.0106500820381302));
#29586=CARTESIAN_POINT('Ctrl Pts',(-0.228860120685564,0.00535152146254403,
-0.0105351369616001));
#29587=CARTESIAN_POINT('Ctrl Pts',(-0.22840446889792,0.00476672800595227,
-0.0103604760517174));
#29588=CARTESIAN_POINT('Ctrl Pts',(-0.227996133929565,0.00417509627566239,
-0.0101124588811835));
#29589=CARTESIAN_POINT('Ctrl Pts',(-0.227785346616275,0.00386968901801932,
-0.00998442950070386));
#29590=CARTESIAN_POINT('Ctrl Pts',(-0.227587167224861,0.00356238788559785,
-0.00983691076309596));
#29591=CARTESIAN_POINT('Ctrl Pts',(-0.227429976757087,0.00324829610005773,
-0.0096628079242218));
#29592=CARTESIAN_POINT('Ctrl Pts',(-0.227272786289312,0.0029342043145176,
-0.00948870508534763));
#29593=CARTESIAN_POINT('Ctrl Pts',(-0.227156605059703,0.00261384836770206,
-0.00928704688478299));
#29594=CARTESIAN_POINT('Ctrl Pts',(-0.227050813062771,0.00230629182834679,
-0.00906389588700253));
#29595=CARTESIAN_POINT('',(-0.225010431372201,-0.00147369574979845,-8.4492836099348E-8));
#29596=CARTESIAN_POINT('Ctrl Pts',(-0.229392050505309,0.00598507587768533,
-0.0106610736635327));
#29597=CARTESIAN_POINT('Ctrl Pts',(-0.229409546005236,0.00596627858890805,
-0.0106582040682476));
#29598=CARTESIAN_POINT('Ctrl Pts',(-0.229427042810866,0.00594748970466014,
-0.0106552720634706));
#29599=CARTESIAN_POINT('Ctrl Pts',(-0.229444539825254,0.00592870925509559,
-0.0106522774653289));
#29600=CARTESIAN_POINT('Ctrl Pts',(-0.229679303096811,0.00567672570617227,
-0.0106120979443468));
#29601=CARTESIAN_POINT('Ctrl Pts',(-0.229914103960048,0.00542625026694678,
-0.0105606753677848));
#29602=CARTESIAN_POINT('Ctrl Pts',(-0.230146292910576,0.00517731697708083,
-0.0104978578559838));
#29603=CARTESIAN_POINT('Ctrl Pts',(-0.230395787010163,0.00490983057485797,
-0.0104303585261942));
#29604=CARTESIAN_POINT('Ctrl Pts',(-0.230642262773844,0.00464408630644996,
-0.0103498209007954));
#29605=CARTESIAN_POINT('Ctrl Pts',(-0.230880984377476,0.0043769207193843,
-0.0102539772995695));
#29606=CARTESIAN_POINT('Ctrl Pts',(-0.231119705981108,0.00410975513231864,
-0.0101581336983435));
#29607=CARTESIAN_POINT('Ctrl Pts',(-0.231350667696974,0.00384106818221418,
-0.0100472466834519));
#29608=CARTESIAN_POINT('Ctrl Pts',(-0.231558063831141,0.00356208088917226,
-0.00991289510667101));
#29609=CARTESIAN_POINT('Ctrl Pts',(-0.231661761898224,0.00342258724265129,
-0.00984571931828055));
#29610=CARTESIAN_POINT('Ctrl Pts',(-0.231759570505304,0.00328056322625301,
-0.00977258639660185));
#29611=CARTESIAN_POINT('Ctrl Pts',(-0.231847603316042,0.00313610180678418,
-0.00969249586807556));
#29612=CARTESIAN_POINT('Ctrl Pts',(-0.23193563612678,0.00299164038731536,
-0.00961240533954928));
#29613=CARTESIAN_POINT('Ctrl Pts',(-0.232013892448937,0.00284472310488733,
-0.00952539034512403));
#29614=CARTESIAN_POINT('Ctrl Pts',(-0.232068608495672,0.00269412255633174,
-0.00942902364866202));
#29615=CARTESIAN_POINT('Ctrl Pts',(-0.232120424438827,0.00255150425825015,
-0.00933776465675944));
#29616=CARTESIAN_POINT('Ctrl Pts',(-0.232151133097279,0.00240569654018845,
-0.00923795022913459));
#29617=CARTESIAN_POINT('Ctrl Pts',(-0.232149401495556,0.00226371239656172,
-0.00913346945015538));
#29618=CARTESIAN_POINT('Ctrl Pts',(-0.232149304578969,0.00225576563928716,
-0.00912762173104255));
#29619=CARTESIAN_POINT('Ctrl Pts',(-0.232149106041286,0.00224783059372626,
-0.00912175980534219));
#29620=CARTESIAN_POINT('Ctrl Pts',(-0.232148803895588,0.00223990837733705,
-0.00911588451784818));
#29621=CARTESIAN_POINT('Ctrl Pts',(-0.232143103334322,0.0020904404875636,
-0.00900503588908099));
#29622=CARTESIAN_POINT('Ctrl Pts',(-0.232100523054338,0.00194565874238837,
-0.00888922979231711));
#29623=CARTESIAN_POINT('Ctrl Pts',(-0.232032441227186,0.00181413122320368,
-0.00877725833061356));
#29624=CARTESIAN_POINT('Ctrl Pts',(-0.231896277572882,0.00155107618483428,
-0.00855331540720646));
#29625=CARTESIAN_POINT('Ctrl Pts',(-0.231658075269179,0.00133961295871075,
-0.00834641499925663));
#29626=CARTESIAN_POINT('Ctrl Pts',(-0.231405343490951,0.00115220259560978,
-0.00814850811062457));
#29627=CARTESIAN_POINT('Ctrl Pts',(-0.231235832079804,0.0010265033450625,
-0.008015768665657));
#29628=CARTESIAN_POINT('Ctrl Pts',(-0.231059787339919,0.000911927967415083,
-0.0078867987552611));
#29629=CARTESIAN_POINT('Ctrl Pts',(-0.230879468894514,0.000803917031338677,
-0.00775865188729638));
#29630=CARTESIAN_POINT('Ctrl Pts',(-0.230790942894308,0.000750889865271893,
-0.00769573913516824));
#29631=CARTESIAN_POINT('Ctrl Pts',(-0.230701386819548,0.000699459349445356,
-0.00763300839578708));
#29632=CARTESIAN_POINT('Ctrl Pts',(-0.230611068015914,0.000649165936946226,
-0.00757003102247231));
#29633=CARTESIAN_POINT('Ctrl Pts',(-0.230336779008904,0.000496429965935362,
-0.0073787751544178));
#29634=CARTESIAN_POINT('Ctrl Pts',(-0.230055458506837,0.000354017033221105,
-0.00718541546478645));
#29635=CARTESIAN_POINT('Ctrl Pts',(-0.229779396359619,0.000216017613201449,
-0.00698219836546261));
#29636=CARTESIAN_POINT('Ctrl Pts',(-0.229406479577426,2.96019811534319E-5,
-0.00670768384932898));
#29637=CARTESIAN_POINT('Ctrl Pts',(-0.229043158402296,-0.000148388160636376,
-0.00641509596421757));
#29638=CARTESIAN_POINT('Ctrl Pts',(-0.228694312977108,-0.000315100219245054,
-0.0061008569866271));
#29639=CARTESIAN_POINT('Ctrl Pts',(-0.228526673107328,-0.000395214750719274,
-0.0059498474635566));
#29640=CARTESIAN_POINT('Ctrl Pts',(-0.228362376180949,-0.000472687651889521,
-0.00579383237136698));
#29641=CARTESIAN_POINT('Ctrl Pts',(-0.228201963842599,-0.000547120768336193,
-0.0056324340965861));
#29642=CARTESIAN_POINT('Ctrl Pts',(-0.227783575331477,-0.000741257709973661,
-0.00521147405961152));
#29643=CARTESIAN_POINT('Ctrl Pts',(-0.227391619436755,-0.000914758282893851,
-0.00475369881014943));
#29644=CARTESIAN_POINT('Ctrl Pts',(-0.227033139047913,-0.00105503991125543,
-0.00426160731172168));
#29645=CARTESIAN_POINT('Ctrl Pts',(-0.226968167554637,-0.00108046475221651,
-0.00417241995175197));
#29646=CARTESIAN_POINT('Ctrl Pts',(-0.226904295686128,-0.00110479407840349,
-0.00408211404554795));
#29647=CARTESIAN_POINT('Ctrl Pts',(-0.226841565329479,-0.00112789199908747,
-0.00399070722071771));
#29648=CARTESIAN_POINT('Ctrl Pts',(-0.226687811436992,-0.00118450566116707,
-0.00376666648720267));
#29649=CARTESIAN_POINT('Ctrl Pts',(-0.226540910396871,-0.00123373203013407,
-0.00353600918100793));
#29650=CARTESIAN_POINT('Ctrl Pts',(-0.226401689603115,-0.00127337073319176,
-0.00329931260295964));
#29651=CARTESIAN_POINT('Ctrl Pts',(-0.226355810163533,-0.00128643344769723,
-0.00322131055988149));
#29652=CARTESIAN_POINT('Ctrl Pts',(-0.226310764792651,-0.00129845243507264,
-0.00314265391460194));
#29653=CARTESIAN_POINT('Ctrl Pts',(-0.226266583240457,-0.00130952028889418,
-0.00306340421519403));
#29654=CARTESIAN_POINT('Ctrl Pts',(-0.226131996169734,-0.00134323549243618,
-0.00282199158097784));
#29655=CARTESIAN_POINT('Ctrl Pts',(-0.226005438708994,-0.00136810837940549,
-0.00257479103062637));
#29656=CARTESIAN_POINT('Ctrl Pts',(-0.225887620499229,-0.00138725794483737,
-0.00232303363175134));
#29657=CARTESIAN_POINT('Ctrl Pts',(-0.225849397642494,-0.0013934704912468,
-0.00224135791279094));
#29658=CARTESIAN_POINT('Ctrl Pts',(-0.225812094598808,-0.001399086557685,
-0.00215920486363162));
#29659=CARTESIAN_POINT('Ctrl Pts',(-0.225775735920245,-0.0014042208063698,
-0.00207661730214151));
#29660=CARTESIAN_POINT('Ctrl Pts',(-0.225671099200072,-0.00141899667183484,
-0.0018389383791714));
#29661=CARTESIAN_POINT('Ctrl Pts',(-0.22557429520518,-0.00142977098012393,
-0.00159650160034879));
#29662=CARTESIAN_POINT('Ctrl Pts',(-0.225482531299466,-0.00143967792564172,
-0.00135284436013466));
#29663=CARTESIAN_POINT('Ctrl Pts',(-0.225363801815749,-0.00145249610853613,
-0.00103758643699353));
#29664=CARTESIAN_POINT('Ctrl Pts',(-0.225253510359594,-0.00146400674691899,
-0.000720357869132175));
#29665=CARTESIAN_POINT('Ctrl Pts',(-0.225145577164679,-0.00146962404402618,
-0.000401845801342884));
#29666=CARTESIAN_POINT('Ctrl Pts',(-0.225100262802465,-0.00147198239389232,
-0.000268122610615833));
#29667=CARTESIAN_POINT('Ctrl Pts',(-0.225055364062672,-0.00147329937223217,
-0.000134167155556775));
#29668=CARTESIAN_POINT('Ctrl Pts',(-0.22501043137218,-0.00147369574980066,
-8.44936689116393E-8));
#29669=CARTESIAN_POINT('',(-0.229322739274083,0.00603943600898884,0.0106683693245468));
#29670=CARTESIAN_POINT('Ctrl Pts',(-0.225010431372201,-0.00147369574979845,
-8.4492836099348E-8));
#29671=CARTESIAN_POINT('Ctrl Pts',(-0.225177252440418,-0.00146995924473084,
0.000502352857987205));
#29672=CARTESIAN_POINT('Ctrl Pts',(-0.225343589262149,-0.00145323503816418,
0.00100315816743078));
#29673=CARTESIAN_POINT('Ctrl Pts',(-0.225531292866178,-0.00143309616656037,
0.0014982458852503));
#29674=CARTESIAN_POINT('Ctrl Pts',(-0.225602322658008,-0.00142547532270333,
0.00168559432598046));
#29675=CARTESIAN_POINT('Ctrl Pts',(-0.225676411832131,-0.00141733572264945,
0.00187209120885228));
#29676=CARTESIAN_POINT('Ctrl Pts',(-0.225754737956661,-0.00140663385766833,
0.00205601235174846));
#29677=CARTESIAN_POINT('Ctrl Pts',(-0.225814245385663,-0.00139850323108151,
0.00219574445796982));
#29678=CARTESIAN_POINT('Ctrl Pts',(-0.225876191803857,-0.00138888392204247,
0.00233442708897512));
#29679=CARTESIAN_POINT('Ctrl Pts',(-0.225940507472793,-0.00137697898725081,
0.00247173089544256));
#29680=CARTESIAN_POINT('Ctrl Pts',(-0.226030373988067,-0.00136034454929846,
0.00266358172783048));
#29681=CARTESIAN_POINT('Ctrl Pts',(-0.226124866188928,-0.00133925282069762,
0.00285274028170326));
#29682=CARTESIAN_POINT('Ctrl Pts',(-0.226223799860628,-0.00131321549610233,
0.00303878544699706));
#29683=CARTESIAN_POINT('Ctrl Pts',(-0.226296987449779,-0.00129395401533097,
0.00317641500109331));
#29684=CARTESIAN_POINT('Ctrl Pts',(-0.226372601929934,-0.00127197872634538,
0.00331241011184743));
#29685=CARTESIAN_POINT('Ctrl Pts',(-0.226450485602142,-0.00124712787546466,
0.00344657465293664));
#29686=CARTESIAN_POINT('Ctrl Pts',(-0.226553231728801,-0.00121434399920691,
0.0036235679371649));
#29687=CARTESIAN_POINT('Ctrl Pts',(-0.226659927062532,-0.00117656292596665,
0.00379737392109265));
#29688=CARTESIAN_POINT('Ctrl Pts',(-0.226770209885917,-0.00113435563325404,
0.00396775128429173));
#29689=CARTESIAN_POINT('Ctrl Pts',(-0.227084864123454,-0.00101393158987724,
0.00445386469402914));
#29690=CARTESIAN_POINT('Ctrl Pts',(-0.22742875305635,-0.000857717907044796,
0.00491155504123866));
#29691=CARTESIAN_POINT('Ctrl Pts',(-0.227796711941448,-0.000677481753928545,
0.00533797868158574));
#29692=CARTESIAN_POINT('Ctrl Pts',(-0.227882201087694,-0.000635606872041938,
0.00543705114437668));
#29693=CARTESIAN_POINT('Ctrl Pts',(-0.227968989504244,-0.000592426211065234,
0.00553444710419628));
#29694=CARTESIAN_POINT('Ctrl Pts',(-0.22805701242935,-0.000548074565095271,
0.00563015386475785));
#29695=CARTESIAN_POINT('Ctrl Pts',(-0.228523900026839,-0.000312826379389474,
0.00613779774785378));
#29696=CARTESIAN_POINT('Ctrl Pts',(-0.229025501740472,-4.52917149988218E-5,
0.00659807131512971));
#29697=CARTESIAN_POINT('Ctrl Pts',(-0.229547710152002,0.000243359606321602,
0.00701769548210368));
#29698=CARTESIAN_POINT('Ctrl Pts',(-0.229573852617382,0.000257809885190769,
0.0070387024402748));
#29699=CARTESIAN_POINT('Ctrl Pts',(-0.229600046729066,0.000272313997292378,
0.00705960636108304));
#29700=CARTESIAN_POINT('Ctrl Pts',(-0.229626281725718,0.000286875865311344,
0.00708041461571968));
#29701=CARTESIAN_POINT('Ctrl Pts',(-0.22986207511333,0.000417754181617712,
0.00726743384488521));
#29702=CARTESIAN_POINT('Ctrl Pts',(-0.230101171205871,0.00055316050312438,
0.00744682385458936));
#29703=CARTESIAN_POINT('Ctrl Pts',(-0.230335756719716,0.000696783137501262,
0.00762332499975972));
#29704=CARTESIAN_POINT('Ctrl Pts',(-0.23059644283898,0.000856385606470733,
0.00781946412969107));
#29705=CARTESIAN_POINT('Ctrl Pts',(-0.230851556648128,0.00102597288099953,
0.00801218706259676));
#29706=CARTESIAN_POINT('Ctrl Pts',(-0.231094258515009,0.00121676345105936,
0.00820928893198079));
#29707=CARTESIAN_POINT('Ctrl Pts',(-0.23124674716807,0.00133663643522354,
0.00833312728132895));
#29708=CARTESIAN_POINT('Ctrl Pts',(-0.231394333661979,0.00146485790708328,
0.00845863327908963));
#29709=CARTESIAN_POINT('Ctrl Pts',(-0.231520723189712,0.00160723465436361,
0.00858829560130594));
#29710=CARTESIAN_POINT('Ctrl Pts',(-0.231595496002384,0.0016914656032734,
0.00866500461908271));
#29711=CARTESIAN_POINT('Ctrl Pts',(-0.231662849914153,0.00178067265894138,
0.00874314135189989));
#29712=CARTESIAN_POINT('Ctrl Pts',(-0.231719410813792,0.00187621923147606,
0.0088229581342544));
#29713=CARTESIAN_POINT('Ctrl Pts',(-0.231795494102225,0.0020047443695707,
0.00893032423543671));
#29714=CARTESIAN_POINT('Ctrl Pts',(-0.231852053675257,0.00214485369195234,
0.00904062598124823));
#29715=CARTESIAN_POINT('Ctrl Pts',(-0.231875572818194,0.00229222206788661,
0.00914846641581533));
#29716=CARTESIAN_POINT('Ctrl Pts',(-0.23189909196113,0.00243959044382088,
0.00925630685038242));
#29717=CARTESIAN_POINT('Ctrl Pts',(-0.231889572375894,0.00259430357999544,
0.00936159342295822));
#29718=CARTESIAN_POINT('Ctrl Pts',(-0.231854413493221,0.00274641686514429,
0.00945789529503096));
#29719=CARTESIAN_POINT('Ctrl Pts',(-0.231784095727876,0.00305064343544201,
0.00965049903917647));
#29720=CARTESIAN_POINT('Ctrl Pts',(-0.23161119843415,0.00334377625563083,
0.00980825830993441));
#29721=CARTESIAN_POINT('Ctrl Pts',(-0.231414651287714,0.00362600117395275,
0.00994191747689838));
#29722=CARTESIAN_POINT('Ctrl Pts',(-0.231218104141277,0.00390822609227465,
0.0100755766438623));
#29723=CARTESIAN_POINT('Ctrl Pts',(-0.230997905530183,0.00417947979400734,
0.0101852181167744));
#29724=CARTESIAN_POINT('Ctrl Pts',(-0.230768518905705,0.00444690860942094,
0.0102788235291743));
#29725=CARTESIAN_POINT('Ctrl Pts',(-0.230580860432451,0.0046656889472835,
0.0103554010053859));
#29726=CARTESIAN_POINT('Ctrl Pts',(-0.230387055372245,0.0048819763870309,
0.0104210919474471));
#29727=CARTESIAN_POINT('Ctrl Pts',(-0.23019006072046,0.00509814736951133,
0.0104776704819747));
#29728=CARTESIAN_POINT('Ctrl Pts',(-0.230146256556025,0.00514621562505539,
0.0104902514094645));
#29729=CARTESIAN_POINT('Ctrl Pts',(-0.230102294680889,0.00519427998360542,
0.0105023779101023));
#29730=CARTESIAN_POINT('Ctrl Pts',(-0.230058207604929,0.00524236841651574,
0.0105140660125324));
#29731=CARTESIAN_POINT('Ctrl Pts',(-0.229815853576752,0.00550671857289634,
0.0105783174659109));
#29732=CARTESIAN_POINT('Ctrl Pts',(-0.229569716846853,0.00577172916293637,
0.0106294062710768));
#29733=CARTESIAN_POINT('Ctrl Pts',(-0.229322739274083,0.00603943600898884,
0.0106683693245468));
#29734=CARTESIAN_POINT('',(-0.227049077441917,0.00230637883574136,0.00906391893415159));
#29735=CARTESIAN_POINT('Ctrl Pts',(-0.227049077441917,0.00230637883574136,
0.00906391893415159));
#29736=CARTESIAN_POINT('Ctrl Pts',(-0.227073318810987,0.00238431864578963,
0.00912046235057106));
#29737=CARTESIAN_POINT('Ctrl Pts',(-0.227097908747937,0.00246328116075861,
0.00917575105202224));
#29738=CARTESIAN_POINT('Ctrl Pts',(-0.227123536768961,0.00254286828211047,
0.00922963379678905));
#29739=CARTESIAN_POINT('Ctrl Pts',(-0.227161978800496,0.00266224896413825,
0.00931045791393928));
#29740=CARTESIAN_POINT('Ctrl Pts',(-0.22720277011395,0.00278302753188814,
0.00938814177886813));
#29741=CARTESIAN_POINT('Ctrl Pts',(-0.227248074883203,0.00290385325814463,
0.00946217390253985));
#29742=CARTESIAN_POINT('Ctrl Pts',(-0.227270727267829,0.00296426612127288,
0.00949918996437571));
#29743=CARTESIAN_POINT('Ctrl Pts',(-0.227294504627205,0.00302469536767607,
0.00953528337842167));
#29744=CARTESIAN_POINT('Ctrl Pts',(-0.227319648794279,0.00308496613435269,
0.0095703826343294));
#29745=CARTESIAN_POINT('Ctrl Pts',(-0.227334570957018,0.00312073467606119,
0.00959121278579584));
#29746=CARTESIAN_POINT('Ctrl Pts',(-0.227349973334997,0.00315644549335353,
0.00961169177662436));
#29747=CARTESIAN_POINT('Ctrl Pts',(-0.227365903473589,0.00319205925221374,
0.00963181686044552));
#29748=CARTESIAN_POINT('Ctrl Pts',(-0.227376815963193,0.00321645544758186,
0.00964560297829475));
#29749=CARTESIAN_POINT('Ctrl Pts',(-0.227387975997183,0.00324080613667955,
0.00965922305709978));
#29750=CARTESIAN_POINT('Ctrl Pts',(-0.227399366335057,0.00326510564441096,
0.00967268198785667));
#29751=CARTESIAN_POINT('Ctrl Pts',(-0.22747408111678,0.00342449796765148,
0.00976096567925429));
#29752=CARTESIAN_POINT('Ctrl Pts',(-0.22755866523419,0.00358193498187751,
0.00984210870278841));
#29753=CARTESIAN_POINT('Ctrl Pts',(-0.227649842528156,0.00373843387538247,
0.0099172547990377));
#29754=CARTESIAN_POINT('Ctrl Pts',(-0.227672636851648,0.00377755859875871,
0.00993604132310003));
#29755=CARTESIAN_POINT('Ctrl Pts',(-0.227695847168838,0.00381662280291635,
0.00995445193258686));
#29756=CARTESIAN_POINT('Ctrl Pts',(-0.227719428568754,0.00385563862870273,
0.00997250248056532));
#29757=CARTESIAN_POINT('Ctrl Pts',(-0.22778372902646,0.00396202482565283,
0.0100217217169544));
#29758=CARTESIAN_POINT('Ctrl Pts',(-0.227850789121976,0.00406806057251539,
0.0100682649261601));
#29759=CARTESIAN_POINT('Ctrl Pts',(-0.227919727715055,0.00417393025766419,
0.0101124421201561));
#29760=CARTESIAN_POINT('Ctrl Pts',(-0.227926636258577,0.00418453977687389,
0.0101168692494866));
#29761=CARTESIAN_POINT('Ctrl Pts',(-0.227933563697047,0.00419514762293024,
0.0101212725626095));
#29762=CARTESIAN_POINT('Ctrl Pts',(-0.227940510167508,0.00420575413544571,
0.0101256523527859));
#29763=CARTESIAN_POINT('Ctrl Pts',(-0.228042194869883,0.00436101572828531,
0.0101897651512286));
#29764=CARTESIAN_POINT('Ctrl Pts',(-0.22814789616919,0.00451584292166484,
0.0102489334827523));
#29765=CARTESIAN_POINT('Ctrl Pts',(-0.228257151826692,0.00467012000595043,
0.0103032405028755));
#29766=CARTESIAN_POINT('Ctrl Pts',(-0.228369821723491,0.00482921824911995,
0.0103592446173776));
#29767=CARTESIAN_POINT('Ctrl Pts',(-0.228486270611578,0.00498772752812297,
0.0104100777128712));
#29768=CARTESIAN_POINT('Ctrl Pts',(-0.228605950089108,0.00514546659205433,
0.010456041453186));
#29769=CARTESIAN_POINT('Ctrl Pts',(-0.228834429091665,0.00544660480501419,
0.0105437904119689));
#29770=CARTESIAN_POINT('Ctrl Pts',(-0.229074679740743,0.00574486937382215,
0.0106139556888789));
#29771=CARTESIAN_POINT('Ctrl Pts',(-0.229322729007605,0.00603936778416517,
0.0106687795114693));
#29772=CARTESIAN_POINT('',(-0.226264593472374,0.00233548629481926,0.00906884038940272));
#29773=CARTESIAN_POINT('Ctrl Pts',(-0.226264593480196,0.00233548634321754,
0.0090688404173902));
#29774=CARTESIAN_POINT('Ctrl Pts',(-0.226394576944157,0.00231954970168914,
0.00906006960165041));
#29775=CARTESIAN_POINT('Ctrl Pts',(-0.226525406606473,0.00230915152537602,
0.00905517566549868));
#29776=CARTESIAN_POINT('Ctrl Pts',(-0.226787422427741,0.00229941738241652,
0.0090533391772081));
#29777=CARTESIAN_POINT('Ctrl Pts',(-0.226918425715393,0.00230006314209026,
0.00905638008239629));
#29778=CARTESIAN_POINT('Ctrl Pts',(-0.227049047294151,0.00230621211406783,
0.00906336897528621));
#29779=CARTESIAN_POINT('',(-0.226391079625555,0.00186369918572083,0.00871144032068667));
#29780=CARTESIAN_POINT('Origin',(-0.227683792439033,0.00776639667921597,
0.00188953853444711));
#29781=CARTESIAN_POINT('',(-0.225391399225421,0.00186320400051213,0.00869213916568744));
#29782=CARTESIAN_POINT('Ctrl Pts',(-0.225391399225484,0.00186320400486124,
0.00869213916233772));
#29783=CARTESIAN_POINT('Ctrl Pts',(-0.225558023686355,0.00186328774236531,
0.00869535478842071));
#29784=CARTESIAN_POINT('Ctrl Pts',(-0.225724648220415,0.00186337087834226,
0.00869857114170172));
#29785=CARTESIAN_POINT('Ctrl Pts',(-0.226057875023074,0.0018635359380542,
0.00870500486370907));
#29786=CARTESIAN_POINT('Ctrl Pts',(-0.226224477410293,0.00186361786200745,
0.00870822223453359));
#29787=CARTESIAN_POINT('Ctrl Pts',(-0.226391079625542,0.00186369918634654,
0.00871144032136585));
#29788=CARTESIAN_POINT('',(-0.225269616388151,0.00232397772164353,0.0090411714391037));
#29789=CARTESIAN_POINT('Origin',(-0.226735468554244,0.0077654556471817,
0.00187401233671198));
#29790=CARTESIAN_POINT('',(-0.225014720871232,0.00228334524727118,0.0090072968842552));
#29791=CARTESIAN_POINT('Ctrl Pts',(-0.225014708918058,0.00228338321464125,
0.00900698417674001));
#29792=CARTESIAN_POINT('Ctrl Pts',(-0.225058707715989,0.0022804931552636,
0.00900576569532436));
#29793=CARTESIAN_POINT('Ctrl Pts',(-0.2251029310297,0.00228252149587852,
0.00900809763828351));
#29794=CARTESIAN_POINT('Ctrl Pts',(-0.225188483608375,0.00229619488802783,
0.00901960729698031));
#29795=CARTESIAN_POINT('Ctrl Pts',(-0.225229440181929,0.00230758548139352,
0.00902859347934716));
#29796=CARTESIAN_POINT('Ctrl Pts',(-0.225267894528976,0.00232332530843618,
0.00904055895880893));
#29797=CARTESIAN_POINT('',(-0.22511807106961,0.0030194940701125,0.00948730014603764));
#29798=CARTESIAN_POINT('Ctrl Pts',(-0.225117921444226,0.00301994314685244,
0.00948650676310671));
#29799=CARTESIAN_POINT('Ctrl Pts',(-0.225116735324925,0.00296209933042116,
0.00945287844947561));
#29800=CARTESIAN_POINT('Ctrl Pts',(-0.225114046175496,0.00290467972170827,
0.00941860289759098));
#29801=CARTESIAN_POINT('Ctrl Pts',(-0.225104870506897,0.00277996152311542,
0.00934219611760584));
#29802=CARTESIAN_POINT('Ctrl Pts',(-0.225097762701751,0.00271289768830998,
0.00929983343525847));
#29803=CARTESIAN_POINT('Ctrl Pts',(-0.225071275977785,0.00252250121128088,
0.00917591424648294));
#29804=CARTESIAN_POINT('Ctrl Pts',(-0.225046633679134,0.00240132284164297,
0.00909253401528519));
#29805=CARTESIAN_POINT('Ctrl Pts',(-0.225014708541206,0.00228344637870765,
0.00900702965187676));
#29806=CARTESIAN_POINT('',(-0.225092272969296,0.00749505820794686,0.0106947832387151));
#29807=CARTESIAN_POINT('Ctrl Pts',(-0.225092270893944,0.00749505808259213,
0.0106948888771213));
#29808=CARTESIAN_POINT('Ctrl Pts',(-0.225024225129317,0.00671188196061008,
0.0106929144122287));
#29809=CARTESIAN_POINT('Ctrl Pts',(-0.224968404063802,0.00593093008167228,
0.0105880278895065));
#29810=CARTESIAN_POINT('Ctrl Pts',(-0.224963126040131,0.0051742066094581,
0.0103830238688901));
#29811=CARTESIAN_POINT('Ctrl Pts',(-0.224957869409366,0.00442055029181519,
0.0101788507713812));
#29812=CARTESIAN_POINT('Ctrl Pts',(-0.225002247330816,0.00369017725769303,
0.00987507507293168));
#29813=CARTESIAN_POINT('Ctrl Pts',(-0.22511807106961,0.0030194940701125,
0.00948730014603765));
#29814=CARTESIAN_POINT('',(-0.225114795773928,0.0119223070838394,0.00952049564286698));
#29815=CARTESIAN_POINT('Ctrl Pts',(-0.225114724781785,0.0119219979226124,
0.00951993302627938));
#29816=CARTESIAN_POINT('Ctrl Pts',(-0.225003084530341,0.0112547568345833,
0.00989797239668878));
#29817=CARTESIAN_POINT('Ctrl Pts',(-0.224963984333154,0.0105350672611751,
0.0101933029905569));
#29818=CARTESIAN_POINT('Ctrl Pts',(-0.224969552040664,0.0097879845343096,
0.0103925472293563));
#29819=CARTESIAN_POINT('Ctrl Pts',(-0.224971338108729,0.00954832744052368,
0.0104564629022893));
#29820=CARTESIAN_POINT('Ctrl Pts',(-0.22497772631488,0.00930594816711339,
0.0105104728615714));
#29821=CARTESIAN_POINT('Ctrl Pts',(-0.224987788152167,0.0090617312619527,
0.0105541768374275));
#29822=CARTESIAN_POINT('Ctrl Pts',(-0.225009092495973,0.00854464071849152,
0.0106467130711986));
#29823=CARTESIAN_POINT('Ctrl Pts',(-0.225046866204789,0.00801931179304763,
0.0106930084471554));
#29824=CARTESIAN_POINT('Ctrl Pts',(-0.225092297269035,0.00749505967569209,
0.0106935463466661));
#29825=CARTESIAN_POINT('',(-0.22499258838655,0.0127125317992707,0.00900988833309594));
#29826=CARTESIAN_POINT('Ctrl Pts',(-0.224991938877462,0.0127124272395741,
0.00900994896083489));
#29827=CARTESIAN_POINT('Ctrl Pts',(-0.225025552074485,0.0125862881553428,
0.00910138340065515));
#29828=CARTESIAN_POINT('Ctrl Pts',(-0.225052649372304,0.0124566919536995,
0.00919011728944026));
#29829=CARTESIAN_POINT('Ctrl Pts',(-0.225084070350122,0.0122533061865343,
0.00932132006962372));
#29830=CARTESIAN_POINT('Ctrl Pts',(-0.225093106140568,0.0121818687796175,
0.00936595433272495));
#29831=CARTESIAN_POINT('Ctrl Pts',(-0.225106409122268,0.0120476391460597,
0.00944712668901661));
#29832=CARTESIAN_POINT('Ctrl Pts',(-0.225111167725843,0.0119850807081392,
0.00948390081391465));
#29833=CARTESIAN_POINT('Ctrl Pts',(-0.225114536864462,0.0119220042196567,
0.00951992555793149));
#29834=CARTESIAN_POINT('',(-0.225275995996774,0.0126688942355271,0.00904667010172663));
#29835=CARTESIAN_POINT('Ctrl Pts',(-0.225275292269729,0.0126691944030332,
0.0090464420147403));
#29836=CARTESIAN_POINT('Ctrl Pts',(-0.22523224496111,0.0126875448165675,
0.00903254829052764));
#29837=CARTESIAN_POINT('Ctrl Pts',(-0.22518604351654,0.0127005646461434,
0.00902228805289712));
#29838=CARTESIAN_POINT('Ctrl Pts',(-0.225090148450807,0.0127152484784252,
0.00900984944409604));
#29839=CARTESIAN_POINT('Ctrl Pts',(-0.22504098157506,0.0127167959862583,
0.00900776711024177));
#29840=CARTESIAN_POINT('Ctrl Pts',(-0.224992260310303,0.01271250203545,
0.00900990144007799));
#29841=CARTESIAN_POINT('',(-0.225398010193384,0.013120318400212,0.00870574369815946));
#29842=CARTESIAN_POINT('Ctrl Pts',(-0.225397991300964,0.0131202941880968,
0.00870570880811002));
#29843=CARTESIAN_POINT('Ctrl Pts',(-0.225376967217776,0.013046681933572,
0.00876512827360961));
#29844=CARTESIAN_POINT('Ctrl Pts',(-0.225356173079467,0.0129720714761437,
0.00882339220392176));
#29845=CARTESIAN_POINT('Ctrl Pts',(-0.225315267761045,0.0128216609209388,
0.008936973809279));
#29846=CARTESIAN_POINT('Ctrl Pts',(-0.225295147418202,0.0127458635364527,
0.00899232711753521));
#29847=CARTESIAN_POINT('Ctrl Pts',(-0.225275261888314,0.0126691065284336,
0.00904650388940398));
#29848=CARTESIAN_POINT('',(-0.226397825284883,0.0131187534369297,0.00872595188639632));
#29849=CARTESIAN_POINT('Ctrl Pts',(-0.226397825264573,0.0131187211963479,
0.00872592705145478));
#29850=CARTESIAN_POINT('Ctrl Pts',(-0.226231196957561,0.0131189815906668,
0.00872255626913465));
#29851=CARTESIAN_POINT('Ctrl Pts',(-0.22606456844847,0.0131192426581214,
0.00871918629101479));
#29852=CARTESIAN_POINT('Ctrl Pts',(-0.22573129369429,0.0131197661684618,
0.00871244760079479));
#29853=CARTESIAN_POINT('Ctrl Pts',(-0.22556464732301,0.0131200286116902,
0.00870907888631731));
#29854=CARTESIAN_POINT('Ctrl Pts',(-0.225398001030979,0.0131202917297391,
0.00870571098993131));
#29855=CARTESIAN_POINT('',(-0.226273558818709,0.0126615507097427,0.00907157974325745));
#29856=CARTESIAN_POINT('Ctrl Pts',(-0.226273546976328,0.0126614891951054,
0.00907159303692138));
#29857=CARTESIAN_POINT('Ctrl Pts',(-0.226293819248747,0.0127397767182858,
0.00901634447273793));
#29858=CARTESIAN_POINT('Ctrl Pts',(-0.226314323246947,0.0128170574252013,
0.00895987557181371));
#29859=CARTESIAN_POINT('Ctrl Pts',(-0.226355750293415,0.0129694606248348,
0.0088446407394028));
#29860=CARTESIAN_POINT('Ctrl Pts',(-0.226376675901891,0.0130446000245681,
0.00878587031714395));
#29861=CARTESIAN_POINT('Ctrl Pts',(-0.226397824863347,0.0131187249268725,
0.00872592400672208));
#29862=CARTESIAN_POINT('',(-0.227025820193335,0.0126926713729642,0.00906414398299204));
#29863=CARTESIAN_POINT('Ctrl Pts',(-0.227025585132577,0.0126930612201683,
0.00906385023298042));
#29864=CARTESIAN_POINT('Ctrl Pts',(-0.226900285105079,0.0126994640941745,
0.0090567813192604));
#29865=CARTESIAN_POINT('Ctrl Pts',(-0.226774554286507,0.0127000381325738,
0.00905389459328833));
#29866=CARTESIAN_POINT('Ctrl Pts',(-0.226523261898834,0.0126895110571021,
0.00905651128120664));
#29867=CARTESIAN_POINT('Ctrl Pts',(-0.226397912137852,0.0126784000805961,
0.00906202567587128));
#29868=CARTESIAN_POINT('Ctrl Pts',(-0.226273566680661,0.0126614379936754,
0.00907162982036916));
#29869=CARTESIAN_POINT('',(-0.229319783972502,0.00893282155661927,0.0106733201854368));
#29870=CARTESIAN_POINT('Ctrl Pts',(-0.227025820193335,0.0126926713729642,
0.00906414398299204));
#29871=CARTESIAN_POINT('Ctrl Pts',(-0.227144422003088,0.0123844750755602,
0.00928810910664895));
#29872=CARTESIAN_POINT('Ctrl Pts',(-0.227378539637632,0.0117345865363843,
0.00969884466117373));
#29873=CARTESIAN_POINT('Ctrl Pts',(-0.228060574676232,0.0104466400243243,
0.0103068898455848));
#29874=CARTESIAN_POINT('Ctrl Pts',(-0.228822775788018,0.00954435960659404,
0.0105618645719844));
#29875=CARTESIAN_POINT('Ctrl Pts',(-0.229319782742692,0.00893282246601824,
0.0106733200063927));
#29876=CARTESIAN_POINT('Ctrl Pts',(-0.225870784240265,0.0163857105469993,
0.00232295787970897));
#29877=CARTESIAN_POINT('Ctrl Pts',(-0.225984689281823,0.0163678565223796,
0.00256925331663685));
#29878=CARTESIAN_POINT('Ctrl Pts',(-0.226270571940394,0.0163157306273066,
0.00313797237727359));
#29879=CARTESIAN_POINT('Ctrl Pts',(-0.226951825491954,0.0160791515514167,
0.00430595120672089));
#29880=CARTESIAN_POINT('Ctrl Pts',(-0.228041504483085,0.0155725225710242,
0.00569876179429522));
#29881=CARTESIAN_POINT('Ctrl Pts',(-0.229307422404798,0.0148998081355142,
0.00684612386700789));
#29882=CARTESIAN_POINT('Ctrl Pts',(-0.230375603478029,0.0142953788605102,
0.00764921276950633));
#29883=CARTESIAN_POINT('Ctrl Pts',(-0.231144606670057,0.0137796598506574,
0.00823050330807649));
#29884=CARTESIAN_POINT('Ctrl Pts',(-0.231717625303835,0.0132437427585838,
0.0087371891906484));
#29885=CARTESIAN_POINT('Ctrl Pts',(-0.231921495045492,0.0126777290387282,
0.00917894991078855));
#29886=CARTESIAN_POINT('Ctrl Pts',(-0.231856609050107,0.0120617879112867,
0.00959326671503007));
#29887=CARTESIAN_POINT('Ctrl Pts',(-0.231418479104261,0.0113315161178985,
0.00998183278666155));
#29888=CARTESIAN_POINT('Ctrl Pts',(-0.230760643568965,0.0105292050159737,
0.0103024614441315));
#29889=CARTESIAN_POINT('Ctrl Pts',(-0.230052352200966,0.00973441143097333,
0.0105331538057983));
#29890=CARTESIAN_POINT('Ctrl Pts',(-0.229564237344982,0.00920073542775872,
0.0106348601580364));
#29891=CARTESIAN_POINT('Ctrl Pts',(-0.229319785796903,0.00893282051848101,
0.0106733203943486));
#29892=CARTESIAN_POINT('',(-0.228033577259201,0.00748440686309334,0.0107613524025277));
#29893=CARTESIAN_POINT('',(-0.225970976589886,0.0102590377499324,0.010274952813057));
#29894=CARTESIAN_POINT('Ctrl Pts',(-0.225971973667151,0.0102581014536471,
0.0102752892966652));
#29895=CARTESIAN_POINT('Ctrl Pts',(-0.226258957253418,0.00981106287023984,
0.0104276655150511));
#29896=CARTESIAN_POINT('Ctrl Pts',(-0.226565327801358,0.00936526590846451,
0.0105414574236971));
#29897=CARTESIAN_POINT('Ctrl Pts',(-0.227252132952874,0.00843377550683359,
0.0107077786319585));
#29898=CARTESIAN_POINT('Ctrl Pts',(-0.227634704870478,0.00795248948585582,
0.0107518722875852));
#29899=CARTESIAN_POINT('Ctrl Pts',(-0.228035368651552,0.00748592054835535,
0.0107600046111732));
#29900=CARTESIAN_POINT('',(-0.226096198836323,0.00749455293783961,0.0107162203443074));
#29901=CARTESIAN_POINT('Ctrl Pts',(-0.226096198887514,0.0074945529422081,
0.0107162197568569));
#29902=CARTESIAN_POINT('Ctrl Pts',(-0.226045613969429,0.00800129271977726,
0.0107155800038505));
#29903=CARTESIAN_POINT('Ctrl Pts',(-0.226007580575707,0.0085095391841719,
0.0106722483098859));
#29904=CARTESIAN_POINT('Ctrl Pts',(-0.225976278112083,0.00923709836231164,
0.0105462751057775));
#29905=CARTESIAN_POINT('Ctrl Pts',(-0.225969942789085,0.00946159749189918,
0.0104982904773385));
#29906=CARTESIAN_POINT('Ctrl Pts',(-0.225965415311814,0.00987711744646229,
0.0103926336528987));
#29907=CARTESIAN_POINT('Ctrl Pts',(-0.225966264872201,0.0100685014222969,
0.0103371128225748));
#29908=CARTESIAN_POINT('Ctrl Pts',(-0.225970496220548,0.0102577785740447,
0.0102753623938262));
#29909=CARTESIAN_POINT('',(-0.225969628990936,0.00470142166790465,0.010263376289086));
#29910=CARTESIAN_POINT('Ctrl Pts',(-0.225968196058152,0.0047015146234352,
0.0102629949238911));
#29911=CARTESIAN_POINT('Ctrl Pts',(-0.225963828387184,0.0048913841275601,
0.01032589169753));
#29912=CARTESIAN_POINT('Ctrl Pts',(-0.225962903267804,0.00508303187486879,
0.0103823036863443));
#29913=CARTESIAN_POINT('Ctrl Pts',(-0.225967406633248,0.00550189479405183,
0.0104902436772195));
#29914=CARTESIAN_POINT('Ctrl Pts',(-0.22597386328584,0.00572895222895801,
0.0105393361889391));
#29915=CARTESIAN_POINT('Ctrl Pts',(-0.226005775090408,0.00646530387556126,
0.0106689593848215));
#29916=CARTESIAN_POINT('Ctrl Pts',(-0.226044659416343,0.00698069636745237,
0.0107145458902014));
#29917=CARTESIAN_POINT('Ctrl Pts',(-0.226096198875693,0.00749455293580526,
0.0107162197565836));
#29918=CARTESIAN_POINT('Ctrl Pts',(-0.22803357693545,0.0074844064806642,
0.0107613523945308));
#29919=CARTESIAN_POINT('Ctrl Pts',(-0.228009905277726,0.00745644439420555,
0.0107607676415092));
#29920=CARTESIAN_POINT('Ctrl Pts',(-0.227986276934626,0.00742844114892991,
0.0107600533973566));
#29921=CARTESIAN_POINT('Ctrl Pts',(-0.227962694037332,0.0074003983292184,
0.0107592078475071));
#29922=CARTESIAN_POINT('Ctrl Pts',(-0.227854134533825,0.00727130839820451,
0.0107553155152501));
#29923=CARTESIAN_POINT('Ctrl Pts',(-0.227747285397279,0.00714229162262032,
0.0107486933562038));
#29924=CARTESIAN_POINT('Ctrl Pts',(-0.227640411533435,0.00701114238092464,
0.0107390484382944));
#29925=CARTESIAN_POINT('Ctrl Pts',(-0.227573160013985,0.00692861532087877,
0.0107329792707631));
#29926=CARTESIAN_POINT('Ctrl Pts',(-0.227506577326311,0.0068461340379774,
0.0107257649510492));
#29927=CARTESIAN_POINT('Ctrl Pts',(-0.227440527701029,0.00676345650279847,
0.0107173671751193));
#29928=CARTESIAN_POINT('Ctrl Pts',(-0.227429839358583,0.0067500773836158,
0.0107160082225962));
#29929=CARTESIAN_POINT('Ctrl Pts',(-0.227419164145874,0.00673669198469641,
0.0107146181614928));
#29930=CARTESIAN_POINT('Ctrl Pts',(-0.227408502408266,0.00672330030514739,
0.0107131968807224));
#29931=CARTESIAN_POINT('Ctrl Pts',(-0.227398507029259,0.00671074560557031,
0.0107118644300003));
#29932=CARTESIAN_POINT('Ctrl Pts',(-0.227388523493641,0.00669818538584928,
0.010710504540147));
#29933=CARTESIAN_POINT('Ctrl Pts',(-0.227378552094813,0.00668561963553653,
0.0107091171207398));
#29934=CARTESIAN_POINT('Ctrl Pts',(-0.227344969296733,0.00664329928883968,
0.0107044444136701));
#29935=CARTESIAN_POINT('Ctrl Pts',(-0.227311528164211,0.00660092147569552,
0.0106994594641931));
#29936=CARTESIAN_POINT('Ctrl Pts',(-0.227278249873491,0.00655849689293043,
0.0106941607624104));
#29937=CARTESIAN_POINT('Ctrl Pts',(-0.227169961041194,0.00642044567608853,
0.0106769185839114));
#29938=CARTESIAN_POINT('Ctrl Pts',(-0.227063128893779,0.00628157692716777,
0.0106563233522903));
#29939=CARTESIAN_POINT('Ctrl Pts',(-0.226958472966203,0.0061419247782648,
0.0106322636464153));
#29940=CARTESIAN_POINT('Ctrl Pts',(-0.226952048338015,0.00613335179866265,
0.0106307866668678));
#29941=CARTESIAN_POINT('Ctrl Pts',(-0.226945632209316,0.00612477610935256,
0.0106292966723998));
#29942=CARTESIAN_POINT('Ctrl Pts',(-0.226939224866442,0.00611619781009488,
0.0106277936487921));
#29943=CARTESIAN_POINT('Ctrl Pts',(-0.226897570156155,0.00606042951777538,
0.0106180223576068));
#29944=CARTESIAN_POINT('Ctrl Pts',(-0.226855528870052,0.00600352434119545,
0.0106075108508253));
#29945=CARTESIAN_POINT('Ctrl Pts',(-0.226814483144495,0.00594725365858661,
0.0105965730065991));
#29946=CARTESIAN_POINT('Ctrl Pts',(-0.226770108470221,0.00588641923117389,
0.010584748065799));
#29947=CARTESIAN_POINT('Ctrl Pts',(-0.226727370143022,0.00582698986468138,
0.0105725911069167));
#29948=CARTESIAN_POINT('Ctrl Pts',(-0.226684141557327,0.00576593664027173,
0.0105594687640135));
#29949=CARTESIAN_POINT('Ctrl Pts',(-0.226652936231869,0.00572186428149994,
0.0105499961667847));
#29950=CARTESIAN_POINT('Ctrl Pts',(-0.226621988893697,0.00567768823496359,
0.0105401693083525));
#29951=CARTESIAN_POINT('Ctrl Pts',(-0.226591267477624,0.00563343719839793,
0.0105299865603063));
#29952=CARTESIAN_POINT('Ctrl Pts',(-0.226577826858092,0.00561407736990039,
0.0105255316080361));
#29953=CARTESIAN_POINT('Ctrl Pts',(-0.226564429604295,0.00559470309431951,
0.010521008528986));
#29954=CARTESIAN_POINT('Ctrl Pts',(-0.226551073458115,0.00557531642343092,
0.0105164171576264));
#29955=CARTESIAN_POINT('Ctrl Pts',(-0.226538552071071,0.00555714141947307,
0.0105121127469768));
#29956=CARTESIAN_POINT('Ctrl Pts',(-0.226526066816743,0.0055389555183428,
0.0105077483136463));
#29957=CARTESIAN_POINT('Ctrl Pts',(-0.226513615992729,0.00552076028083763,
0.010503323707922));
#29958=CARTESIAN_POINT('Ctrl Pts',(-0.226473450913159,0.00546206431329363,
0.0104890503842619));
#29959=CARTESIAN_POINT('Ctrl Pts',(-0.226432631356042,0.00540176900244369,
0.0104737572539422));
#29960=CARTESIAN_POINT('Ctrl Pts',(-0.226393664287511,0.00534371303495483,
0.0104584291238958));
#29961=CARTESIAN_POINT('Ctrl Pts',(-0.226367644141469,0.00530494633246592,
0.0104481938098889));
#29962=CARTESIAN_POINT('Ctrl Pts',(-0.226343230956819,0.00526837461445328,
0.0104382944101526));
#29963=CARTESIAN_POINT('Ctrl Pts',(-0.226316946251662,0.00522874762316253,
0.0104272855401428));
#29964=CARTESIAN_POINT('Ctrl Pts',(-0.226291077207928,0.00518974728571816,
0.0104164507623493));
#29965=CARTESIAN_POINT('Ctrl Pts',(-0.226264206467458,0.00514903911302078,
0.0104048478061562));
#29966=CARTESIAN_POINT('Ctrl Pts',(-0.226238708504583,0.00511034574189367,
0.0103935371682146));
#29967=CARTESIAN_POINT('Ctrl Pts',(-0.226233205333744,0.00510199463429003,
0.0103910960173982));
#29968=CARTESIAN_POINT('Ctrl Pts',(-0.226227700333222,0.00509363746989984,
0.0103886398549127));
#29969=CARTESIAN_POINT('Ctrl Pts',(-0.226222196488384,0.00508527941953711,
0.0103861702923412));
#29970=CARTESIAN_POINT('Ctrl Pts',(-0.226182592689434,0.00502513772659641,
0.010368400158467));
#29971=CARTESIAN_POINT('Ctrl Pts',(-0.226143231315418,0.00496523360787539,
0.010350032573918));
#29972=CARTESIAN_POINT('Ctrl Pts',(-0.226103876677456,0.00490537822662242,
0.0103309871000461));
#29973=CARTESIAN_POINT('Ctrl Pts',(-0.226081464749338,0.00487129140556136,
0.0103201409631357));
#29974=CARTESIAN_POINT('Ctrl Pts',(-0.226059075388918,0.00483724771525806,
0.0103090842351201));
#29975=CARTESIAN_POINT('Ctrl Pts',(-0.226036702403961,0.0048032531669151,
0.0102978161090545));
#29976=CARTESIAN_POINT('Ctrl Pts',(-0.226025515911483,0.004786255892744,
0.0102921820460218));
#29977=CARTESIAN_POINT('Ctrl Pts',(-0.226014333561778,0.00476927087634384,
0.0102864951249411));
#29978=CARTESIAN_POINT('Ctrl Pts',(-0.226003154809509,0.00475229874089972,
0.0102807552003522));
#29979=CARTESIAN_POINT('Ctrl Pts',(-0.225997565433375,0.00474381267317885,
0.0102778852380582));
#29980=CARTESIAN_POINT('Ctrl Pts',(-0.225991976958479,0.00473532982465564,
0.0102750020244736));
#29981=CARTESIAN_POINT('Ctrl Pts',(-0.225986389326614,0.0047268502677692,
0.0102721055390739));
#29982=CARTESIAN_POINT('Ctrl Pts',(-0.225980801694748,0.00471837071088277,
0.0102692090536741));
#29983=CARTESIAN_POINT('Ctrl Pts',(-0.225975214905513,0.0047098944449384,
0.0102662992960872));
#29984=CARTESIAN_POINT('Ctrl Pts',(-0.225969628990936,0.00470142166790475,
0.0102633762890857));
#29985=CARTESIAN_POINT('',(-0.226096178744282,0.00750540343988805,-0.0107162180661903));
#29986=CARTESIAN_POINT('',(-0.225967411913371,0.0102623479612313,-0.0102748686137305));
#29987=CARTESIAN_POINT('Ctrl Pts',(-0.225967387201314,0.0102611633020894,
-0.0102752620305393));
#29988=CARTESIAN_POINT('Ctrl Pts',(-0.225963503316852,0.0100728173574592,
-0.010336734102349));
#29989=CARTESIAN_POINT('Ctrl Pts',(-0.22596296794087,0.00988279893284449,
-0.0103918116764779));
#29990=CARTESIAN_POINT('Ctrl Pts',(-0.22596813343084,0.00946801496741777,
-0.0104970323863582));
#29991=CARTESIAN_POINT('Ctrl Pts',(-0.225974821774181,0.00924339636561263,
-0.0105448231600401));
#29992=CARTESIAN_POINT('Ctrl Pts',(-0.226007053817059,0.00851770773012774,
-0.0106704459522781));
#29993=CARTESIAN_POINT('Ctrl Pts',(-0.226045487878963,0.00801086921392995,
-0.0107145664926717));
#29994=CARTESIAN_POINT('Ctrl Pts',(-0.226096168126154,0.00750551040622462,
-0.0107162162799583));
#29995=CARTESIAN_POINT('',(-0.228054819889722,0.00748068141568947,-0.0107604444270658));
#29996=CARTESIAN_POINT('Ctrl Pts',(-0.228054819890027,0.00748068141595342,
-0.0107604444270559));
#29997=CARTESIAN_POINT('Ctrl Pts',(-0.227652037218058,0.00794552320395912,
-0.0107521683783107));
#29998=CARTESIAN_POINT('Ctrl Pts',(-0.227267804242261,0.00842519382017008,
-0.0107081952621097));
#29999=CARTESIAN_POINT('Ctrl Pts',(-0.226574304617479,0.00935827291019254,
-0.0105431611063224));
#30000=CARTESIAN_POINT('Ctrl Pts',(-0.226262051637222,0.00980918637230702,
-0.0104294968164533));
#30001=CARTESIAN_POINT('Ctrl Pts',(-0.225968440683985,0.0102619875384845,
-0.0102750157142978));
#30002=CARTESIAN_POINT('',(-0.225972184946916,0.00467377596756055,-0.010252770733025));
#30003=CARTESIAN_POINT('Ctrl Pts',(-0.225973609942387,0.00467436557371437,
-0.0102529563829087));
#30004=CARTESIAN_POINT('Ctrl Pts',(-0.226285458894388,0.00517297659214837,
-0.0104271136615909));
#30005=CARTESIAN_POINT('Ctrl Pts',(-0.226623269987956,0.00566740906512651,
-0.0105522882614033));
#30006=CARTESIAN_POINT('Ctrl Pts',(-0.227329537494644,0.0066117069902153,
-0.0107122048385642));
#30007=CARTESIAN_POINT('Ctrl Pts',(-0.227687882265678,0.00704950453591529,
-0.0107513952059892));
#30008=CARTESIAN_POINT('Ctrl Pts',(-0.228054819889427,0.00748068141594102,
-0.0107604444270423));
#30009=CARTESIAN_POINT('Ctrl Pts',(-0.226096200187826,0.00750540266069626,
-0.0107162171111456));
#30010=CARTESIAN_POINT('Ctrl Pts',(-0.226044299402367,0.00698548623471811,
-0.0107155583402523));
#30011=CARTESIAN_POINT('Ctrl Pts',(-0.226005601313484,0.00646398203969811,
-0.0106699545805781));
#30012=CARTESIAN_POINT('Ctrl Pts',(-0.225974806245419,0.00571858163159882,
-0.0105374320042732));
#30013=CARTESIAN_POINT('Ctrl Pts',(-0.225968822940153,0.00548862267467334,
-0.0104869806370106));
#30014=CARTESIAN_POINT('Ctrl Pts',(-0.225965434348515,0.00506386537530727,
-0.0103761076146514));
#30015=CARTESIAN_POINT('Ctrl Pts',(-0.225966991269723,0.00486851066308794,
-0.010317937672268));
#30016=CARTESIAN_POINT('Ctrl Pts',(-0.225972142300558,0.00467541771917558,
-0.0102532772611998));
#30017=CARTESIAN_POINT('Ctrl Pts',(-0.224903047769934,0.0163974953490442,
0.00232527569536224));
#30018=CARTESIAN_POINT('Ctrl Pts',(-0.228003678801843,0.0163652528946496,
0.00231821622721085));
#30019=CARTESIAN_POINT('Ctrl Pts',(-0.23110431006382,0.0163330357098684,
0.00231114482972889));
#30020=CARTESIAN_POINT('Ctrl Pts',(-0.234204941533998,0.0163008422866106,
0.00230405918705812));
#30021=CARTESIAN_POINT('Ctrl Pts',(-0.224902923051373,0.016421905903896,
0.001999690061282));
#30022=CARTESIAN_POINT('Ctrl Pts',(-0.228003554472057,0.0163857948128496,
0.00199154431614981));
#30023=CARTESIAN_POINT('Ctrl Pts',(-0.231104186130884,0.0163497065102629,
0.00198339075959686));
#30024=CARTESIAN_POINT('Ctrl Pts',(-0.23420481801057,0.0163136399270852,
0.00197522735965944));
#30025=CARTESIAN_POINT('Ctrl Pts',(-0.224902686634519,0.0164496060066283,
0.00134999605462854));
#30026=CARTESIAN_POINT('Ctrl Pts',(-0.228003316903349,0.0164061218898441,
0.00134119319572166));
#30027=CARTESIAN_POINT('Ctrl Pts',(-0.231103947348719,0.0163626446434222,
0.00133240817680761));
#30028=CARTESIAN_POINT('Ctrl Pts',(-0.234204577993315,0.0163191760221561,
0.00132364096404516));
#30029=CARTESIAN_POINT('Ctrl Pts',(-0.22490247733934,0.0164891827557564,
8.48946422705292E-5));
#30030=CARTESIAN_POINT('Ctrl Pts',(-0.2280031047451,0.0164387037966636,
8.36968421714054E-5));
#30031=CARTESIAN_POINT('Ctrl Pts',(-0.231103732057188,0.01638822192355,
8.25020821930779E-5));
#30032=CARTESIAN_POINT('Ctrl Pts',(-0.234204359262361,0.016337735996471,
8.13110569434896E-5));
#30033=CARTESIAN_POINT('Ctrl Pts',(-0.224902601832635,0.0164577305274795,
-0.00116946331798178));
#30034=CARTESIAN_POINT('Ctrl Pts',(-0.22800323228218,0.0164115731563456,
-0.00115947279336496));
#30035=CARTESIAN_POINT('Ctrl Pts',(-0.231103862912676,0.016365419418937,
-0.00114950763219157));
#30036=CARTESIAN_POINT('Ctrl Pts',(-0.234204493754791,0.0163192718567599,
-0.00113956819841304));
#30037=CARTESIAN_POINT('Ctrl Pts',(-0.2249031047193,0.016401050271707,-0.00247428944274167));
#30038=CARTESIAN_POINT('Ctrl Pts',(-0.228003735976318,0.016370691448232,
-0.00246735407024901));
#30039=CARTESIAN_POINT('Ctrl Pts',(-0.231104367476673,0.0163403620163895,
-0.00246039974613875));
#30040=CARTESIAN_POINT('Ctrl Pts',(-0.234204999188339,0.0163100597051565,
-0.00245342363871553));
#30041=CARTESIAN_POINT('Ctrl Pts',(-0.224903620482978,0.0162331344936927,
-0.00377581649114323));
#30042=CARTESIAN_POINT('Ctrl Pts',(-0.228004247053984,0.0162183248288798,
-0.00377611183675602));
#30043=CARTESIAN_POINT('Ctrl Pts',(-0.231104873706723,0.0162035348039987,
-0.00377640360674382));
#30044=CARTESIAN_POINT('Ctrl Pts',(-0.23420550044494,0.0161887639228305,
-0.00377669038870648));
#30045=CARTESIAN_POINT('Ctrl Pts',(-0.224904244439412,0.0157454055087051,
-0.00535508843351867));
#30046=CARTESIAN_POINT('Ctrl Pts',(-0.228004869356698,0.015745877431058,
-0.00536654194974573));
#30047=CARTESIAN_POINT('Ctrl Pts',(-0.231105494288016,0.0157463686608469,
-0.00537798949180189));
#30048=CARTESIAN_POINT('Ctrl Pts',(-0.234206119236561,0.0157468784277487,
-0.00538942975580705));
#30049=CARTESIAN_POINT('Ctrl Pts',(-0.224904927056323,0.014756116525245,
-0.0070809462510311));
#30050=CARTESIAN_POINT('Ctrl Pts',(-0.228005551277712,0.0147682738612367,
-0.00710847555851588));
#30051=CARTESIAN_POINT('Ctrl Pts',(-0.231106175457583,0.0147804448844733,
-0.00713600323790223));
#30052=CARTESIAN_POINT('Ctrl Pts',(-0.234206799604821,0.014792629252247,
-0.00716352865861212));
#30053=CARTESIAN_POINT('Ctrl Pts',(-0.224905705935764,0.0129587456084716,
-0.00904270204015799));
#30054=CARTESIAN_POINT('Ctrl Pts',(-0.228006331471737,0.0129775263446935,
-0.00909152831654588));
#30055=CARTESIAN_POINT('Ctrl Pts',(-0.231106956961612,0.0129963155259409,
-0.00914035417356039));
#30056=CARTESIAN_POINT('Ctrl Pts',(-0.234207582410669,0.0130151128918419,
-0.00918917939755658));
#30057=CARTESIAN_POINT('Ctrl Pts',(-0.224906344901157,0.00996717482975785,
-0.0106558172504251));
#30058=CARTESIAN_POINT('Ctrl Pts',(-0.228006973196984,0.00997888641244874,
-0.0107253416344494));
#30059=CARTESIAN_POINT('Ctrl Pts',(-0.23110760149003,0.00999060093234777,
-0.0107948661290257));
#30060=CARTESIAN_POINT('Ctrl Pts',(-0.234208229780548,0.0100023182636535,
-0.010864390745125));
#30061=CARTESIAN_POINT('Ctrl Pts',(-0.224906421473904,0.00588448586822914,
-0.0108495989887083));
#30062=CARTESIAN_POINT('Ctrl Pts',(-0.228007050197119,0.00587660352368733,
-0.0109217704181749));
#30063=CARTESIAN_POINT('Ctrl Pts',(-0.231107678925808,0.00586871925150363,
-0.0109939418074081));
#30064=CARTESIAN_POINT('Ctrl Pts',(-0.23420830765933,0.00586083314294305,
-0.0110661131658069));
#30065=CARTESIAN_POINT('Ctrl Pts',(-0.224905896797368,0.00275206275993148,
-0.00952499259309634));
#30066=CARTESIAN_POINT('Ctrl Pts',(-0.22800652301585,0.00273399542249794,
-0.00957977151548));
#30067=CARTESIAN_POINT('Ctrl Pts',(-0.231107149196805,0.00271592133715538,
-0.00963455045765119));
#30068=CARTESIAN_POINT('Ctrl Pts',(-0.234207775344483,0.00269784071003669,
-0.00968932931015458));
#30069=CARTESIAN_POINT('Ctrl Pts',(-0.224905188461513,0.000775386387695849,
-0.00774097724716007));
#30070=CARTESIAN_POINT('Ctrl Pts',(-0.228005812987761,0.000760338332521188,
-0.0077754138708565));
#30071=CARTESIAN_POINT('Ctrl Pts',(-0.231106437467874,0.000745278047377309,
-0.00780984908461508));
#30072=CARTESIAN_POINT('Ctrl Pts',(-0.234207061909447,0.000730205873823641,
-0.00784428237662763));
#30073=CARTESIAN_POINT('Ctrl Pts',(-0.224904545212544,-0.00037433699893992,
-0.00611286595312136));
#30074=CARTESIAN_POINT('Ctrl Pts',(-0.228005169500613,-0.000380655003703386,
-0.00613103039787742));
#30075=CARTESIAN_POINT('Ctrl Pts',(-0.231105793767721,-0.000386989095479687,
-0.00614919200572512));
#30076=CARTESIAN_POINT('Ctrl Pts',(-0.234206418022201,-0.000393338834079428,
-0.00616734988680402));
#30077=CARTESIAN_POINT('Ctrl Pts',(-0.224903937950997,-0.00100476933014151,
-0.00458381173225385));
#30078=CARTESIAN_POINT('Ctrl Pts',(-0.228004563842973,-0.000997949740617374,
-0.00458943898701532));
#30079=CARTESIAN_POINT('Ctrl Pts',(-0.231105189790958,-0.000991151361328939,
-0.00459505880592969));
#30080=CARTESIAN_POINT('Ctrl Pts',(-0.234205815794275,-0.000984373265027772,
-0.00460066961067425));
#30081=CARTESIAN_POINT('Ctrl Pts',(-0.224903434943426,-0.00130314167877163,
-0.00330350941820122));
#30082=CARTESIAN_POINT('Ctrl Pts',(-0.228004062879574,-0.00128286930948369,
-0.00330122419140405));
#30083=CARTESIAN_POINT('Ctrl Pts',(-0.231104690943801,-0.00126261869681616,
-0.0032989320974583));
#30084=CARTESIAN_POINT('Ctrl Pts',(-0.234205319131308,-0.00124238896138437,
-0.00329663139924215));
#30085=CARTESIAN_POINT('Ctrl Pts',(-0.224903041260456,-0.00140805611840559,
-0.00232453718253355));
#30086=CARTESIAN_POINT('Ctrl Pts',(-0.228003673257076,-0.0013756315595115,
-0.00231672000225054));
#30087=CARTESIAN_POINT('Ctrl Pts',(-0.231104305522642,-0.00134323774830377,
-0.00230888218475535));
#30088=CARTESIAN_POINT('Ctrl Pts',(-0.234204938019884,-0.00131087220379368,
-0.00230102069899992));
#30089=CARTESIAN_POINT('Ctrl Pts',(-0.224902686634356,-0.00144960594189391,
-0.00134999602285112));
#30090=CARTESIAN_POINT('Ctrl Pts',(-0.228003316903184,-0.00140612182039602,
-0.00134119316178982));
#30091=CARTESIAN_POINT('Ctrl Pts',(-0.23110394734855,-0.00136264456921374,
-0.00133240814074275));
#30092=CARTESIAN_POINT('Ctrl Pts',(-0.234204577993143,-0.00131917594314456,
-0.00132364092587474));
#30093=CARTESIAN_POINT('Ctrl Pts',(-0.22490247733939,-0.0014891827680679,
-8.48946648711828E-5));
#30094=CARTESIAN_POINT('Ctrl Pts',(-0.228003104745152,-0.00143870380997731,
-8.36968663193096E-5));
#30095=CARTESIAN_POINT('Ctrl Pts',(-0.231103732057244,-0.00138822193789455,
-8.25021078797203E-5));
#30096=CARTESIAN_POINT('Ctrl Pts',(-0.23420435926242,-0.00133773601187166,
-8.1311084157012E-5));
#30097=CARTESIAN_POINT('Ctrl Pts',(-0.22490260183294,-0.0014577307002292,
0.00116946334942344));
#30098=CARTESIAN_POINT('Ctrl Pts',(-0.228003232282475,-0.00141157334093523,
0.00115947282708936));
#30099=CARTESIAN_POINT('Ctrl Pts',(-0.231103862912961,-0.00136541961535455,
0.00114950766822477));
#30100=CARTESIAN_POINT('Ctrl Pts',(-0.234204493755065,-0.001319272064998,
0.00113956823678177));
#30101=CARTESIAN_POINT('Ctrl Pts',(-0.224903104718753,-0.00140104996632292,
0.00247428939345485));
#30102=CARTESIAN_POINT('Ctrl Pts',(-0.228003735975788,-0.00137069112187628,
0.00246735401736931));
#30103=CARTESIAN_POINT('Ctrl Pts',(-0.231104367476161,-0.0013403616690761,
0.00246039968961847));
#30104=CARTESIAN_POINT('Ctrl Pts',(-0.234204999187845,-0.00131005933689176,
0.00245342357850486));
#30105=CARTESIAN_POINT('Ctrl Pts',(-0.224903620487317,-0.00123313642614889,
0.00377581720335721));
#30106=CARTESIAN_POINT('Ctrl Pts',(-0.228004247058324,-0.00121832689931329,
0.00377611259775251));
#30107=CARTESIAN_POINT('Ctrl Pts',(-0.231104873711069,-0.00120353701330459,
0.00377640441621043));
#30108=CARTESIAN_POINT('Ctrl Pts',(-0.234205500449294,-0.00118876627184354,
0.00377669124621538));
#30109=CARTESIAN_POINT('Ctrl Pts',(-0.224904244452509,-0.000745411287960432,
0.00535508951527424));
#30110=CARTESIAN_POINT('Ctrl Pts',(-0.228004869369835,-0.000745883603517816,
0.00536654310520161));
#30111=CARTESIAN_POINT('Ctrl Pts',(-0.231105494301186,-0.000746375225293753,
0.00537799072107391));
#30112=CARTESIAN_POINT('Ctrl Pts',(-0.234206119249757,-0.000746885383007411,
0.00538943105918803));
#30113=CARTESIAN_POINT('Ctrl Pts',(-0.224904927022406,0.000243903830950042,
0.00708094602779947));
#30114=CARTESIAN_POINT('Ctrl Pts',(-0.22800555124417,0.000231747907332828,
0.00710847531073915));
#30115=CARTESIAN_POINT('Ctrl Pts',(-0.231106175424446,0.00021957829815924,
0.00713600296412369));
#30116=CARTESIAN_POINT('Ctrl Pts',(-0.234206799572117,0.000207395346249357,
0.0071635283576419));
#30117=CARTESIAN_POINT('Ctrl Pts',(-0.224905705882564,0.00204129536417242,
0.00904270545084878));
#30118=CARTESIAN_POINT('Ctrl Pts',(-0.228006331417495,0.00202251745037019,
0.00909153197079319));
#30119=CARTESIAN_POINT('Ctrl Pts',(-0.231106956906316,0.00200373108991613,
0.00914035807264341));
#30120=CARTESIAN_POINT('Ctrl Pts',(-0.234207582354303,0.00198493654309014,
0.00918918354252649));
#30121=CARTESIAN_POINT('Ctrl Pts',(-0.224906344934492,0.00503279669879239,
0.0106558220281949));
#30122=CARTESIAN_POINT('Ctrl Pts',(-0.228006973230644,0.00502108315461209,
0.0107253467403358));
#30123=CARTESIAN_POINT('Ctrl Pts',(-0.231107601524016,0.00500936667421796,
0.0107948715627757));
#30124=CARTESIAN_POINT('Ctrl Pts',(-0.234208229814862,0.00499764738343722,
0.0108643965065502));
#30125=CARTESIAN_POINT('Ctrl Pts',(-0.22490642148267,0.00911553811978304,
0.0108495997280891));
#30126=CARTESIAN_POINT('Ctrl Pts',(-0.22800705020616,0.00912342211753167,
0.0109217712057851));
#30127=CARTESIAN_POINT('Ctrl Pts',(-0.231107678935135,0.0091313080421625,
0.0109939426427322));
#30128=CARTESIAN_POINT('Ctrl Pts',(-0.234208307668951,0.00913919580236395,
0.0110661140483708));
#30129=CARTESIAN_POINT('Ctrl Pts',(-0.224905896781363,0.0122479140000228,
0.00952499840433065));
#30130=CARTESIAN_POINT('Ctrl Pts',(-0.228006522998932,0.0122659797356893,
0.00957977773742142));
#30131=CARTESIAN_POINT('Ctrl Pts',(-0.231107149178945,0.012284052220171,
0.00963455709198015));
#30132=CARTESIAN_POINT('Ctrl Pts',(-0.234207775325653,0.0123021312474762,
0.00968933635838273));
#30133=CARTESIAN_POINT('Ctrl Pts',(-0.224905188406661,0.0142245802852993,
0.00774097735435126));
#30134=CARTESIAN_POINT('Ctrl Pts',(-0.228005812932864,0.014239626038719,
0.0077754139801973));
#30135=CARTESIAN_POINT('Ctrl Pts',(-0.231106437412959,0.0142546840218181,
0.00780984919513146));
#30136=CARTESIAN_POINT('Ctrl Pts',(-0.234207061854539,0.014269753892948,
0.00784428248742507));
#30137=CARTESIAN_POINT('Ctrl Pts',(-0.224904545213284,0.0153743354777482,
0.00611286639462737));
#30138=CARTESIAN_POINT('Ctrl Pts',(-0.228005169501712,0.0153806533667306,
0.00613103086359291));
#30139=CARTESIAN_POINT('Ctrl Pts',(-0.231105793769188,0.0153869873403304,
0.0061491924949429));
#30140=CARTESIAN_POINT('Ctrl Pts',(-0.234206418024041,0.0153933369583363,
0.00616735039916125));
#30141=CARTESIAN_POINT('Ctrl Pts',(-0.224903937959543,0.0160047733300576,
0.00458381273421664));
#30142=CARTESIAN_POINT('Ctrl Pts',(-0.228004563851456,0.015997954017428,
0.00458944005855562));
#30143=CARTESIAN_POINT('Ctrl Pts',(-0.231105189799372,0.0159911559151915,
0.00459505994710943));
#30144=CARTESIAN_POINT('Ctrl Pts',(-0.234205815802617,0.0159843780961064,
0.00460067082154373));
#30145=CARTESIAN_POINT('Ctrl Pts',(-0.224903434945887,0.0163031426775171,
0.00330350985910996));
#30146=CARTESIAN_POINT('Ctrl Pts',(-0.228004062882068,0.0162828703806443,
0.0033012246620879));
#30147=CARTESIAN_POINT('Ctrl Pts',(-0.231104690946332,0.0162626198410551,
0.00329893259759974));
#30148=CARTESIAN_POINT('Ctrl Pts',(-0.23420531913388,0.0162423901793082,
0.00329663192843727));
#30149=CARTESIAN_POINT('Ctrl Pts',(-0.224903172488496,0.0163730847941923,
0.00265086132944247));
#30150=CARTESIAN_POINT('Ctrl Pts',(-0.22800380313163,0.0163447109764496,
0.00264488813827189));
#30151=CARTESIAN_POINT('Ctrl Pts',(-0.231104433996755,0.0163163649094739,
0.00263889889986091));
#30152=CARTESIAN_POINT('Ctrl Pts',(-0.234205065057425,0.0162880446461359,
0.00263289101445681));
#30153=CARTESIAN_POINT('Ctrl Pts',(-0.224903047769934,0.0163974953490442,
0.00232527569536224));
#30154=CARTESIAN_POINT('Ctrl Pts',(-0.228003678801843,0.0163652528946496,
0.00231821622721085));
#30155=CARTESIAN_POINT('Ctrl Pts',(-0.23110431006382,0.0163330357098684,
0.00231114482972889));
#30156=CARTESIAN_POINT('Ctrl Pts',(-0.234204941533998,0.0163008422866106,
0.00230405918705812));
#30157=CARTESIAN_POINT('',(-0.225009761049809,0.0164742955512205,-2.91283822632387E-7));
#30158=CARTESIAN_POINT('Ctrl Pts',(-0.225009761049848,0.0164742955512199,
-2.9128306942331E-7));
#30159=CARTESIAN_POINT('Ctrl Pts',(-0.225235788735119,0.0164707797999031,
0.000697174222861705));
#30160=CARTESIAN_POINT('Ctrl Pts',(-0.225493369618686,0.016441583044206,
0.00148467486114592));
#30161=CARTESIAN_POINT('Ctrl Pts',(-0.225831296494198,0.0163919000464353,
0.00223757402366504));
#30162=CARTESIAN_POINT('Ctrl Pts',(-0.225870784240265,0.0163857105469993,
0.00232295787970897));
#30163=CARTESIAN_POINT('Ctrl Pts',(-0.231901468479132,0.0119424667401788,
-0.00964990277379923));
#30164=CARTESIAN_POINT('Ctrl Pts',(-0.23196556433204,0.0120553195071661,
-0.00958547241096005));
#30165=CARTESIAN_POINT('Ctrl Pts',(-0.232092641041587,0.012318056643556,
-0.00942714628191483));
#30166=CARTESIAN_POINT('Ctrl Pts',(-0.232189484894588,0.0127464465580913,
-0.00913453448129261));
#30167=CARTESIAN_POINT('Ctrl Pts',(-0.232026909656826,0.0133298270418654,
-0.00866985986404063));
#30168=CARTESIAN_POINT('Ctrl Pts',(-0.231431264476163,0.0138642223513919,
-0.00814845542092376));
#30169=CARTESIAN_POINT('Ctrl Pts',(-0.230626882102772,0.0143537410803797,
-0.00758117056316697));
#30170=CARTESIAN_POINT('Ctrl Pts',(-0.229503933937131,0.0149270508431769,
-0.00680405147634905));
#30171=CARTESIAN_POINT('Ctrl Pts',(-0.22817297623813,0.0155747191869899,
-0.00568892386192561));
#30172=CARTESIAN_POINT('Ctrl Pts',(-0.227021852380984,0.0160747388453188,
-0.00431844004910359));
#30173=CARTESIAN_POINT('Ctrl Pts',(-0.22625946762174,0.0163293197705724,
-0.00307502577355553));
#30174=CARTESIAN_POINT('Ctrl Pts',(-0.225588510819443,0.0164318308607234,
-0.00175821008748369));
#30175=CARTESIAN_POINT('Ctrl Pts',(-0.225239759337853,0.0164707047194801,
-0.000703191917106053));
#30176=CARTESIAN_POINT('Ctrl Pts',(-0.225009761049809,0.0164742955512205,
-2.91283822632387E-7));
#30177=CARTESIAN_POINT('',(-0.227105547431055,0.0164416356533412,-1.96367613579375E-8));
#30178=CARTESIAN_POINT('Ctrl Pts',(-0.227105547430907,0.0164416356533435,
-1.96363604482556E-8));
#30179=CARTESIAN_POINT('Ctrl Pts',(-0.227140935573775,0.0164410841784684,
-9.60298985735003E-5));
#30180=CARTESIAN_POINT('Ctrl Pts',(-0.227176314604842,0.0164400697376915,
-0.000192131486811683));
#30181=CARTESIAN_POINT('Ctrl Pts',(-0.227212010478261,0.0164386687878891,
-0.000288124301984629));
#30182=CARTESIAN_POINT('Ctrl Pts',(-0.227307348630138,0.016434927067846,
-0.000544506250803369));
#30183=CARTESIAN_POINT('Ctrl Pts',(-0.227404969846049,0.0164285564552437,
-0.00080011931205441));
#30184=CARTESIAN_POINT('Ctrl Pts',(-0.227510944626544,0.0164208305077663,
-0.00105112973174067));
#30185=CARTESIAN_POINT('Ctrl Pts',(-0.227524004952427,0.0164198783624414,
-0.00108206424149788));
#30186=CARTESIAN_POINT('Ctrl Pts',(-0.227537191850656,0.0164189056258689,
-0.00111292900197045));
#30187=CARTESIAN_POINT('Ctrl Pts',(-0.227550505575517,0.0164179103665598,
-0.00114372242291194));
#30188=CARTESIAN_POINT('Ctrl Pts',(-0.227570729683619,0.0164163985258039,
-0.00119049892463991));
#30189=CARTESIAN_POINT('Ctrl Pts',(-0.227591245817737,0.0164148331361413,
-0.00123710938263162));
#30190=CARTESIAN_POINT('Ctrl Pts',(-0.227612055857281,0.0164132070087615,
-0.00128355085207765));
#30191=CARTESIAN_POINT('Ctrl Pts',(-0.227684890995684,0.0164075155629321,
-0.00144609599513877));
#30192=CARTESIAN_POINT('Ctrl Pts',(-0.227761330033667,0.0164011975804018,
-0.00160657657145748));
#30193=CARTESIAN_POINT('Ctrl Pts',(-0.227841439738122,0.016393908424669,
-0.00176485026197984));
#30194=CARTESIAN_POINT('Ctrl Pts',(-0.22788149459035,0.0163902638468026,
-0.00184398710724102));
#30195=CARTESIAN_POINT('Ctrl Pts',(-0.227922466302893,0.0163863523316187,
-0.00192257103644991));
#30196=CARTESIAN_POINT('Ctrl Pts',(-0.227964360185775,0.0163821164167468,
-0.0020005813551573));
#30197=CARTESIAN_POINT('Ctrl Pts',(-0.227994642668365,0.0163790545373139,
-0.00205697016315432));
#30198=CARTESIAN_POINT('Ctrl Pts',(-0.228025406156946,0.0163758205550357,
-0.00211305781216197));
#30199=CARTESIAN_POINT('Ctrl Pts',(-0.228056654057935,0.0163723992572222,
-0.00216883939895636));
#30200=CARTESIAN_POINT('Ctrl Pts',(-0.228068635634597,0.0163710874077623,
-0.0021902280790714));
#30201=CARTESIAN_POINT('Ctrl Pts',(-0.228080688431295,0.0163697480197511,
-0.00221157175871921));
#30202=CARTESIAN_POINT('Ctrl Pts',(-0.228092811031844,0.0163683783499799,
-0.00223286967464982));
#30203=CARTESIAN_POINT('Ctrl Pts',(-0.228286284646469,0.0163465187695721,
-0.00257277898389818));
#30204=CARTESIAN_POINT('Ctrl Pts',(-0.228497453761435,0.016317224118046,
-0.00290123520754679));
#30205=CARTESIAN_POINT('Ctrl Pts',(-0.228724359620867,0.0162698007708276,
-0.00321950024123378));
#30206=CARTESIAN_POINT('Ctrl Pts',(-0.228731950990746,0.0162682141737667,
-0.00323014812664534));
#30207=CARTESIAN_POINT('Ctrl Pts',(-0.228739560119947,0.0162666070912213,
-0.00324078450904247));
#30208=CARTESIAN_POINT('Ctrl Pts',(-0.228747187150802,0.0162649798437748,
-0.00325140938042041));
#30209=CARTESIAN_POINT('Ctrl Pts',(-0.22886498654879,0.0162398470269272,
-0.00341551038850264));
#30210=CARTESIAN_POINT('Ctrl Pts',(-0.228987064650102,0.0162097845462495,
-0.003576845525633));
#30211=CARTESIAN_POINT('Ctrl Pts',(-0.229113100652467,0.0161761306248802,
-0.00373426103364333));
#30212=CARTESIAN_POINT('Ctrl Pts',(-0.229235349109519,0.0161434880474898,
-0.00388694600150465));
#30213=CARTESIAN_POINT('Ctrl Pts',(-0.229361320812065,0.0161074674237774,
-0.00403594274649993));
#30214=CARTESIAN_POINT('Ctrl Pts',(-0.229490644364937,0.0160692846524978,
-0.00418024936974081));
#30215=CARTESIAN_POINT('Ctrl Pts',(-0.229494651113392,0.0160681016602552,
-0.00418472032902758));
#30216=CARTESIAN_POINT('Ctrl Pts',(-0.229498661073176,0.0160669165977826,
-0.00418918679279889));
#30217=CARTESIAN_POINT('Ctrl Pts',(-0.229502674213524,0.0160657294663742,
-0.00419364877005753));
#30218=CARTESIAN_POINT('Ctrl Pts',(-0.229769760214949,0.0159867224659753,
-0.00449060615537639));
#30219=CARTESIAN_POINT('Ctrl Pts',(-0.230050851774607,0.0158986361087921,
-0.00476766623051437));
#30220=CARTESIAN_POINT('Ctrl Pts',(-0.230340579947594,0.0158014507554148,
-0.00503153449351247));
#30221=CARTESIAN_POINT('Ctrl Pts',(-0.230485444034087,0.0157528580787261,
-0.00516346862501151));
#30222=CARTESIAN_POINT('Ctrl Pts',(-0.23063247142736,0.015701991599058,
-0.005292100425029));
#30223=CARTESIAN_POINT('Ctrl Pts',(-0.230781004357612,0.0156488559127553,
-0.00541825073710578));
#30224=CARTESIAN_POINT('Ctrl Pts',(-0.230929537287864,0.0155957202264526,
-0.00554440104918256));
#30225=CARTESIAN_POINT('Ctrl Pts',(-0.231079576062874,0.0155403155041193,
-0.00566806935446317));
#30226=CARTESIAN_POINT('Ctrl Pts',(-0.231230463152709,0.0154826501973941,
-0.00579007476384777));
#30227=CARTESIAN_POINT('Ctrl Pts',(-0.23123663742441,0.0154802905437494,
-0.00579506720254754));
#30228=CARTESIAN_POINT('Ctrl Pts',(-0.231242813084713,0.015477927087919,
-0.00580005681784355));
#30229=CARTESIAN_POINT('Ctrl Pts',(-0.231248990111509,0.0154755598168904,
-0.00580504368212982));
#30230=CARTESIAN_POINT('Ctrl Pts',(-0.231393767503663,0.0154200756272723,
-0.00592192599949613));
#30231=CARTESIAN_POINT('Ctrl Pts',(-0.231539296831414,0.0153624991268241,
-0.00603729915711179));
#30232=CARTESIAN_POINT('Ctrl Pts',(-0.231684621095551,0.0153023668196266,
-0.00615185576425954));
#30233=CARTESIAN_POINT('Ctrl Pts',(-0.231836145719153,0.0152396689262739,
-0.00627130000767094));
#30234=CARTESIAN_POINT('Ctrl Pts',(-0.231987452488494,0.0151741955395839,
-0.00638985441608159));
#30235=CARTESIAN_POINT('Ctrl Pts',(-0.232137421202335,0.0151053986626134,
-0.0065083426471185));
#30236=CARTESIAN_POINT('Ctrl Pts',(-0.232147808330346,0.0151006336556357,
-0.00651654937498939));
#30237=CARTESIAN_POINT('Ctrl Pts',(-0.232158189240001,0.0150958524418954,
-0.00652475591244986));
#30238=CARTESIAN_POINT('Ctrl Pts',(-0.232168563225385,0.0150910549860577,
-0.0065329622985253));
#30239=CARTESIAN_POINT('Ctrl Pts',(-0.232307968201396,0.0150265870702838,
-0.00664323920866527));
#30240=CARTESIAN_POINT('Ctrl Pts',(-0.232446123690228,0.0149591860652729,
-0.00675348212769047));
#30241=CARTESIAN_POINT('Ctrl Pts',(-0.232580949251388,0.0148875018376449,
-0.00686495643825133));
#30242=CARTESIAN_POINT('Ctrl Pts',(-0.232725808015384,0.0148104831438382,
-0.00698472624084943));
#30243=CARTESIAN_POINT('Ctrl Pts',(-0.232866806881461,0.0147285158365232,
-0.00710592568938485));
#30244=CARTESIAN_POINT('Ctrl Pts',(-0.233001397075398,0.0146399654688394,
-0.00723005776422935));
#30245=CARTESIAN_POINT('Ctrl Pts',(-0.23301078614597,0.0146337881566073,
-0.00723871727185641));
#30246=CARTESIAN_POINT('Ctrl Pts',(-0.233020143486601,0.0146275789986391,
-0.00724739024669289));
#30247=CARTESIAN_POINT('Ctrl Pts',(-0.233029468522886,0.0146213373298964,
-0.0072560774060185));
#30248=CARTESIAN_POINT('Ctrl Pts',(-0.23315381576358,0.0145381060949952,
-0.00737191870235509));
#30249=CARTESIAN_POINT('Ctrl Pts',(-0.23327241953563,0.0144490980254842,
-0.00749027865120103));
#30250=CARTESIAN_POINT('Ctrl Pts',(-0.233382525334888,0.0143533124344016,
-0.00761063469097697));
#30251=CARTESIAN_POINT('Ctrl Pts',(-0.233500888177628,0.0142503436995081,
-0.00774001645928322));
#30252=CARTESIAN_POINT('Ctrl Pts',(-0.233609449565788,0.0141395435376383,
-0.00787171593683602));
#30253=CARTESIAN_POINT('Ctrl Pts',(-0.233704718238572,0.0140195979133241,
-0.00800520776939137));
#30254=CARTESIAN_POINT('Ctrl Pts',(-0.233711754187254,0.0140107394792492,
-0.00801506664173452));
#30255=CARTESIAN_POINT('Ctrl Pts',(-0.23371871727556,0.0140018315631178,
-0.00802493503816399));
#30256=CARTESIAN_POINT('Ctrl Pts',(-0.233725606005006,0.0139928736528168,
-0.00803481260910125));
#30257=CARTESIAN_POINT('Ctrl Pts',(-0.233765354917564,0.0139411852832834,
-0.00809180754648525));
#30258=CARTESIAN_POINT('Ctrl Pts',(-0.233802628113303,0.0138878323304247,
-0.00814910802237563));
#30259=CARTESIAN_POINT('Ctrl Pts',(-0.233837278186415,0.0138329085468894,
-0.00820649113639346));
#30260=CARTESIAN_POINT('Ctrl Pts',(-0.233898260900202,0.0137362449306085,
-0.0083074830739002));
#30261=CARTESIAN_POINT('Ctrl Pts',(-0.233951125609911,0.0136347095732914,
-0.00840873442372893));
#30262=CARTESIAN_POINT('Ctrl Pts',(-0.233995079511644,0.0135287531593584,
-0.00850908837254629));
#30263=CARTESIAN_POINT('Ctrl Pts',(-0.234039033413378,0.0134227967454253,
-0.00860944232136365));
#30264=CARTESIAN_POINT('Ctrl Pts',(-0.234074079450773,0.0133124189875615,
-0.00870890006003178));
#30265=CARTESIAN_POINT('Ctrl Pts',(-0.234099371837349,0.0131980565381413,
-0.00880635042806751));
#30266=CARTESIAN_POINT('Ctrl Pts',(-0.234101929684424,0.0131864909369363,
-0.00881620569174632));
#30267=CARTESIAN_POINT('Ctrl Pts',(-0.234104387698283,0.0131748847922406,
-0.00882604066222298));
#30268=CARTESIAN_POINT('Ctrl Pts',(-0.234106744905702,0.0131632387859299,
-0.00883585391535451));
#30269=CARTESIAN_POINT('Ctrl Pts',(-0.234135465605892,0.0130213414488917,
-0.00895542061057182));
#30270=CARTESIAN_POINT('Ctrl Pts',(-0.234149200249736,0.0128735165504675,
-0.00907176004245325));
#30271=CARTESIAN_POINT('Ctrl Pts',(-0.234148122016187,0.0127221513249176,
-0.00918311339548255));
#30272=CARTESIAN_POINT('Ctrl Pts',(-0.234147538652231,0.012640257177773,
-0.0092433596498313));
#30273=CARTESIAN_POINT('Ctrl Pts',(-0.234142623795018,0.0125573369859019,
-0.00930216102216956));
#30274=CARTESIAN_POINT('Ctrl Pts',(-0.2341334317926,0.0124737587188891,
-0.00935924909880171));
#30275=CARTESIAN_POINT('Ctrl Pts',(-0.234128835791391,0.0124319695853827,
-0.00938779313711778));
#30276=CARTESIAN_POINT('Ctrl Pts',(-0.234123170785509,0.0123900143644245,
-0.00941590693239571));
#30277=CARTESIAN_POINT('Ctrl Pts',(-0.23411644470908,0.0123479377552723,
-0.00944355743439764));
#30278=CARTESIAN_POINT('Ctrl Pts',(-0.234109718632652,0.0123058611461201,
-0.00947120793639956));
#30279=CARTESIAN_POINT('Ctrl Pts',(-0.234101931503068,0.01226366317307,
-0.00949839513366344));
#30280=CARTESIAN_POINT('Ctrl Pts',(-0.234093091644146,0.0122213891644512,
-0.00952508926526118));
#30281=CARTESIAN_POINT('Ctrl Pts',(-0.234090670032958,0.0122098085257659,
-0.00953240191677332));
#30282=CARTESIAN_POINT('Ctrl Pts',(-0.234088169321776,0.0121982220309786,
-0.00953967830460782));
#30283=CARTESIAN_POINT('Ctrl Pts',(-0.234085589675658,0.0121866306191717,
-0.00954691779081663));
#30284=CARTESIAN_POINT('Ctrl Pts',(-0.2340682957397,0.0121089218466376,
-0.00959545127374656));
#30285=CARTESIAN_POINT('Ctrl Pts',(-0.234047453702354,0.0120309920728459,
-0.00964232599577092));
#30286=CARTESIAN_POINT('Ctrl Pts',(-0.234023415843097,0.0119530144195835,
-0.00968754222491458));
#30287=CARTESIAN_POINT('Ctrl Pts',(-0.228104649974285,0.0163642118483275,
0.00231798200374011));
#30288=CARTESIAN_POINT('Ctrl Pts',(-0.228080473933464,0.0163672125078731,
0.00227403526561382));
#30289=CARTESIAN_POINT('Ctrl Pts',(-0.228056571982133,0.0163700464923153,
0.00222992337348044));
#30290=CARTESIAN_POINT('Ctrl Pts',(-0.228032949149827,0.0163727324397856,
0.00218564039839086));
#30291=CARTESIAN_POINT('Ctrl Pts',(-0.227887225499328,0.0163893014127747,
0.00191246922648189));
#30292=CARTESIAN_POINT('Ctrl Pts',(-0.227752115936573,0.0164000989794123,
0.00163267292450821));
#30293=CARTESIAN_POINT('Ctrl Pts',(-0.22762725738731,0.0164102722574105,
0.001347528898789));
#30294=CARTESIAN_POINT('Ctrl Pts',(-0.227593613235951,0.0164130135298889,
0.0012706945224726));
#30295=CARTESIAN_POINT('Ctrl Pts',(-0.227560713431936,0.0164157214331456,
0.00119347836067573));
#30296=CARTESIAN_POINT('Ctrl Pts',(-0.227528550504412,0.0164183289449134,
0.00111580340593609));
#30297=CARTESIAN_POINT('Ctrl Pts',(-0.227430952435461,0.0164262414122448,
0.000880099563898515));
#30298=CARTESIAN_POINT('Ctrl Pts',(-0.227340124895196,0.0164332189050637,
0.000640707665641815));
#30299=CARTESIAN_POINT('Ctrl Pts',(-0.227251433179574,0.0164371685419467,
0.000399944878391123));
#30300=CARTESIAN_POINT('Ctrl Pts',(-0.227202427891157,0.0164393508550662,
0.000266914980992263));
#30301=CARTESIAN_POINT('Ctrl Pts',(-0.227154074607713,0.016440605869286,
0.000133457190854296));
#30302=CARTESIAN_POINT('Ctrl Pts',(-0.227105591678119,0.0164410560897492,
1.32243616293715E-9));
#30303=CARTESIAN_POINT('Origin',(-0.226994617004166,0.00749997243979571,
0.00184285919272757));
#30304=CARTESIAN_POINT('',(-0.228031328918381,0.00748423226422772,0.010860760471908));
#30305=CARTESIAN_POINT('',(-0.225968509292903,0.0102911505109728,0.0103703808319117));
#30306=CARTESIAN_POINT('Ctrl Pts',(-0.225969748832453,0.0102900711236161,
0.0103707889115062));
#30307=CARTESIAN_POINT('Ctrl Pts',(-0.226289106570716,0.00978576005587371,
0.0105425714270296));
#30308=CARTESIAN_POINT('Ctrl Pts',(-0.22664061138589,0.00927176167283401,
0.0106681425457542));
#30309=CARTESIAN_POINT('Ctrl Pts',(-0.227339846850015,0.00833009565011997,
0.0108177785145977));
#30310=CARTESIAN_POINT('Ctrl Pts',(-0.227681836252118,0.00789982596134801,
0.0108536050057603));
#30311=CARTESIAN_POINT('Ctrl Pts',(-0.228033703347829,0.00748625084485732,
0.0108608393494597));
#30312=CARTESIAN_POINT('',(-0.225967560871587,0.00467023837789646,0.0103577170409566));
#30313=CARTESIAN_POINT('Ctrl Pts',(-0.228031308457579,0.00748420429971502,
0.0108607824347881));
#30314=CARTESIAN_POINT('Ctrl Pts',(-0.227821724450862,0.00723381073129729,
0.0108556558941106));
#30315=CARTESIAN_POINT('Ctrl Pts',(-0.227529404666869,0.00687470775376698,
0.0108331524160897));
#30316=CARTESIAN_POINT('Ctrl Pts',(-0.227175687258202,0.00641955626299225,
0.0107783812752486));
#30317=CARTESIAN_POINT('Ctrl Pts',(-0.226944206963435,0.00611293830577671,
0.010731009622336));
#30318=CARTESIAN_POINT('Ctrl Pts',(-0.226726702915377,0.00581110890073526,
0.0106729151048354));
#30319=CARTESIAN_POINT('Ctrl Pts',(-0.226565930211992,0.00557919413302389,
0.0106212588865583));
#30320=CARTESIAN_POINT('Ctrl Pts',(-0.226426475018125,0.00537259079248901,
0.0105700841876947));
#30321=CARTESIAN_POINT('Ctrl Pts',(-0.226359986159531,0.00527168795372337,
0.0105432010021426));
#30322=CARTESIAN_POINT('Ctrl Pts',(-0.226210309700029,0.00504332716767546,
0.0104795938046293));
#30323=CARTESIAN_POINT('Ctrl Pts',(-0.226074000007555,0.00483347349684773,
0.0104142248999611));
#30324=CARTESIAN_POINT('Ctrl Pts',(-0.225967561113698,0.00467023900632648,
0.0103577181008014));
#30325=CARTESIAN_POINT('',(-0.226088437963177,0.00749380654222876,0.0108173476998421));
#30326=CARTESIAN_POINT('Ctrl Pts',(-0.225965888685649,0.00467021151082653,
0.010357671607895));
#30327=CARTESIAN_POINT('Ctrl Pts',(-0.225942476168076,0.00559702753572744,
0.010664481305269));
#30328=CARTESIAN_POINT('Ctrl Pts',(-0.225998103434488,0.00657292145943362,
0.0108147034606632));
#30329=CARTESIAN_POINT('Ctrl Pts',(-0.226088521671434,0.00749380377234182,
0.0108173545262585));
#30330=CARTESIAN_POINT('Ctrl Pts',(-0.226088395525365,0.00749423713891311,
0.0108173519914327));
#30331=CARTESIAN_POINT('Ctrl Pts',(-0.226088209593573,0.00749614094361597,
0.010817349043451));
#30332=CARTESIAN_POINT('Ctrl Pts',(-0.226088023861152,0.0074980445644577,
0.0108173454950728));
#30333=CARTESIAN_POINT('Ctrl Pts',(-0.225999185723901,0.00840946053812611,
0.0108153591200668));
#30334=CARTESIAN_POINT('Ctrl Pts',(-0.225945309305692,0.00937289305355034,
0.0106696121468602));
#30335=CARTESIAN_POINT('Ctrl Pts',(-0.225967999251384,0.010289620296038,
0.0103708969367641));
#30336=CARTESIAN_POINT('Ctrl Pts',(-0.185723055456903,0.0169037490465727,
0.00243669718465323));
#30337=CARTESIAN_POINT('Ctrl Pts',(-0.232326704333039,0.0164203047763951,
0.00231142721965166));
#30338=CARTESIAN_POINT('Ctrl Pts',(-0.185723055456903,0.0169917319681535,
0.0020581868105832));
#30339=CARTESIAN_POINT('Ctrl Pts',(-0.232326704333039,0.0164327431878904,
0.00190716238014556));
#30340=CARTESIAN_POINT('Ctrl Pts',(-0.185723055456904,0.0171348389058692,
0.00126455176521327));
#30341=CARTESIAN_POINT('Ctrl Pts',(-0.232326704333039,0.0164529746481233,
0.00113116956517427));
#30342=CARTESIAN_POINT('Ctrl Pts',(-0.185723055456903,0.0172123852537007,
-4.57104323127425E-14));
#30343=CARTESIAN_POINT('Ctrl Pts',(-0.232326704333039,0.0164639376096499,
-5.12643732643055E-15));
#30344=CARTESIAN_POINT('Ctrl Pts',(-0.185723055456904,0.0171348389058572,
-0.00126455176530287));
#30345=CARTESIAN_POINT('Ctrl Pts',(-0.232326704333039,0.0164529746481216,
-0.00113116956518479));
#30346=CARTESIAN_POINT('Ctrl Pts',(-0.185723055456903,0.0169917319681347,
-0.00205818681066974));
#30347=CARTESIAN_POINT('Ctrl Pts',(-0.232326704333039,0.0164327431878878,
-0.00190716238015681));
#30348=CARTESIAN_POINT('Ctrl Pts',(-0.185723055456903,0.0166573800151943,
-0.00349659872622789));
#30349=CARTESIAN_POINT('Ctrl Pts',(-0.232326704333039,0.0163854748419384,
-0.00344344619644609));
#30350=CARTESIAN_POINT('Ctrl Pts',(-0.185723055456904,0.0158049536659853,
-0.00552554202981291));
#30351=CARTESIAN_POINT('Ctrl Pts',(-0.23232670433304,0.0158790365063827,
-0.00570322401511438));
#30352=CARTESIAN_POINT('Ctrl Pts',(-0.185723055456903,0.0136025708308564,
-0.00796594412460981));
#30353=CARTESIAN_POINT('Ctrl Pts',(-0.232326704333039,0.0138912669883084,
-0.00858048214849728));
#30354=CARTESIAN_POINT('Ctrl Pts',(-0.185723055456904,0.0107282744647946,
-0.00954209114738551));
#30355=CARTESIAN_POINT('Ctrl Pts',(-0.23232670433304,0.0109544909042364,
-0.010506785011137));
#30356=CARTESIAN_POINT('Ctrl Pts',(-0.185723055456903,0.00749999999987153,
-0.0100866616277759));
#30357=CARTESIAN_POINT('Ctrl Pts',(-0.232326704333039,0.00749999999987138,
-0.0111842362468306));
#30358=CARTESIAN_POINT('Ctrl Pts',(-0.185723055456904,0.00427172553496278,
-0.00954209114730134));
#30359=CARTESIAN_POINT('Ctrl Pts',(-0.23232670433304,0.00404550909552549,
-0.0105067850110401));
#30360=CARTESIAN_POINT('Ctrl Pts',(-0.185723055456903,0.00139742916894219,
-0.0079659441244508));
#30361=CARTESIAN_POINT('Ctrl Pts',(-0.232326704333039,0.00110873301150744,
-0.00858048214831799));
#30362=CARTESIAN_POINT('Ctrl Pts',(-0.185723055456904,-0.000804953666122893,
-0.00552554202959671));
#30363=CARTESIAN_POINT('Ctrl Pts',(-0.23232670433304,-0.000879036506486045,
-0.00570322401487933));
#30364=CARTESIAN_POINT('Ctrl Pts',(-0.185723055456903,-0.00165738001527906,
-0.00349659872598971));
#30365=CARTESIAN_POINT('Ctrl Pts',(-0.232326704333039,-0.0013854748419783,
-0.00344344619619682));
#30366=CARTESIAN_POINT('Ctrl Pts',(-0.185723055456903,-0.00199173196817847,
-0.00205818681044279));
#30367=CARTESIAN_POINT('Ctrl Pts',(-0.232326704333039,-0.00143274318789395,
-0.00190716237992731));
#30368=CARTESIAN_POINT('Ctrl Pts',(-0.185723055456903,-0.00213483890587743,
-0.00126455176511326));
#30369=CARTESIAN_POINT('Ctrl Pts',(-0.232326704333039,-0.00145297464812447,
-0.001131169564997));
#30370=CARTESIAN_POINT('Ctrl Pts',(-0.185723055456904,-0.00221238525369828,
8.33588010327838E-14));
#30371=CARTESIAN_POINT('Ctrl Pts',(-0.232326704333039,-0.0014639376096495,
1.20148665217339E-13));
#30372=CARTESIAN_POINT('Ctrl Pts',(-0.185723055456903,-0.00213483890585875,
0.00126455176527974));
#30373=CARTESIAN_POINT('Ctrl Pts',(-0.232326704333039,-0.00145297464812182,
0.00113116956523674));
#30374=CARTESIAN_POINT('Ctrl Pts',(-0.185723055456903,-0.00199173196814768,
0.00205818681060856));
#30375=CARTESIAN_POINT('Ctrl Pts',(-0.232326704333039,-0.0014327431878896,
0.00190716238016579));
#30376=CARTESIAN_POINT('Ctrl Pts',(-0.185723055456903,-0.00165738001522438,
0.00349659872621544));
#30377=CARTESIAN_POINT('Ctrl Pts',(-0.232326704333039,-0.00138547484194287,
0.00344344619705013));
#30378=CARTESIAN_POINT('Ctrl Pts',(-0.185723055456904,-0.000804955358563482,
0.00552554230330677));
#30379=CARTESIAN_POINT('Ctrl Pts',(-0.232326704333039,-0.000879051981413446,
0.0057032265164018));
#30380=CARTESIAN_POINT('Ctrl Pts',(-0.185723055456903,0.00139743580946407,
0.00796594412565152));
#30381=CARTESIAN_POINT('Ctrl Pts',(-0.232326704333039,0.00110879372578601,
0.00858048215857438));
#30382=CARTESIAN_POINT('Ctrl Pts',(-0.185723055456904,0.00427172361958147,
0.0095420921652245));
#30383=CARTESIAN_POINT('Ctrl Pts',(-0.232326704333039,0.0040454915818506,
0.0105067943176977));
#30384=CARTESIAN_POINT('Ctrl Pts',(-0.185723055456904,0.00750000000000269,
0.0100866612741451));
#30385=CARTESIAN_POINT('Ctrl Pts',(-0.23232670433304,0.00749999999999982,
0.011184233013541));
#30386=CARTESIAN_POINT('Ctrl Pts',(-0.185723055456904,0.0107282763804236,
0.00954209216522276));
#30387=CARTESIAN_POINT('Ctrl Pts',(-0.232326704333039,0.010954508418149,
0.0105067943176979));
#30388=CARTESIAN_POINT('Ctrl Pts',(-0.185723055456904,0.0136025641905403,
0.00796594412564821));
#30389=CARTESIAN_POINT('Ctrl Pts',(-0.23232670433304,0.0138912062742137,
0.00858048215857484));
#30390=CARTESIAN_POINT('Ctrl Pts',(-0.185723055456904,0.0158049553585666,
0.0055255423033021));
#30391=CARTESIAN_POINT('Ctrl Pts',(-0.232326704333039,0.0158790519814133,
0.00570322651640249));
#30392=CARTESIAN_POINT('Ctrl Pts',(-0.185723055456903,0.0166573800152265,
0.00349659872621015));
#30393=CARTESIAN_POINT('Ctrl Pts',(-0.232326704333039,0.0163854748419429,
0.00344344619705094));
#30394=CARTESIAN_POINT('Ctrl Pts',(-0.185723055456903,0.0169037490465727,
0.00243669718465325));
#30395=CARTESIAN_POINT('Ctrl Pts',(-0.232326704333039,0.0164203047763951,
0.00231142721965168));
#30396=CARTESIAN_POINT('',(-0.214999728174719,0.0156143096410472,-0.00564621361629089));
#30397=CARTESIAN_POINT('Ctrl Pts',(-0.220090794747946,0.0165472343306677,
0.00234431717574848));
#30398=CARTESIAN_POINT('Ctrl Pts',(-0.220117505055273,0.0165517330921288,
0.00228542154256059));
#30399=CARTESIAN_POINT('Ctrl Pts',(-0.220143226024636,0.0165561317703932,
0.00222617711841132));
#30400=CARTESIAN_POINT('Ctrl Pts',(-0.220167930171668,0.0165604182112109,
0.00216658683604705));
#30401=CARTESIAN_POINT('Ctrl Pts',(-0.220302085046398,0.0165836955553021,
0.00184298420951398));
#30402=CARTESIAN_POINT('Ctrl Pts',(-0.220406320979476,0.0166037523754693,
0.00150806229365304));
#30403=CARTESIAN_POINT('Ctrl Pts',(-0.220478938005581,0.0166181019152006,
0.00116601824206587));
#30404=CARTESIAN_POINT('Ctrl Pts',(-0.220559927566779,0.0166341059157574,
0.000784537491144179));
#30405=CARTESIAN_POINT('Ctrl Pts',(-0.220601586758498,0.0166429502091465,
0.000394001417140767));
#30406=CARTESIAN_POINT('Ctrl Pts',(-0.22060155721139,0.0166430032112023,
3.29174539469179E-6));
#30407=CARTESIAN_POINT('Ctrl Pts',(-0.220601527573304,0.0166430563764536,
-0.000388620937738244));
#30408=CARTESIAN_POINT('Ctrl Pts',(-0.220559550159924,0.0166342277778145,
-0.000781963648253663));
#30409=CARTESIAN_POINT('Ctrl Pts',(-0.220478178797353,0.016618112703623,
-0.00116602012469409));
#30410=CARTESIAN_POINT('Ctrl Pts',(-0.220405693171807,0.0166037573924105,
-0.00150813770832684));
#30411=CARTESIAN_POINT('Ctrl Pts',(-0.220301947463313,0.0165836800531986,
-0.00184305410985848));
#30412=CARTESIAN_POINT('Ctrl Pts',(-0.220168746900573,0.0165605041990195,
-0.0021653437607661));
#30413=CARTESIAN_POINT('Ctrl Pts',(-0.220143927401298,0.016556185800627,
-0.00222539656829727));
#30414=CARTESIAN_POINT('Ctrl Pts',(-0.2201180830146,0.0165517570763484,
-0.00228504938166036));
#30415=CARTESIAN_POINT('Ctrl Pts',(-0.22009123609363,0.0165472297523478,
-0.00234431598932238));
#30416=CARTESIAN_POINT('Ctrl Pts',(-0.219965170557077,0.0165259707211935,
-0.00262261519179285));
#30417=CARTESIAN_POINT('Ctrl Pts',(-0.219816999384638,0.0164925356057389,
-0.00288799098246844));
#30418=CARTESIAN_POINT('Ctrl Pts',(-0.219649037008359,0.016450115766149,
-0.00314010411404311));
#30419=CARTESIAN_POINT('Ctrl Pts',(-0.219445305358693,0.0163986621960713,
-0.00344590726672758));
#30420=CARTESIAN_POINT('Ctrl Pts',(-0.219212476942563,0.0163339394016627,
-0.00373144395556523));
#30421=CARTESIAN_POINT('Ctrl Pts',(-0.218955730221358,0.0162632438912369,
-0.00399091800136782));
#30422=CARTESIAN_POINT('Ctrl Pts',(-0.218442236778948,0.0161218528703853,
-0.00450986609297299));
#30423=CARTESIAN_POINT('Ctrl Pts',(-0.217833090583353,0.0159569647380836,
-0.00492410039029786));
#30424=CARTESIAN_POINT('Ctrl Pts',(-0.217158667709042,0.0158301156325255,
-0.00520782050433744));
#30425=CARTESIAN_POINT('Ctrl Pts',(-0.216794280228025,0.0157615796622844,
-0.00536111313661152));
#30426=CARTESIAN_POINT('Ctrl Pts',(-0.216410834738256,0.0157042273221352,
-0.00547647426027126));
#30427=CARTESIAN_POINT('Ctrl Pts',(-0.216017823748763,0.0156661782184681,
-0.00555035855253401));
#30428=CARTESIAN_POINT('Ctrl Pts',(-0.21568343433353,0.0156338045244352,
-0.00561322225341056));
#30429=CARTESIAN_POINT('Ctrl Pts',(-0.215342120180744,0.0156154190771227,
-0.00564609861724332));
#30430=CARTESIAN_POINT('Ctrl Pts',(-0.214999728174719,0.0156143096410472,
-0.00564621361629089));
#30431=CARTESIAN_POINT('',(-0.192768466211737,0.0155323575322467,-0.00565446565602188));
#30432=CARTESIAN_POINT('Ctrl Pts',(-0.192768471267355,0.0155311142648402,
-0.00565367499839099));
#30433=CARTESIAN_POINT('Ctrl Pts',(-0.200178878547941,0.015561682319149,
-0.00565299192900956));
#30434=CARTESIAN_POINT('Ctrl Pts',(-0.207589299767349,0.0155894984464108,
-0.00565023605674504));
#30435=CARTESIAN_POINT('Ctrl Pts',(-0.214999727535123,0.0156143038560219,
-0.00564622471354199));
#30436=CARTESIAN_POINT('',(-0.186116972293536,0.00807761530404598,-0.00989662596793202));
#30437=CARTESIAN_POINT('Ctrl Pts',(-0.192768467297635,0.0155311217264212,
-0.00565366324004662));
#30438=CARTESIAN_POINT('Ctrl Pts',(-0.192553538631542,0.0154928316295278,
-0.00571249831822603));
#30439=CARTESIAN_POINT('Ctrl Pts',(-0.192126359873203,0.015400452164298,
-0.00585256845739566));
#30440=CARTESIAN_POINT('Ctrl Pts',(-0.191427233283813,0.0151794461386251,
-0.00616010599105498));
#30441=CARTESIAN_POINT('Ctrl Pts',(-0.190868940070598,0.0149513426159108,
-0.00645166872819745));
#30442=CARTESIAN_POINT('Ctrl Pts',(-0.190250537576569,0.0146393883647952,
-0.00681374640562836));
#30443=CARTESIAN_POINT('Ctrl Pts',(-0.189729516535842,0.0143200690862221,
-0.00714747621846582));
#30444=CARTESIAN_POINT('Ctrl Pts',(-0.189019762799825,0.0138059199805297,
-0.00763060364735688));
#30445=CARTESIAN_POINT('Ctrl Pts',(-0.188408531961533,0.0132414344427084,
-0.00807836328034344));
#30446=CARTESIAN_POINT('Ctrl Pts',(-0.187828208926315,0.0125602396324074,
-0.00852034249444996));
#30447=CARTESIAN_POINT('Ctrl Pts',(-0.187449134948595,0.0120341789970749,
-0.00881634519754376));
#30448=CARTESIAN_POINT('Ctrl Pts',(-0.187090455089954,0.0114381778019524,
-0.00910151919630248));
#30449=CARTESIAN_POINT('Ctrl Pts',(-0.186797972413645,0.0108473589238396,
-0.00933775607435096));
#30450=CARTESIAN_POINT('Ctrl Pts',(-0.186527846028905,0.0101622086658462,
-0.00955771999823304));
#30451=CARTESIAN_POINT('Ctrl Pts',(-0.186261990169622,0.00925438874498978,
-0.00977599514646285));
#30452=CARTESIAN_POINT('Ctrl Pts',(-0.186150558186061,0.00854952262296873,
-0.00986894325761661));
#30453=CARTESIAN_POINT('Ctrl Pts',(-0.186117379249033,0.0080775870920664,
-0.00989663768469957));
#30454=CARTESIAN_POINT('',(-0.186100495884658,0.00793881407698417,-0.00990361580204106));
#30455=CARTESIAN_POINT('Ctrl Pts',(-0.186100495884658,0.00793881407698417,
-0.00990361580204106));
#30456=CARTESIAN_POINT('Ctrl Pts',(-0.186107265118205,0.00798254987096854,
-0.00990176581450937));
#30457=CARTESIAN_POINT('Ctrl Pts',(-0.186113922409534,0.0080335687668118,
-0.00989921262958112));
#30458=CARTESIAN_POINT('Ctrl Pts',(-0.186116958557054,0.00807758863112322,
-0.00989662810000007));
#30459=CARTESIAN_POINT('',(-0.185999364351498,0.00750000000000023,-0.00991138348459597));
#30460=CARTESIAN_POINT('Ctrl Pts',(-0.185999469845766,0.00749998739549284,
-0.00991138532823997));
#30461=CARTESIAN_POINT('Ctrl Pts',(-0.186001338958666,0.00750760781264758,
-0.00991142760973324));
#30462=CARTESIAN_POINT('Ctrl Pts',(-0.186009114261658,0.00753659870661198,
-0.00991164463711701));
#30463=CARTESIAN_POINT('Ctrl Pts',(-0.18602099569412,0.00758276948028511,
-0.00991151377077237));
#30464=CARTESIAN_POINT('Ctrl Pts',(-0.186026938057374,0.0076058612673871,
-0.00991144831945915));
#30465=CARTESIAN_POINT('Ctrl Pts',(-0.186033907335661,0.00763325051566056,
-0.00991130411162516));
#30466=CARTESIAN_POINT('Ctrl Pts',(-0.186042705129421,0.00766942125256383,
-0.0099108628019639));
#30467=CARTESIAN_POINT('Ctrl Pts',(-0.18605150292318,0.00770559198946711,
-0.00991042149230265));
#30468=CARTESIAN_POINT('Ctrl Pts',(-0.186062131323826,0.00775054205776099,
-0.00990959055677255));
#30469=CARTESIAN_POINT('Ctrl Pts',(-0.186070367106067,0.00778657725573298,
-0.00990869847733454));
#30470=CARTESIAN_POINT('Ctrl Pts',(-0.186086838670548,0.00785864765167694,
-0.00990691431845853));
#30471=CARTESIAN_POINT('Ctrl Pts',(-0.18609372665111,0.00789507828299981,
-0.00990546578957274));
#30472=CARTESIAN_POINT('Ctrl Pts',(-0.186100495884658,0.00793881407698417,
-0.00990361580204106));
#30473=CARTESIAN_POINT('',(-0.186096190050249,0.0070814223423058,-0.00990442392752799));
#30474=CARTESIAN_POINT('Ctrl Pts',(-0.186096190050249,0.0070814223423058,
-0.00990442392752799));
#30475=CARTESIAN_POINT('Ctrl Pts',(-0.186077709288058,0.00718824343638535,
-0.00990892115509886));
#30476=CARTESIAN_POINT('Ctrl Pts',(-0.186046718946517,0.00732820276343046,
-0.00991245346926289));
#30477=CARTESIAN_POINT('Ctrl Pts',(-0.185999469351116,0.00750001479860198,
-0.00991138531705731));
#30478=CARTESIAN_POINT('',(-0.186116972875644,0.00692238473624832,-0.00989662598588015));
#30479=CARTESIAN_POINT('Ctrl Pts',(-0.186116959160015,0.00692241144484341,
-0.00989662811818303));
#30480=CARTESIAN_POINT('Ctrl Pts',(-0.186114180722263,0.00696269561858531,
-0.0098989933157357));
#30481=CARTESIAN_POINT('Ctrl Pts',(-0.186107547814753,0.00701580747228393,
-0.00990194593950673));
#30482=CARTESIAN_POINT('Ctrl Pts',(-0.186096190050249,0.0070814223423058,
-0.00990442392752799));
#30483=CARTESIAN_POINT('',(-0.192768468047837,-0.000531121860071518,-0.00565366303468581));
#30484=CARTESIAN_POINT('Ctrl Pts',(-0.186117379249032,0.00692241290794315,
-0.00989663768470023));
#30485=CARTESIAN_POINT('Ctrl Pts',(-0.186150547404768,0.00645063072958828,
-0.00986895225675147));
#30486=CARTESIAN_POINT('Ctrl Pts',(-0.186261932611995,0.00574597187644414,
-0.00977604664100172));
#30487=CARTESIAN_POINT('Ctrl Pts',(-0.186527643355928,0.00483841251243376,
-0.0095578911982986));
#30488=CARTESIAN_POINT('Ctrl Pts',(-0.186797662606925,0.00415336530792349,
-0.00933800703012731));
#30489=CARTESIAN_POINT('Ctrl Pts',(-0.187089867547376,0.00356288427383543,
-0.00910198973672387));
#30490=CARTESIAN_POINT('Ctrl Pts',(-0.187448677686789,0.00296655606527825,
-0.00881670870907843));
#30491=CARTESIAN_POINT('Ctrl Pts',(-0.18782652671858,0.00244197053597788,
-0.00852164547016561));
#30492=CARTESIAN_POINT('Ctrl Pts',(-0.188405806126936,0.00176150898886227,
-0.00808041909580759));
#30493=CARTESIAN_POINT('Ctrl Pts',(-0.189013908627982,0.00119895188987953,
-0.00763477774095243));
#30494=CARTESIAN_POINT('Ctrl Pts',(-0.189725220968284,0.000682672430095184,
-0.00715027528319919));
#30495=CARTESIAN_POINT('Ctrl Pts',(-0.19024844359526,0.000361785469120427,
-0.00681503282008351));
#30496=CARTESIAN_POINT('Ctrl Pts',(-0.19086389333632,5.11131219040483E-5,
-0.00645458607971318));
#30497=CARTESIAN_POINT('Ctrl Pts',(-0.191418362838009,-0.000176268882400119,
-0.00616437018057724));
#30498=CARTESIAN_POINT('Ctrl Pts',(-0.192123247609021,-0.000399817339443113,
-0.00585356940633785));
#30499=CARTESIAN_POINT('Ctrl Pts',(-0.192552358590443,-0.000492621421588735,
-0.00571282131797196));
#30500=CARTESIAN_POINT('Ctrl Pts',(-0.192768468047837,-0.000531121860071518,
-0.00565366303468581));
#30501=CARTESIAN_POINT('',(-0.214999728174719,-0.000614309641048097,-0.00564621361629096));
#30502=CARTESIAN_POINT('Ctrl Pts',(-0.214999727480966,-0.000614303178801771,
-0.00564622601275543));
#30503=CARTESIAN_POINT('Ctrl Pts',(-0.207589299761315,-0.000589501940551079,
-0.00565022926213394));
#30504=CARTESIAN_POINT('Ctrl Pts',(-0.200178878524307,-0.000561687127315493,
-0.00565298419618518));
#30505=CARTESIAN_POINT('Ctrl Pts',(-0.192768471170869,-0.000531115971629387,
-0.00565367231393811));
#30506=CARTESIAN_POINT('',(-0.214999728175217,-0.000614308556352198,0.00564621407322208));
#30507=CARTESIAN_POINT('Ctrl Pts',(-0.214999728174719,-0.000614309641048097,
-0.00564621361629096));
#30508=CARTESIAN_POINT('Ctrl Pts',(-0.21573850211318,-0.000616703454117696,
-0.0056459654846237));
#30509=CARTESIAN_POINT('Ctrl Pts',(-0.217223304763531,-0.000790930473226734,
-0.00533944491480338));
#30510=CARTESIAN_POINT('Ctrl Pts',(-0.218746260771501,-0.00120277693812265,
-0.00430233875808143));
#30511=CARTESIAN_POINT('Ctrl Pts',(-0.219676141040077,-0.00146568982444615,
-0.00316380099642141));
#30512=CARTESIAN_POINT('Ctrl Pts',(-0.220374968741458,-0.0016004092271873,
-0.00185706856797699));
#30513=CARTESIAN_POINT('Ctrl Pts',(-0.22075211591453,-0.00167135211208185,
-4.24711954689424E-6));
#30514=CARTESIAN_POINT('Ctrl Pts',(-0.220376469572862,-0.0016005504927844,
0.00185335284380898));
#30515=CARTESIAN_POINT('Ctrl Pts',(-0.219678171970889,-0.0014662512330438,
0.00316084634731099));
#30516=CARTESIAN_POINT('Ctrl Pts',(-0.218746792417777,-0.00120287411926783,
0.00430240406335488));
#30517=CARTESIAN_POINT('Ctrl Pts',(-0.217223954144023,-0.000791566407931855,
0.00533790744423129));
#30518=CARTESIAN_POINT('Ctrl Pts',(-0.215744536661587,-0.000616721921800092,
0.00564596392366559));
#30519=CARTESIAN_POINT('Ctrl Pts',(-0.214999728175217,-0.000614308556352198,
0.00564621407322208));
#30520=CARTESIAN_POINT('',(-0.192768467995111,-0.000531121635157075,0.00565366251134238));
#30521=CARTESIAN_POINT('Ctrl Pts',(-0.192768468030036,-0.00053111358431346,
0.00565367517106098));
#30522=CARTESIAN_POINT('Ctrl Pts',(-0.200178876390431,-0.00056168139528131,
0.00565299213563766));
#30523=CARTESIAN_POINT('Ctrl Pts',(-0.20758929868895,-0.000589497383419672,
0.00565023637807718));
#30524=CARTESIAN_POINT('Ctrl Pts',(-0.214999727535667,-0.000614302771609743,
0.00564622516979113));
#30525=CARTESIAN_POINT('Ctrl Pts',(-0.192768462908899,-0.000531120840243836,
0.00565366372878243));
#30526=CARTESIAN_POINT('Ctrl Pts',(-0.192552801493728,-0.000492700078165468,
0.00571269932462467));
#30527=CARTESIAN_POINT('Ctrl Pts',(-0.192124458781824,-0.000400070483159716,
0.00585317259136444));
#30528=CARTESIAN_POINT('Ctrl Pts',(-0.191421518043594,-0.000177397871371761,
0.00616285200383273));
#30529=CARTESIAN_POINT('Ctrl Pts',(-0.190866264373635,5.00112782188013E-5,
0.0064532469370294));
#30530=CARTESIAN_POINT('Ctrl Pts',(-0.190250499708039,0.00036063440493152,
0.00681376176935662));
#30531=CARTESIAN_POINT('Ctrl Pts',(-0.189727113151071,0.000681405916027528,
0.00714901524785936));
#30532=CARTESIAN_POINT('Ctrl Pts',(-0.189015316243516,0.00119775071995663,
0.0076337612796465));
#30533=CARTESIAN_POINT('Ctrl Pts',(-0.188406936412897,0.00176034576435437,
0.00807957177832989));
#30534=CARTESIAN_POINT('Ctrl Pts',(-0.187827448741697,0.0024407808400988,
0.00852093044215746));
#30535=CARTESIAN_POINT('Ctrl Pts',(-0.187449339498272,0.00296554636590169,
0.00881618573576621));
#30536=CARTESIAN_POINT('Ctrl Pts',(-0.187090406949154,0.00356188460332164,
0.00910155665687714));
#30537=CARTESIAN_POINT('Ctrl Pts',(-0.186797998280614,0.00415259607751215,
0.00933773637730888));
#30538=CARTESIAN_POINT('Ctrl Pts',(-0.186527846972215,0.00483778154507395,
0.00955771997476887));
#30539=CARTESIAN_POINT('Ctrl Pts',(-0.186352129082402,0.00543781226559763,
0.0097019893028026));
#30540=CARTESIAN_POINT('Ctrl Pts',(-0.18626928197773,0.0058180982296112,
0.00977044711790262));
#30541=CARTESIAN_POINT('Ctrl Pts',(-0.186240951883218,0.00596786139892777,
0.00979390672266723));
#30542=CARTESIAN_POINT('',(-0.190954534254184,0.00352393167612197,0.00915627380277794));
#30543=CARTESIAN_POINT('Ctrl Pts',(-0.190954534310351,0.00352393181819051,
0.00915627369813247));
#30544=CARTESIAN_POINT('Ctrl Pts',(-0.19094632664236,0.00362759799902633,
0.00920360461773492));
#30545=CARTESIAN_POINT('Ctrl Pts',(-0.19093545240702,0.00376077062731066,
0.00926213843487851));
#30546=CARTESIAN_POINT('Ctrl Pts',(-0.190924142450368,0.00391598246737441,
0.00932477587001288));
#30547=CARTESIAN_POINT('Ctrl Pts',(-0.190918487472042,0.00399358838740629,
0.00935609458758006));
#30548=CARTESIAN_POINT('Ctrl Pts',(-0.190912721390573,0.00407665332153031,
0.0093885448454316));
#30549=CARTESIAN_POINT('Ctrl Pts',(-0.190906716936133,0.00417452738184911,
0.00942477637181333));
#30550=CARTESIAN_POINT('Ctrl Pts',(-0.190904087456934,0.00421738852908344,
0.00944064293320573));
#30551=CARTESIAN_POINT('Ctrl Pts',(-0.190901414383111,0.00426310553578685,
0.00945719956921678));
#30552=CARTESIAN_POINT('Ctrl Pts',(-0.190898866584097,0.00430862868740381,
0.00947328023960344));
#30553=CARTESIAN_POINT('Ctrl Pts',(-0.190895596446577,0.00436705832227904,
0.00949392001663707));
#30554=CARTESIAN_POINT('Ctrl Pts',(-0.19089253268803,0.00442517237653945,
0.00951376128014555));
#30555=CARTESIAN_POINT('Ctrl Pts',(-0.190890032378645,0.00447636934260713,
0.00953078141909249));
#30556=CARTESIAN_POINT('Ctrl Pts',(-0.190885584051554,0.00456745441089561,
0.00956106212979344));
#30557=CARTESIAN_POINT('Ctrl Pts',(-0.190882904338584,0.00463651587043694,
0.00958281759923728));
#30558=CARTESIAN_POINT('Ctrl Pts',(-0.190880531451168,0.00471329694686104,
0.00960615849718409));
#30559=CARTESIAN_POINT('Ctrl Pts',(-0.190878158563751,0.00479007802328515,
0.00962949939513091));
#30560=CARTESIAN_POINT('Ctrl Pts',(-0.190876100121299,0.00487468124703968,
0.00965407619729078));
#30561=CARTESIAN_POINT('Ctrl Pts',(-0.190874739449471,0.00495722266620057,
0.00967681019044906));
#30562=CARTESIAN_POINT('Ctrl Pts',(-0.190873378777642,0.00503976408536146,
0.00969954418360734));
#30563=CARTESIAN_POINT('Ctrl Pts',(-0.190872712070185,0.00512019613320558,
0.0097206091211127));
#30564=CARTESIAN_POINT('Ctrl Pts',(-0.190872856109916,0.00520802569623835,
0.00974229097280704));
#30565=CARTESIAN_POINT('Ctrl Pts',(-0.190873000149648,0.00529585525927111,
0.00976397282450137));
#30566=CARTESIAN_POINT('Ctrl Pts',(-0.190873962538537,0.00539117015513677,
0.00978592595965043));
#30567=CARTESIAN_POINT('Ctrl Pts',(-0.190875081406697,0.00546555964115924,
0.00980214880648675));
#30568=CARTESIAN_POINT('Ctrl Pts',(-0.190876200274857,0.0055399491271817,
0.00981837165332308));
#30569=CARTESIAN_POINT('Ctrl Pts',(-0.190877463096275,0.00559329168544975,
0.00982942944626223));
#30570=CARTESIAN_POINT('Ctrl Pts',(-0.190879780185886,0.00566986525134087,
0.00984441872877178));
#30571=CARTESIAN_POINT('Ctrl Pts',(-0.190882097275498,0.005746438817232,
0.00985940801128134));
#30572=CARTESIAN_POINT('Ctrl Pts',(-0.190885478987397,0.00584632900620433,
0.00987786397855303));
#30573=CARTESIAN_POINT('Ctrl Pts',(-0.19089009347875,0.00595176589423788,
0.00989528793015295));
#30574=CARTESIAN_POINT('Ctrl Pts',(-0.190890175357787,0.00595363675501567,
0.00989559709887227));
#30575=CARTESIAN_POINT('Ctrl Pts',(-0.190890257625829,0.00595550936098245,
0.00989590599388756));
#30576=CARTESIAN_POINT('Ctrl Pts',(-0.190890340272952,0.00595738356554221,
0.00989621458805049));
#30577=CARTESIAN_POINT('',(-0.19155098689841,0.00310490369588466,0.00896382639094083));
#30578=CARTESIAN_POINT('Ctrl Pts',(-0.190954506945739,0.00352390963011318,
0.00915626296509413));
#30579=CARTESIAN_POINT('Ctrl Pts',(-0.190982278824996,0.00349425566396222,
0.00914324986724137));
#30580=CARTESIAN_POINT('Ctrl Pts',(-0.19101331050615,0.00346142897667129,
0.00912863700187908));
#30581=CARTESIAN_POINT('Ctrl Pts',(-0.191107038094531,0.00337454011628438,
0.00908963731875738));
#30582=CARTESIAN_POINT('Ctrl Pts',(-0.191230009334021,0.00328208373715836,
0.00904716953434546));
#30583=CARTESIAN_POINT('Ctrl Pts',(-0.191371313193077,0.00319458454024611,
0.00900637041021926));
#30584=CARTESIAN_POINT('Ctrl Pts',(-0.19149550396465,0.0031312929367007,
0.00897638835379347));
#30585=CARTESIAN_POINT('Ctrl Pts',(-0.19155044938687,0.00310515928473931,
0.00896394806017618));
#30586=CARTESIAN_POINT('',(-0.192244127898258,0.0028370269379133,0.00883272019762234));
#30587=CARTESIAN_POINT('Ctrl Pts',(-0.19155098689841,0.00310490369588466,
0.00896382639094083));
#30588=CARTESIAN_POINT('Ctrl Pts',(-0.191605706721645,0.00307889106552294,
0.00895144323092614));
#30589=CARTESIAN_POINT('Ctrl Pts',(-0.191677276008409,0.00304801612626287,
0.00893663613670419));
#30590=CARTESIAN_POINT('Ctrl Pts',(-0.191792352343094,0.00300073160810067,
0.00891381119032522));
#30591=CARTESIAN_POINT('Ctrl Pts',(-0.19190916590961,0.00295569191589503,
0.00889185169317019));
#30592=CARTESIAN_POINT('Ctrl Pts',(-0.191939972002056,0.00294429797831757,
0.00888625973348703));
#30593=CARTESIAN_POINT('Ctrl Pts',(-0.192048790468399,0.0029037328706347,
0.00886629204061889));
#30594=CARTESIAN_POINT('Ctrl Pts',(-0.192155294606237,0.00286458613052319,
0.00884674800931049));
#30595=CARTESIAN_POINT('Ctrl Pts',(-0.192242576586721,0.00283267476154068,
0.00883054397400312));
#30596=CARTESIAN_POINT('',(-0.19208322262791,0.00464057435056716,0.00960976448008655));
#30597=CARTESIAN_POINT('Ctrl Pts',(-0.19208322262791,0.00464057435056716,
0.00960976448008655));
#30598=CARTESIAN_POINT('Ctrl Pts',(-0.192085206341064,0.00459342467188857,
0.00959502212455125));
#30599=CARTESIAN_POINT('Ctrl Pts',(-0.192087617750331,0.00454199577158409,
0.00957848718067775));
#30600=CARTESIAN_POINT('Ctrl Pts',(-0.192090642929679,0.0044854654686816,
0.00955971369095227));
#30601=CARTESIAN_POINT('Ctrl Pts',(-0.192093681203115,0.0044286904818797,
0.00954085894267279));
#30602=CARTESIAN_POINT('Ctrl Pts',(-0.192097341832823,0.00436678587514305,
0.00951968523993041));
#30603=CARTESIAN_POINT('Ctrl Pts',(-0.192101377292397,0.00430349575245546,
0.00949723790948274));
#30604=CARTESIAN_POINT('Ctrl Pts',(-0.192105910696384,0.00423239611949469,
0.00947202075255517));
#30605=CARTESIAN_POINT('Ctrl Pts',(-0.19211091713946,0.00415955363953229,
0.00944518465642903));
#30606=CARTESIAN_POINT('Ctrl Pts',(-0.19211604569542,0.00409011964816775,
0.00941867243889797));
#30607=CARTESIAN_POINT('Ctrl Pts',(-0.192135433288675,0.00382763679854969,
0.0093184477179726));
#30608=CARTESIAN_POINT('Ctrl Pts',(-0.192156497399979,0.00361313712343995,
0.00922457021543034));
#30609=CARTESIAN_POINT('Ctrl Pts',(-0.192178551157702,0.00340772429612771,
0.00912725829435275));
#30610=CARTESIAN_POINT('Ctrl Pts',(-0.192200186009473,0.00320621323724796,
0.00903179479037128));
#30611=CARTESIAN_POINT('Ctrl Pts',(-0.192222796816838,0.00301409159924088,
0.00893185014394745));
#30612=CARTESIAN_POINT('Ctrl Pts',(-0.19224448913935,0.00284151729909065,
0.00883554521382252));
#30613=CARTESIAN_POINT('',(-0.192075122449827,0.00543334712284603,0.00982163800799055));
#30614=CARTESIAN_POINT('Ctrl Pts',(-0.192075122449827,0.00543334712284603,
0.00982163800799055));
#30615=CARTESIAN_POINT('Ctrl Pts',(-0.192073745904168,0.00537589936645501,
0.00980887345605507));
#30616=CARTESIAN_POINT('Ctrl Pts',(-0.192072795708241,0.00532266174270566,
0.00979647660250808));
#30617=CARTESIAN_POINT('Ctrl Pts',(-0.192072170762121,0.00527270892376701,
0.00978447083173468));
#30618=CARTESIAN_POINT('Ctrl Pts',(-0.192071143546597,0.00519060214775848,
0.00976473710794001));
#30619=CARTESIAN_POINT('Ctrl Pts',(-0.192070999692292,0.0051174235825934,
0.00974584944479457));
#30620=CARTESIAN_POINT('Ctrl Pts',(-0.19207108592788,0.00508480464904163,
0.00973731727043851));
#30621=CARTESIAN_POINT('Ctrl Pts',(-0.192071129045674,0.00506849518226574,
0.00973305118326047));
#30622=CARTESIAN_POINT('Ctrl Pts',(-0.192071228710843,0.00506231357119921,
0.00973141845477906));
#30623=CARTESIAN_POINT('Ctrl Pts',(-0.192071444468926,0.00504813553730963,
0.00972765351664012));
#30624=CARTESIAN_POINT('Ctrl Pts',(-0.19207166022701,0.00503395750342006,
0.00972388857850117));
#30625=CARTESIAN_POINT('Ctrl Pts',(-0.192071992671388,0.00501179032802861,
0.00971796436653364));
#30626=CARTESIAN_POINT('Ctrl Pts',(-0.192072495237599,0.0049858984125824,
0.009710903448484));
#30627=CARTESIAN_POINT('Ctrl Pts',(-0.19207350037002,0.00493411458168996,
0.00969678161238471));
#30628=CARTESIAN_POINT('Ctrl Pts',(-0.192075184614482,0.00486741174909846,
0.00967817636683549));
#30629=CARTESIAN_POINT('Ctrl Pts',(-0.192077858011542,0.00478539381423263,
0.00965389070203072));
#30630=CARTESIAN_POINT('Ctrl Pts',(-0.192079277812855,0.00474183531206385,
0.0096409929475969));
#30631=CARTESIAN_POINT('Ctrl Pts',(-0.192080975907986,0.00469395101363589,
0.00962652426427693));
#30632=CARTESIAN_POINT('Ctrl Pts',(-0.19208322262791,0.00464057435056716,
0.00960976448008655));
#30633=CARTESIAN_POINT('Ctrl Pts',(-0.192094713079881,0.00595467555603429,
0.0099226782462026));
#30634=CARTESIAN_POINT('Ctrl Pts',(-0.192093438683974,0.0059288836017015,
0.00991841040641334));
#30635=CARTESIAN_POINT('Ctrl Pts',(-0.192092050254312,0.00590009560033358,
0.00991353641647854));
#30636=CARTESIAN_POINT('Ctrl Pts',(-0.192090655876427,0.0058695679699555,
0.00990820459990516));
#30637=CARTESIAN_POINT('Ctrl Pts',(-0.192086141620258,0.00577073569120594,
0.00989094300523516));
#30638=CARTESIAN_POINT('Ctrl Pts',(-0.19208157119045,0.00565371489836332,
0.00986856917129485));
#30639=CARTESIAN_POINT('Ctrl Pts',(-0.192078337556395,0.00554975597457726,
0.00984678202053675));
#30640=CARTESIAN_POINT('Ctrl Pts',(-0.192077071228137,0.00550904446530914,
0.00983824992191826));
#30641=CARTESIAN_POINT('Ctrl Pts',(-0.192076008513737,0.00547032319090132,
0.00982987069770896));
#30642=CARTESIAN_POINT('Ctrl Pts',(-0.192075122449827,0.00543334712284603,
0.00982163800799055));
#30643=CARTESIAN_POINT('',(-0.193087902622454,0.00259433627597418,0.00870850447702694));
#30644=CARTESIAN_POINT('Ctrl Pts',(-0.192891760060441,0.00595287508888906,
0.00994024214377629));
#30645=CARTESIAN_POINT('Ctrl Pts',(-0.192890566945838,0.00592739245907241,
0.00993600999446998));
#30646=CARTESIAN_POINT('Ctrl Pts',(-0.192884601854086,0.0057942541567979,
0.00991325429118574));
#30647=CARTESIAN_POINT('Ctrl Pts',(-0.192872041248742,0.0054401365750408,
0.00984514869329706));
#30648=CARTESIAN_POINT('Ctrl Pts',(-0.192866762099152,0.00495868049753787,
0.00972769113725174));
#30649=CARTESIAN_POINT('Ctrl Pts',(-0.192885277880319,0.00432843397316892,
0.00953146350645171));
#30650=CARTESIAN_POINT('Ctrl Pts',(-0.192925778339018,0.00382224510393984,
0.00933240208330745));
#30651=CARTESIAN_POINT('Ctrl Pts',(-0.19296164636954,0.00350616168796143,
0.00919061074969547));
#30652=CARTESIAN_POINT('Ctrl Pts',(-0.192985497265266,0.00331338011994894,
0.00909895014912776));
#30653=CARTESIAN_POINT('Ctrl Pts',(-0.193008594946383,0.00314020797556435,
0.00901202176798678));
#30654=CARTESIAN_POINT('Ctrl Pts',(-0.193020791858502,0.00305306311402364,
0.00896654755713946));
#30655=CARTESIAN_POINT('Ctrl Pts',(-0.193046579479833,0.00287167102747878,
0.0088696212197973));
#30656=CARTESIAN_POINT('Ctrl Pts',(-0.19306986918682,0.00271385629159264,
0.00878009081354476));
#30657=CARTESIAN_POINT('Ctrl Pts',(-0.193087902622454,0.00259433627597418,
0.00870850447702694));
#30658=CARTESIAN_POINT('',(-0.194289733361641,0.00259543694850618,0.00873259552391554));
#30659=CARTESIAN_POINT('',(-0.193087902747045,0.0025943401192753,0.00870849809117663));
#30660=CARTESIAN_POINT('Ctrl Pts',(-0.194289733361641,0.00259543694850618,
0.00873259552391554));
#30661=CARTESIAN_POINT('Ctrl Pts',(-0.194271528725811,0.00271568039656882,
0.00880482321695224));
#30662=CARTESIAN_POINT('Ctrl Pts',(-0.194255897964241,0.00282122439999286,
0.00886474330262958));
#30663=CARTESIAN_POINT('Ctrl Pts',(-0.194242056106171,0.00291670895493246,
0.00891714289225702));
#30664=CARTESIAN_POINT('Ctrl Pts',(-0.194235135148102,0.00296445143268365,
0.00894334279698027));
#30665=CARTESIAN_POINT('Ctrl Pts',(-0.194228662428445,0.00300970838330853,
0.00896761155435052));
#30666=CARTESIAN_POINT('Ctrl Pts',(-0.194223419901485,0.00304661531765659,
0.0089871258554761));
#30667=CARTESIAN_POINT('Ctrl Pts',(-0.194218177374525,0.00308352225200465,
0.00900664015660169));
#30668=CARTESIAN_POINT('Ctrl Pts',(-0.194214162614404,0.00311201443001013,
0.00902152057309972));
#30669=CARTESIAN_POINT('Ctrl Pts',(-0.194208252055201,0.00315520779816521,
0.00904365403355806));
#30670=CARTESIAN_POINT('Ctrl Pts',(-0.194202341495998,0.00319840116632029,
0.0090657874940164));
#30671=CARTESIAN_POINT('Ctrl Pts',(-0.194194539515255,0.00325640731426551,
0.00909495824185457));
#30672=CARTESIAN_POINT('Ctrl Pts',(-0.19418763059952,0.0033095193635379,
0.0091209708909162));
#30673=CARTESIAN_POINT('Ctrl Pts',(-0.194180721683785,0.00336263141281028,
0.00914698353997783));
#30674=CARTESIAN_POINT('Ctrl Pts',(-0.1941747028172,0.00341077872854798,
0.00916998462247426));
#30675=CARTESIAN_POINT('Ctrl Pts',(-0.194168967265586,0.00345787450382826,
0.00919205245244361));
#30676=CARTESIAN_POINT('Ctrl Pts',(-0.194157496162359,0.00355206605438881,
0.00923618811238231));
#30677=CARTESIAN_POINT('Ctrl Pts',(-0.194147158641889,0.00364205090957071,
0.00927657770576536));
#30678=CARTESIAN_POINT('Ctrl Pts',(-0.194137514962956,0.0037358380241254,
0.00931692735652691));
#30679=CARTESIAN_POINT('Ctrl Pts',(-0.194119406580828,0.0039119464284688,
0.0093926937626603));
#30680=CARTESIAN_POINT('Ctrl Pts',(-0.19410375587135,0.0041016834482665,
0.00946781093462956));
#30681=CARTESIAN_POINT('Ctrl Pts',(-0.194092490888446,0.004294996654283,
0.00953690694685357));
#30682=CARTESIAN_POINT('Ctrl Pts',(-0.19409175746337,0.00430758262571006,
0.00954140555537337));
#30683=CARTESIAN_POINT('Ctrl Pts',(-0.194091042628832,0.00432018336915257,
0.00954587951955885));
#30684=CARTESIAN_POINT('Ctrl Pts',(-0.194090346916936,0.00433279593942552,
0.00955032777148575));
#30685=CARTESIAN_POINT('Ctrl Pts',(-0.19407896547467,0.00453913025852806,
0.00962309858763756));
#30686=CARTESIAN_POINT('Ctrl Pts',(-0.194072700655243,0.00474875923096642,
0.00968875779931998));
#30687=CARTESIAN_POINT('Ctrl Pts',(-0.194070631885882,0.00494981833866685,
0.00974471116442283));
#30688=CARTESIAN_POINT('Ctrl Pts',(-0.194068563116522,0.00515087744636728,
0.00980066452952569));
#30689=CARTESIAN_POINT('Ctrl Pts',(-0.19407067236164,0.0053431217362215,
0.00984773853892592));
#30690=CARTESIAN_POINT('Ctrl Pts',(-0.194076586118239,0.00555334261219932,
0.00989187662448376));
#30691=CARTESIAN_POINT('Ctrl Pts',(-0.194079542996539,0.00565845305018821,
0.00991394566726268));
#30692=CARTESIAN_POINT('Ctrl Pts',(-0.19408345578846,0.00576810145447717,
0.00993506549656636));
#30693=CARTESIAN_POINT('Ctrl Pts',(-0.194088151554064,0.00587655136153835,
0.00995399441587651));
#30694=CARTESIAN_POINT('Ctrl Pts',(-0.194089210184997,0.00590100071357329,
0.00995826182213251));
#30695=CARTESIAN_POINT('Ctrl Pts',(-0.194090308396205,0.00592538822477612,
0.00996242241717579));
#30696=CARTESIAN_POINT('Ctrl Pts',(-0.194091473879223,0.00595018587709226,
0.00996655302891216));
#30697=CARTESIAN_POINT('',(-0.19508880402446,0.00259613937631384,0.00874861526161622));
#30698=CARTESIAN_POINT('Ctrl Pts',(-0.194890827700361,0.00594838029502342,
0.00998416681136753));
#30699=CARTESIAN_POINT('Ctrl Pts',(-0.194889713960232,0.00592436947855236,
0.00998014991521366));
#30700=CARTESIAN_POINT('Ctrl Pts',(-0.194883852863042,0.00579261937904974,
0.00995750870450058));
#30701=CARTESIAN_POINT('Ctrl Pts',(-0.19487142704807,0.00543995741384574,
0.00988940370129619));
#30702=CARTESIAN_POINT('Ctrl Pts',(-0.194866284257113,0.0049586687135079,
0.00977150277032712));
#30703=CARTESIAN_POINT('Ctrl Pts',(-0.194885044401134,0.00432865252952493,
0.00957453103971056));
#30704=CARTESIAN_POINT('Ctrl Pts',(-0.19492582233458,0.00382278364537034,
0.00937473168531034));
#30705=CARTESIAN_POINT('Ctrl Pts',(-0.194961893178176,0.00350696808990623,
0.00923242757156718));
#30706=CARTESIAN_POINT('Ctrl Pts',(-0.194985873725367,0.00331435951877626,
0.00914043502989879));
#30707=CARTESIAN_POINT('Ctrl Pts',(-0.195009093344523,0.00314135359488825,
0.00905319208558937));
#30708=CARTESIAN_POINT('Ctrl Pts',(-0.195021352135067,0.00305430708509385,
0.00900755901258544));
#30709=CARTESIAN_POINT('Ctrl Pts',(-0.195047271623395,0.00287311693036189,
0.00891029014674232));
#30710=CARTESIAN_POINT('Ctrl Pts',(-0.195070679357827,0.00271549678394977,
0.00882044735032797));
#30711=CARTESIAN_POINT('Ctrl Pts',(-0.19508880402446,0.00259613937631384,
0.00874861526161622));
#30712=CARTESIAN_POINT('',(-0.19629064847218,0.00259721050736435,0.00877274833518847));
#30713=CARTESIAN_POINT('',(-0.195088804147468,0.0025961431799468,0.00874860897199265));
#30714=CARTESIAN_POINT('Ctrl Pts',(-0.19629064847218,0.00259721050736436,
0.00877274833518847));
#30715=CARTESIAN_POINT('Ctrl Pts',(-0.196272353578319,0.0027173147463442,
0.00884523531704338));
#30716=CARTESIAN_POINT('Ctrl Pts',(-0.196256645487058,0.00282274836854239,
0.00890537208131317));
#30717=CARTESIAN_POINT('Ctrl Pts',(-0.196242734961374,0.00291813783584734,
0.00895796128107918));
#30718=CARTESIAN_POINT('Ctrl Pts',(-0.196235779668928,0.00296583277249766,
0.00898425599287699));
#30719=CARTESIAN_POINT('Ctrl Pts',(-0.196229274785596,0.00301104622815838,
0.0090086126430062));
#30720=CARTESIAN_POINT('Ctrl Pts',(-0.196224006516798,0.00304791619144044,
0.00902819648410093));
#30721=CARTESIAN_POINT('Ctrl Pts',(-0.196218738248,0.00308478615472249,
0.00904778032519565));
#30722=CARTESIAN_POINT('Ctrl Pts',(-0.196214704155585,0.00311324738212467,
0.00906271231000411));
#30723=CARTESIAN_POINT('Ctrl Pts',(-0.196208763690641,0.00315640258061905,
0.00908492642526198));
#30724=CARTESIAN_POINT('Ctrl Pts',(-0.196202823225698,0.00319955777911343,
0.00910714054051985));
#30725=CARTESIAN_POINT('Ctrl Pts',(-0.196194980787967,0.00325751941637139,
0.00913642031755311));
#30726=CARTESIAN_POINT('Ctrl Pts',(-0.196188035587219,0.00331059184700996,
0.00916252984284632));
#30727=CARTESIAN_POINT('Ctrl Pts',(-0.196181090386472,0.00336366427764853,
0.00918863936813953));
#30728=CARTESIAN_POINT('Ctrl Pts',(-0.196175039391781,0.00341177630756539,
0.00921172568002843));
#30729=CARTESIAN_POINT('Ctrl Pts',(-0.196169272892308,0.00345883730293629,
0.00923387466272813));
#30730=CARTESIAN_POINT('Ctrl Pts',(-0.19615773989336,0.00355295929367808,
0.00927817262812752));
#30731=CARTESIAN_POINT('Ctrl Pts',(-0.196147345195326,0.00364287649867495,
0.00931870835293598));
#30732=CARTESIAN_POINT('Ctrl Pts',(-0.196137643728015,0.00373661105067373,
0.00935920966817614));
#30733=CARTESIAN_POINT('Ctrl Pts',(-0.196119713132662,0.00390985456823773,
0.0094340656329037));
#30734=CARTESIAN_POINT('Ctrl Pts',(-0.196104161588853,0.00409635321035026,
0.0095083139085995));
#30735=CARTESIAN_POINT('Ctrl Pts',(-0.196092843570277,0.00428645811893465,
0.00957676005490717));
#30736=CARTESIAN_POINT('Ctrl Pts',(-0.196091914211108,0.00430206824880583,
0.00958238038970547));
#30737=CARTESIAN_POINT('Ctrl Pts',(-0.196091013396839,0.0043177021066952,
0.00958796292404868));
#30738=CARTESIAN_POINT('Ctrl Pts',(-0.196090142154209,0.00433335401676975,
0.009593505584366));
#30739=CARTESIAN_POINT('Ctrl Pts',(-0.19607866065389,0.00453961964745067,
0.00966654844754104));
#30740=CARTESIAN_POINT('Ctrl Pts',(-0.196072313469605,0.00474915014441373,
0.00973243826951178));
#30741=CARTESIAN_POINT('Ctrl Pts',(-0.196070177583228,0.00495016153240564,
0.00978859876622602));
#30742=CARTESIAN_POINT('Ctrl Pts',(-0.196068041696851,0.00515117292039755,
0.00984475926294027));
#30743=CARTESIAN_POINT('Ctrl Pts',(-0.196070099062835,0.00534341906999027,
0.00989201695645952));
#30744=CARTESIAN_POINT('Ctrl Pts',(-0.196075967808123,0.00555364142327267,
0.00993632357023678));
#30745=CARTESIAN_POINT('Ctrl Pts',(-0.196078902180768,0.00565875259991386,
0.0099584768771254));
#30746=CARTESIAN_POINT('Ctrl Pts',(-0.196082794197006,0.0057684019450636,
0.00997967664938378));
#30747=CARTESIAN_POINT('Ctrl Pts',(-0.196087472032619,0.00587685690239138,
0.00999867723685306));
#30748=CARTESIAN_POINT('Ctrl Pts',(-0.196088458447276,0.00589972678674669,
0.0100026838885434));
#30749=CARTESIAN_POINT('Ctrl Pts',(-0.196089479615871,0.0059225427625479,
0.0100065966003908));
#30750=CARTESIAN_POINT('Ctrl Pts',(-0.196090558152439,0.0059456909738631,
0.0100104788652639));
#30751=CARTESIAN_POINT('',(-0.197089662404178,0.00259797405121459,0.00878884347189939));
#30752=CARTESIAN_POINT('Ctrl Pts',(-0.196889861047832,0.00594388566779889,
0.0100280902017948));
#30753=CARTESIAN_POINT('Ctrl Pts',(-0.196888837648877,0.00592159442464991,
0.010024333805948));
#30754=CARTESIAN_POINT('Ctrl Pts',(-0.196883091265258,0.00579144662888638,
0.0100018530788455));
#30755=CARTESIAN_POINT('Ctrl Pts',(-0.196870803496027,0.00544040664358776,
0.00993381410319575));
#30756=CARTESIAN_POINT('Ctrl Pts',(-0.196865788922285,0.00495923422978679,
0.00981549844312244));
#30757=CARTESIAN_POINT('Ctrl Pts',(-0.196884784226902,0.00432929226751012,
0.00961778687411515));
#30758=CARTESIAN_POINT('Ctrl Pts',(-0.196925834282415,0.00382363098333961,
0.00941724253688526));
#30759=CARTESIAN_POINT('Ctrl Pts',(-0.196962104915578,0.00350801189151409,
0.009274415400131));
#30760=CARTESIAN_POINT('Ctrl Pts',(-0.196986213416204,0.00331553231284704,
0.00918208265328692));
#30761=CARTESIAN_POINT('Ctrl Pts',(-0.197009553267731,0.00314265469214262,
0.00909451705606134));
#30762=CARTESIAN_POINT('Ctrl Pts',(-0.19702187385383,0.0030556819289598,
0.00904871761708454));
#30763=CARTESIAN_POINT('Ctrl Pts',(-0.197047923761315,0.00287465209234715,
0.0089510947199911));
#30764=CARTESIAN_POINT('Ctrl Pts',(-0.197071447917473,0.00271719298855498,
0.00886092932785962));
#30765=CARTESIAN_POINT('Ctrl Pts',(-0.197089662404178,0.00259797405121459,
0.00878884347189939));
#30766=CARTESIAN_POINT('',(-0.198291526612024,0.00259925634552079,0.00881316468156375));
#30767=CARTESIAN_POINT('',(-0.197089662528356,0.00259797789988061,0.00878883713767665));
#30768=CARTESIAN_POINT('Ctrl Pts',(-0.198291526612024,0.00259925634552079,
0.00881316468156375));
#30769=CARTESIAN_POINT('Ctrl Pts',(-0.198273132696056,0.00271922866138589,
0.00888590375084709));
#30770=CARTESIAN_POINT('Ctrl Pts',(-0.198257339690863,0.00282455834668754,
0.00894625110008983));
#30771=CARTESIAN_POINT('Ctrl Pts',(-0.19824335373048,0.00291985877639059,
0.00899902457795324));
#30772=CARTESIAN_POINT('Ctrl Pts',(-0.198236360719517,0.00296750920091354,
0.0090254114329924));
#30773=CARTESIAN_POINT('Ctrl Pts',(-0.198229820492752,0.00301268208812486,
0.00904985350188748));
#30774=CARTESIAN_POINT('Ctrl Pts',(-0.198224523869574,0.00304951773520309,
0.00906950500261461));
#30775=CARTESIAN_POINT('Ctrl Pts',(-0.198219227246395,0.00308635338228131,
0.00908915650334175));
#30776=CARTESIAN_POINT('Ctrl Pts',(-0.198215171776289,0.00311478604942531,
0.00910413877179396));
#30777=CARTESIAN_POINT('Ctrl Pts',(-0.198209198476182,0.00315790597635664,
0.00912643125667087));
#30778=CARTESIAN_POINT('Ctrl Pts',(-0.198203225176075,0.00320102590328796,
0.00914872374154777));
#30779=CARTESIAN_POINT('Ctrl Pts',(-0.198195338468025,0.00325894642302733,
0.00917810925876707));
#30780=CARTESIAN_POINT('Ctrl Pts',(-0.198188353589727,0.00331198230778945,
0.00920431265300255));
#30781=CARTESIAN_POINT('Ctrl Pts',(-0.198181368711429,0.00336501819255157,
0.00923051604723802));
#30782=CARTESIAN_POINT('Ctrl Pts',(-0.198175282616766,0.00341309769589153,
0.00925368486756316));
#30783=CARTESIAN_POINT('Ctrl Pts',(-0.198169482305615,0.00346012706315391,
0.00927591255722074));
#30784=CARTESIAN_POINT('Ctrl Pts',(-0.198157881683312,0.00355418579767866,
0.00932036793653589));
#30785=CARTESIAN_POINT('Ctrl Pts',(-0.198147424513911,0.00364404326995715,
0.00936104592055934));
#30786=CARTESIAN_POINT('Ctrl Pts',(-0.198137660544414,0.00373772805993553,
0.00940169259078848));
#30787=CARTESIAN_POINT('Ctrl Pts',(-0.198119913759321,0.00390800755892871,
0.00947557112159327));
#30788=CARTESIAN_POINT('Ctrl Pts',(-0.198104467740312,0.0040911383889277,
0.00954887570378074));
#30789=CARTESIAN_POINT('Ctrl Pts',(-0.19809309874562,0.0042779199997942,
0.00961661122033504));
#30790=CARTESIAN_POINT('Ctrl Pts',(-0.198091957697867,0.00429666631318535,
0.00962340948711916));
#30791=CARTESIAN_POINT('Ctrl Pts',(-0.198090857718422,0.00431544857027613,
0.00963015350494398));
#30792=CARTESIAN_POINT('Ctrl Pts',(-0.198089800603058,0.00433425688018677,
0.00963683962793629));
#30793=CARTESIAN_POINT('Ctrl Pts',(-0.198078210765531,0.0045404645122726,
0.00971014390655727));
#30794=CARTESIAN_POINT('Ctrl Pts',(-0.198071771836712,0.00474993416743466,
0.00977626207010369));
#30795=CARTESIAN_POINT('Ctrl Pts',(-0.198069559753659,0.00495091769207219,
0.00983262144189136));
#30796=CARTESIAN_POINT('Ctrl Pts',(-0.198067347670605,0.00515190121670971,
0.00988898081367903));
#30797=CARTESIAN_POINT('Ctrl Pts',(-0.19806934434283,0.0053441509600576,
0.00993640952736992));
#30798=CARTESIAN_POINT('Ctrl Pts',(-0.19807515731124,0.0055543837248035,
0.00998087296857176));
#30799=CARTESIAN_POINT('Ctrl Pts',(-0.198078063795445,0.00565950010717645,
0.0100031046891727));
#30800=CARTESIAN_POINT('Ctrl Pts',(-0.198081929169107,0.0057691566710522,
0.010024378634757));
#30801=CARTESIAN_POINT('Ctrl Pts',(-0.198086583120904,0.00587762248490804,
0.0100434450536445));
#30802=CARTESIAN_POINT('Ctrl Pts',(-0.198087489992435,0.00589875819128381,
0.0100471603462046));
#30803=CARTESIAN_POINT('Ctrl Pts',(-0.198088426645042,0.00591984801275532,
0.0100507949964277));
#30804=CARTESIAN_POINT('Ctrl Pts',(-0.198089410867419,0.00594119659128827,
0.0100543996135915));
#30805=CARTESIAN_POINT('',(-0.199090540183301,0.00260012944092227,0.00882936615427334));
#30806=CARTESIAN_POINT('Ctrl Pts',(-0.198888606651639,0.00593939180859995,
0.0100720065732061));
#30807=CARTESIAN_POINT('Ctrl Pts',(-0.198887676387017,0.00591893933289523,
0.0100685351665996));
#30808=CARTESIAN_POINT('Ctrl Pts',(-0.198882044030561,0.00579055403993556,
0.0100462494530026));
#30809=CARTESIAN_POINT('Ctrl Pts',(-0.198869890751112,0.00544134676562644,
0.00997834423696948));
#30810=CARTESIAN_POINT('Ctrl Pts',(-0.198865041548557,0.00495992103640058,
0.00985954411932006));
#30811=CARTESIAN_POINT('Ctrl Pts',(-0.19888434673602,0.0043304455028863,
0.00966125441771457));
#30812=CARTESIAN_POINT('Ctrl Pts',(-0.198925750261522,0.00382474303179102,
0.00945991595216248));
#30813=CARTESIAN_POINT('Ctrl Pts',(-0.198962251165325,0.00350936192060643,
0.00931660579371268));
#30814=CARTESIAN_POINT('Ctrl Pts',(-0.198986506970023,0.00331701212666396,
0.00922394949251914));
#30815=CARTESIAN_POINT('Ctrl Pts',(-0.199009982866199,0.00314426989599801,
0.00913607982520711));
#30816=CARTESIAN_POINT('Ctrl Pts',(-0.19902237458798,0.00305736235190651,
0.009090117421809));
#30817=CARTESIAN_POINT('Ctrl Pts',(-0.19904857160634,0.00287649479718902,
0.00899215805150388));
#30818=CARTESIAN_POINT('Ctrl Pts',(-0.19907222585195,0.00271920306422584,
0.00890168902253671));
#30819=CARTESIAN_POINT('Ctrl Pts',(-0.199090540183301,0.00260012944092227,
0.00882936615427334));
#30820=CARTESIAN_POINT('',(-0.200292328770423,0.00260137281375138,0.00885372168982735));
#30821=CARTESIAN_POINT('',(-0.199090540305781,0.00260013324515697,0.00882935992144404));
#30822=CARTESIAN_POINT('Ctrl Pts',(-0.200292328770423,0.00260137281375138,
0.00885372168982735));
#30823=CARTESIAN_POINT('Ctrl Pts',(-0.200273837896757,0.00272121175790609,
0.00892670462618666));
#30824=CARTESIAN_POINT('Ctrl Pts',(-0.200257961423412,0.00282643766557617,
0.00898725675305832));
#30825=CARTESIAN_POINT('Ctrl Pts',(-0.200243900974506,0.00292165061038557,
0.00904021017006671));
#30826=CARTESIAN_POINT('Ctrl Pts',(-0.200236870718853,0.00296925729406923,
0.00906668699607533));
#30827=CARTESIAN_POINT('Ctrl Pts',(-0.200230295497294,0.00301439072573244,
0.00909121268824908));
#30828=CARTESIAN_POINT('Ctrl Pts',(-0.200224970624474,0.00305119417903304,
0.00911093102925758));
#30829=CARTESIAN_POINT('Ctrl Pts',(-0.200219645751654,0.00308799763233363,
0.00913064937026609));
#30830=CARTESIAN_POINT('Ctrl Pts',(-0.200215568764996,0.0031164048833556,
0.00914568206453222));
#30831=CARTESIAN_POINT('Ctrl Pts',(-0.20020956272179,0.00315949117040272,
0.00916805152229006));
#30832=CARTESIAN_POINT('Ctrl Pts',(-0.200203556678583,0.00320257745744984,
0.00919042098004789));
#30833=CARTESIAN_POINT('Ctrl Pts',(-0.200195626022548,0.00326045695423104,
0.00921990933366753));
#30834=CARTESIAN_POINT('Ctrl Pts',(-0.200188601532831,0.00331345701852395,
0.00924620432155298));
#30835=CARTESIAN_POINT('Ctrl Pts',(-0.200181577043113,0.00336645708281686,
0.00927249930943843));
#30836=CARTESIAN_POINT('Ctrl Pts',(-0.200175455659094,0.00341450543872106,
0.00929574895779386));
#30837=CARTESIAN_POINT('Ctrl Pts',(-0.200169621352145,0.00346150318350308,
0.00931805309801738));
#30838=CARTESIAN_POINT('Ctrl Pts',(-0.200157952738249,0.00355549867306711,
0.00936266137846443));
#30839=CARTESIAN_POINT('Ctrl Pts',(-0.20014743274518,0.00364529078631978,
0.00940347505836594));
#30840=CARTESIAN_POINT('Ctrl Pts',(-0.200137604015595,0.00373893481032285,
0.00944426681906609));
#30841=CARTESIAN_POINT('Ctrl Pts',(-0.200120047004139,0.00390621067117079,
0.00951713294116265));
#30842=CARTESIAN_POINT('Ctrl Pts',(-0.200104706208719,0.00408597836688247,
0.00958947556607649));
#30843=CARTESIAN_POINT('Ctrl Pts',(-0.200093286933946,0.00426938216658885,
0.00965646105117785));
#30844=CARTESIAN_POINT('Ctrl Pts',(-0.200091920779482,0.00429132383316669,
0.00966447491556889));
#30845=CARTESIAN_POINT('Ctrl Pts',(-0.200090610752696,0.00431331641716091,
0.00967241458652526));
#30846=CARTESIAN_POINT('Ctrl Pts',(-0.200089359773607,0.00433534378299784,
0.00968027408652165));
#30847=CARTESIAN_POINT('Ctrl Pts',(-0.200077652236101,0.00454149128290405,
0.00975382878601519));
#30848=CARTESIAN_POINT('Ctrl Pts',(-0.200071114735433,0.00475081464251925,
0.00982013994437917));
#30849=CARTESIAN_POINT('Ctrl Pts',(-0.20006882183701,0.00495177345483577,
0.0098766928364664));
#30850=CARTESIAN_POINT('Ctrl Pts',(-0.200066528938587,0.00515273226715229,
0.00993324572855362));
#30851=CARTESIAN_POINT('Ctrl Pts',(-0.20006846267712,0.00534507943381997,
0.00998086237617104));
#30852=CARTESIAN_POINT('Ctrl Pts',(-0.200074226063807,0.00555533499112588,
0.0100254775673568));
#30853=CARTESIAN_POINT('Ctrl Pts',(-0.20007710775715,0.00566046276977883,
0.0100477851629496));
#30854=CARTESIAN_POINT('Ctrl Pts',(-0.200080951668549,0.0057701121703622,
0.0100691264095741));
#30855=CARTESIAN_POINT('Ctrl Pts',(-0.200085588250657,0.00587857122173911,
0.0100882522879767));
#30856=CARTESIAN_POINT('Ctrl Pts',(-0.200086414932592,0.00589790898743928,
0.0100916623468944));
#30857=CARTESIAN_POINT('Ctrl Pts',(-0.200087266677091,0.00591720835943309,
0.0100950045482874));
#30858=CARTESIAN_POINT('Ctrl Pts',(-0.200088157086456,0.00593670244816755,
0.0100983180218859));
#30859=CARTESIAN_POINT('',(-0.201091331877826,0.00260231956762303,0.0088700075790552));
#30860=CARTESIAN_POINT('Ctrl Pts',(-0.200887345683122,0.0059348980442802,
0.0101159223609127));
#30861=CARTESIAN_POINT('Ctrl Pts',(-0.200886506663953,0.00591628097381425,
0.0101127400212251));
#30862=CARTESIAN_POINT('Ctrl Pts',(-0.200880986324111,0.0057896653627417,
0.010090654716993));
#30863=CARTESIAN_POINT('Ctrl Pts',(-0.200868962037106,0.005442297041805,
0.0100228912331785));
#30864=CARTESIAN_POINT('Ctrl Pts',(-0.20086426816572,0.00496065222418959,
0.00990362400826062));
#30865=CARTESIAN_POINT('Ctrl Pts',(-0.200883867541184,0.00433161563399345,
0.00970476368487069));
#30866=CARTESIAN_POINT('Ctrl Pts',(-0.200925609896317,0.00382589679812178,
0.00950265618711336));
#30867=CARTESIAN_POINT('Ctrl Pts',(-0.200962333382757,0.00351075052547446,
0.00935887421941144));
#30868=CARTESIAN_POINT('Ctrl Pts',(-0.200986731782129,0.00331853051675235,
0.00926590227797969));
#30869=CARTESIAN_POINT('Ctrl Pts',(-0.201010339542551,0.00314592329813722,
0.00917773598410989));
#30870=CARTESIAN_POINT('Ctrl Pts',(-0.201022800394077,0.00305908023167697,
0.00913161420213365));
#30871=CARTESIAN_POINT('Ctrl Pts',(-0.201049140182371,0.00287837410448303,
0.0090333264982479));
#30872=CARTESIAN_POINT('Ctrl Pts',(-0.201072920671161,0.00272124883301824,
0.00894256141583152));
#30873=CARTESIAN_POINT('Ctrl Pts',(-0.201091331877826,0.00260231956762303,
0.0088700075790552));
#30874=CARTESIAN_POINT('',(-0.202293065733516,0.00260357610533656,0.00889442911865277));
#30875=CARTESIAN_POINT('',(-0.201091331999189,0.00260232334500957,0.00887000141752919));
#30876=CARTESIAN_POINT('Ctrl Pts',(-0.202293065733516,0.00260357610533656,
0.00889442911865277));
#30877=CARTESIAN_POINT('Ctrl Pts',(-0.202274475468373,0.00272326920892133,
0.00896764049982792));
#30878=CARTESIAN_POINT('Ctrl Pts',(-0.202258513370394,0.00282838010195822,
0.00902838492069327));
#30879=CARTESIAN_POINT('Ctrl Pts',(-0.202244376443369,0.00292349537576616,
0.00908150758113047));
#30880=CARTESIAN_POINT('Ctrl Pts',(-0.202237307948081,0.00297105322646132,
0.00910806903075321));
#30881=CARTESIAN_POINT('Ctrl Pts',(-0.202230696778204,0.00301614236175929,
0.00913267346161789));
#30882=CARTESIAN_POINT('Ctrl Pts',(-0.202225342855067,0.00305290982182173,
0.00915245482498696));
#30883=CARTESIAN_POINT('Ctrl Pts',(-0.20221998893193,0.00308967728188417,
0.00917223618835603));
#30884=CARTESIAN_POINT('Ctrl Pts',(-0.202215889781666,0.00311805638280766,
0.00918731651992855));
#30885=CARTESIAN_POINT('Ctrl Pts',(-0.202209850054849,0.00316110438387033,
0.00920975861098695));
#30886=CARTESIAN_POINT('Ctrl Pts',(-0.202203810328033,0.00320415238493301,
0.00923220070204534));
#30887=CARTESIAN_POINT('Ctrl Pts',(-0.202195834488617,0.00326198425819688,
0.00926178607004551));
#30888=CARTESIAN_POINT('Ctrl Pts',(-0.202188769218574,0.00331494264804402,
0.00928816764310139));
#30889=CARTESIAN_POINT('Ctrl Pts',(-0.202181703948532,0.00336790103789116,
0.00931454921615728));
#30890=CARTESIAN_POINT('Ctrl Pts',(-0.202175546173851,0.00341591316921346,
0.00933787544456852));
#30891=CARTESIAN_POINT('Ctrl Pts',(-0.202169676846241,0.0034628734948644,
0.00936025161595196));
#30892=CARTESIAN_POINT('Ctrl Pts',(-0.202157938191021,0.00355679414616629,
0.00940500395871885));
#30893=CARTESIAN_POINT('Ctrl Pts',(-0.202147353627051,0.00364650633906559,
0.00944594396933934));
#30894=CARTESIAN_POINT('Ctrl Pts',(-0.202137457493401,0.00374010383894624,
0.00948687578309684));
#30895=CARTESIAN_POINT('Ctrl Pts',(-0.202120088590578,0.0039043786898437,
0.00955871603107942));
#30896=CARTESIAN_POINT('Ctrl Pts',(-0.202104850677498,0.00408081733665042,
0.00963009264144663));
#30897=CARTESIAN_POINT('Ctrl Pts',(-0.202093384451066,0.0042608447204149,
0.00969630907557451));
#30898=CARTESIAN_POINT('Ctrl Pts',(-0.202091784646742,0.00428596271268767,
0.0097055478027391));
#30899=CARTESIAN_POINT('Ctrl Pts',(-0.202090258264773,0.00431114910199664,
0.00971468928320473));
#30900=CARTESIAN_POINT('Ctrl Pts',(-0.202088809761387,0.00433637909078407,
0.00972372430600667));
#30901=CARTESIAN_POINT('Ctrl Pts',(-0.202076979445947,0.00454243917237846,
0.00979751575916425));
#30902=CARTESIAN_POINT('Ctrl Pts',(-0.20207034194049,0.00475153493044841,
0.00986399247318988));
#30903=CARTESIAN_POINT('Ctrl Pts',(-0.202067969551709,0.00495244619644365,
0.00992073315628037));
#30904=CARTESIAN_POINT('Ctrl Pts',(-0.202065597162928,0.00515335746243889,
0.00997747383937085));
#30905=CARTESIAN_POINT('Ctrl Pts',(-0.202067472167892,0.00534583912516003,
0.0100252890958902));
#30906=CARTESIAN_POINT('Ctrl Pts',(-0.202073197894455,0.005556098712338,
0.0100700539580997));
#30907=CARTESIAN_POINT('Ctrl Pts',(-0.202076060757737,0.00566122850592697,
0.0100924363892045));
#30908=CARTESIAN_POINT('Ctrl Pts',(-0.202079891079458,0.00577084725715454,
0.0101138415381843));
#30909=CARTESIAN_POINT('Ctrl Pts',(-0.202084519326978,0.00587927387560881,
0.0101330242882825));
#30910=CARTESIAN_POINT('Ctrl Pts',(-0.202085271363521,0.0058968919435591,
0.010136141262689));
#30911=CARTESIAN_POINT('Ctrl Pts',(-0.202086044354192,0.0059144780827782,
0.0101392016200004));
#30912=CARTESIAN_POINT('Ctrl Pts',(-0.202086848594906,0.00593220842806255,
0.0101422352280257));
#30913=CARTESIAN_POINT('',(-0.203091791305043,0.00260433418259679,0.00891063271010805));
#30914=CARTESIAN_POINT('Ctrl Pts',(-0.202885099445385,0.00593040690138148,
0.0101598141695237));
#30915=CARTESIAN_POINT('Ctrl Pts',(-0.202884354971372,0.00591368430258583,
0.0101569360655661));
#30916=CARTESIAN_POINT('Ctrl Pts',(-0.202878992896662,0.00578947217370395,
0.0101351728763029));
#30917=CARTESIAN_POINT('Ctrl Pts',(-0.202867259104593,0.0054454906008289,
0.0100679541944753));
#30918=CARTESIAN_POINT('Ctrl Pts',(-0.202863123060488,0.004959530471194,
0.00994714447823416));
#30919=CARTESIAN_POINT('Ctrl Pts',(-0.202883406117703,0.00433659227554887,
0.00974971310348173));
#30920=CARTESIAN_POINT('Ctrl Pts',(-0.202926463640028,0.00382383543467921,
0.00954412528623439));
#30921=CARTESIAN_POINT('Ctrl Pts',(-0.202963209822097,0.003510675044003,
0.00940051603960522));
#30922=CARTESIAN_POINT('Ctrl Pts',(-0.202987598667131,0.00331891162837778,
0.00930736298217058));
#30923=CARTESIAN_POINT('Ctrl Pts',(-0.203011094368678,0.0031470861154104,
0.00921921390736344));
#30924=CARTESIAN_POINT('Ctrl Pts',(-0.203023587987513,0.00305986178150982,
0.00917269162038482));
#30925=CARTESIAN_POINT('Ctrl Pts',(-0.203049839751636,0.00287944809228144,
0.00907412081376304));
#30926=CARTESIAN_POINT('Ctrl Pts',(-0.2030734973985,0.00272278133299953,
0.00898321135849634));
#30927=CARTESIAN_POINT('Ctrl Pts',(-0.203091791305043,0.00260433418259679,
0.00891063271010805));
#30928=CARTESIAN_POINT('',(-0.204293510165871,0.00260574519043331,0.00893520746292813));
#30929=CARTESIAN_POINT('',(-0.203091791426825,0.00260433798081893,0.00891062654167635));
#30930=CARTESIAN_POINT('Ctrl Pts',(-0.204293510165871,0.00260574519043331,
0.00893520746292813));
#30931=CARTESIAN_POINT('Ctrl Pts',(-0.204275076567995,0.00272501382324815,
0.00900847502531422));
#30932=CARTESIAN_POINT('Ctrl Pts',(-0.204259227819518,0.00282988504055417,
0.0090693498218917));
#30933=CARTESIAN_POINT('Ctrl Pts',(-0.20424517062167,0.00292489404478681,
0.00912264277868882));
#30934=CARTESIAN_POINT('Ctrl Pts',(-0.20423814199043,0.00297239876531212,
0.00914928937959851));
#30935=CARTESIAN_POINT('Ctrl Pts',(-0.204231562274048,0.00301746803417767,
0.00917398932116904));
#30936=CARTESIAN_POINT('Ctrl Pts',(-0.204226221712992,0.00305430402977027,
0.00919389171338426));
#30937=CARTESIAN_POINT('Ctrl Pts',(-0.204220881151935,0.00309114002536287,
0.00921379410559949));
#30938=CARTESIAN_POINT('Ctrl Pts',(-0.204216777274443,0.00311967596045992,
0.00922902065933212));
#30939=CARTESIAN_POINT('Ctrl Pts',(-0.204210753464681,0.00316274908232262,
0.00925156788917228));
#30940=CARTESIAN_POINT('Ctrl Pts',(-0.20420472965492,0.00320582220418532,
0.00927411511901243));
#30941=CARTESIAN_POINT('Ctrl Pts',(-0.204196790365541,0.00326354743608214,
0.00930376547534614));
#30942=CARTESIAN_POINT('Ctrl Pts',(-0.204189744354715,0.00331644916448935,
0.00933022524743304));
#30943=CARTESIAN_POINT('Ctrl Pts',(-0.204182698343888,0.00336935089289657,
0.00935668501951994));
#30944=CARTESIAN_POINT('Ctrl Pts',(-0.204176542556964,0.00341735669267945,
0.00938010148299971));
#30945=CARTESIAN_POINT('Ctrl Pts',(-0.20417067241306,0.00346426236205979,
0.00940254036039787));
#30946=CARTESIAN_POINT('Ctrl Pts',(-0.204158932125252,0.0035580737008205,
0.00944741811519419));
#30947=CARTESIAN_POINT('Ctrl Pts',(-0.204148334510898,0.00364747781089567,
0.00948838331382297));
#30948=CARTESIAN_POINT('Ctrl Pts',(-0.20413834003469,0.00374131254045276,
0.00952957637488636));
#30949=CARTESIAN_POINT('Ctrl Pts',(-0.204121212928019,0.00390211310558426,
0.00960016716285746));
#30950=CARTESIAN_POINT('Ctrl Pts',(-0.20410586914575,0.00407615059995422,
0.00967093159324034));
#30951=CARTESIAN_POINT('Ctrl Pts',(-0.204094147762405,0.00425230443228834,
0.00973617036461655));
#30952=CARTESIAN_POINT('Ctrl Pts',(-0.204092189183428,0.00428173877315499,
0.00974707140610378));
#30953=CARTESIAN_POINT('Ctrl Pts',(-0.20409033174393,0.00431122959651332,
0.0097578240646924));
#30954=CARTESIAN_POINT('Ctrl Pts',(-0.204088584023885,0.00434072179096112,
0.0097684095940632));
#30955=CARTESIAN_POINT('Ctrl Pts',(-0.204076376834576,0.00454671405039965,
0.0098423456694646));
#30956=CARTESIAN_POINT('Ctrl Pts',(-0.204069514965021,0.00475286180502225,
0.0099080404173306));
#30957=CARTESIAN_POINT('Ctrl Pts',(-0.204066816106438,0.00495305084389507,
0.00996477003023813));
#30958=CARTESIAN_POINT('Ctrl Pts',(-0.204064117247854,0.0051532398827679,
0.0100214996431457));
#30959=CARTESIAN_POINT('Ctrl Pts',(-0.204065567196888,0.005347245104113,
0.01006991838009));
#30960=CARTESIAN_POINT('Ctrl Pts',(-0.204071292044941,0.00555973157676272,
0.0101152347804172));
#30961=CARTESIAN_POINT('Ctrl Pts',(-0.204074496107032,0.00567865523126791,
0.0101405972981752));
#30962=CARTESIAN_POINT('Ctrl Pts',(-0.204079049119957,0.00580343197303493,
0.0101647293003646));
#30963=CARTESIAN_POINT('Ctrl Pts',(-0.204084593180221,0.00592771653709633,
0.0101861316274437));
#30964=CARTESIAN_POINT('',(-0.205092331912265,0.00260645114791581,0.00895141913306061));
#30965=CARTESIAN_POINT('Ctrl Pts',(-0.204883316991064,0.00592592657070326,
0.0102036471645642));
#30966=CARTESIAN_POINT('Ctrl Pts',(-0.204882671137622,0.00591144529308884,
0.0102011599238186));
#30967=CARTESIAN_POINT('Ctrl Pts',(-0.20487717178741,0.00578506672453634,
0.0101791477099926));
#30968=CARTESIAN_POINT('Ctrl Pts',(-0.204866209701125,0.00545213555483161,
0.0101133657534363));
#30969=CARTESIAN_POINT('Ctrl Pts',(-0.204861852683361,0.00496215483740597,
0.00999260159629974));
#30970=CARTESIAN_POINT('Ctrl Pts',(-0.204880095936079,0.00442886261065933,
0.00982107008356725));
#30971=CARTESIAN_POINT('Ctrl Pts',(-0.204907085968845,0.00405046827475919,
0.00967788144453791));
#30972=CARTESIAN_POINT('Ctrl Pts',(-0.204937958692689,0.00372990950313333,
0.00954347459787447));
#30973=CARTESIAN_POINT('Ctrl Pts',(-0.204963618489919,0.00351270551424823,
0.00944317167265714));
#30974=CARTESIAN_POINT('Ctrl Pts',(-0.20498815842505,0.00332022837241253,
0.00934936436806583));
#30975=CARTESIAN_POINT('Ctrl Pts',(-0.205011645825832,0.00314877731821974,
0.00926103688660394));
#30976=CARTESIAN_POINT('Ctrl Pts',(-0.205024182885467,0.00306131323278087,
0.00921420176338373));
#30977=CARTESIAN_POINT('Ctrl Pts',(-0.205050437575135,0.00288103174617778,
0.00911528740541476));
#30978=CARTESIAN_POINT('Ctrl Pts',(-0.205074070416774,0.00272461878566508,
0.00902413649647073));
#30979=CARTESIAN_POINT('Ctrl Pts',(-0.205092331912265,0.00260645114791581,
0.00895141913306061));
#30980=CARTESIAN_POINT('',(-0.206293999435804,0.00260759218872069,0.00897588362098812));
#30981=CARTESIAN_POINT('',(-0.20509233202994,0.00260645482550656,0.0089514131859722));
#30982=CARTESIAN_POINT('Ctrl Pts',(-0.206293999435804,0.00260759218872069,
0.00897588362098812));
#30983=CARTESIAN_POINT('Ctrl Pts',(-0.206275606236776,0.00272657234509535,
0.00904928873984808));
#30984=CARTESIAN_POINT('Ctrl Pts',(-0.206251865963918,0.00288355267308425,
0.00914095396549715));
#30985=CARTESIAN_POINT('Ctrl Pts',(-0.206225558203887,0.00306373816500964,
0.00924000226939381));
#30986=CARTESIAN_POINT('Ctrl Pts',(-0.206213206763392,0.00314955254584123,
0.00928606722127801));
#30987=CARTESIAN_POINT('Ctrl Pts',(-0.206189409028581,0.0033223041095643,
0.00937526677216162));
#30988=CARTESIAN_POINT('Ctrl Pts',(-0.206164656195616,0.00351506923364879,
0.00946938213392435));
#30989=CARTESIAN_POINT('Ctrl Pts',(-0.206138728171142,0.00373241945612685,
0.00956991384257538));
#30990=CARTESIAN_POINT('Ctrl Pts',(-0.206107559899463,0.00405172320144206,
0.00970403637599294));
#30991=CARTESIAN_POINT('Ctrl Pts',(-0.206079921416922,0.00443029769141955,
0.00984754120837745));
#30992=CARTESIAN_POINT('Ctrl Pts',(-0.206061315628273,0.00496107403636117,
0.010018644986773));
#30993=CARTESIAN_POINT('Ctrl Pts',(-0.206065539578611,0.00545325447955815,
0.0101402646231475));
#30994=CARTESIAN_POINT('Ctrl Pts',(-0.206076538113247,0.00578510480717584,
0.0102059130522982));
#30995=CARTESIAN_POINT('Ctrl Pts',(-0.20608201684332,0.00591016240860172,
0.0102277486059419));
#30996=CARTESIAN_POINT('Ctrl Pts',(-0.206082602390132,0.00592322960732983,
0.0102300014544386));
#30997=CARTESIAN_POINT('',(-0.207092852170764,0.00260851097558208,0.00899226563559695));
#30998=CARTESIAN_POINT('Ctrl Pts',(-0.206881571004172,0.00592143254235674,
0.0102475607510614));
#30999=CARTESIAN_POINT('Ctrl Pts',(-0.206881020496666,0.00590893384282267,
0.0102453998143091));
#31000=CARTESIAN_POINT('Ctrl Pts',(-0.206875680990742,0.00578499503296741,
0.0102237098597449));
#31001=CARTESIAN_POINT('Ctrl Pts',(-0.206864923140502,0.00545427255237323,
0.0101582379308979));
#31002=CARTESIAN_POINT('Ctrl Pts',(-0.206860949893193,0.0049619143385102,
0.010036492327419));
#31003=CARTESIAN_POINT('Ctrl Pts',(-0.206879692666681,0.00442978956942307,
0.00986470087572262));
#31004=CARTESIAN_POINT('Ctrl Pts',(-0.206907292633342,0.00405093552770489,
0.00972082871068698));
#31005=CARTESIAN_POINT('Ctrl Pts',(-0.206938369196101,0.00373106068533,
0.00958619552651098));
#31006=CARTESIAN_POINT('Ctrl Pts',(-0.206964134873792,0.00351390912494474,
0.00948554071057212));
#31007=CARTESIAN_POINT('Ctrl Pts',(-0.206988721782151,0.00332157558445463,
0.00939143426474644));
#31008=CARTESIAN_POINT('Ctrl Pts',(-0.207012209264182,0.0031503451607018,
0.00930287133695935));
#31009=CARTESIAN_POINT('Ctrl Pts',(-0.207024781376472,0.00306268383339939,
0.0092557414932042));
#31010=CARTESIAN_POINT('Ctrl Pts',(-0.207051031204484,0.00288252984294508,
0.00915648754524844));
#31011=CARTESIAN_POINT('Ctrl Pts',(-0.207074629977899,0.00272638846036655,
0.00906510989893176));
#31012=CARTESIAN_POINT('Ctrl Pts',(-0.207092852170764,0.00260851097558208,
0.00899226563559695));
#31013=CARTESIAN_POINT('',(-0.208294495555528,0.002609557221425,0.00901672737671743));
#31014=CARTESIAN_POINT('',(-0.207092852286225,0.00260851459105031,0.00899225981344203));
#31015=CARTESIAN_POINT('Ctrl Pts',(-0.208294495555528,0.002609557221425,
0.00901672737671743));
#31016=CARTESIAN_POINT('Ctrl Pts',(-0.208276153739984,0.00272818271907759,
0.00909022007273419));
#31017=CARTESIAN_POINT('Ctrl Pts',(-0.208252462664079,0.00288480997457173,
0.00918206687811871));
#31018=CARTESIAN_POINT('Ctrl Pts',(-0.208226174631601,0.0030647907813057,
0.00928141626672825));
#31019=CARTESIAN_POINT('Ctrl Pts',(-0.208213795276203,0.00315076692511177,
0.00932775588295479));
#31020=CARTESIAN_POINT('Ctrl Pts',(-0.208190006020789,0.00332326101084848,
0.00941718226047124));
#31021=CARTESIAN_POINT('Ctrl Pts',(-0.208165206295545,0.00351592866849304,
0.00951162039509459));
#31022=CARTESIAN_POINT('Ctrl Pts',(-0.208139241772671,0.00373263243560695,
0.00961227396471289));
#31023=CARTESIAN_POINT('Ctrl Pts',(-0.20810762277873,0.00405359805798186,
0.00974757364736688));
#31024=CARTESIAN_POINT('Ctrl Pts',(-0.208079658202872,0.00442984491645365,
0.00989065971484939));
#31025=CARTESIAN_POINT('Ctrl Pts',(-0.2080603918466,0.00496098587762989,
0.0100626318644918));
#31026=CARTESIAN_POINT('Ctrl Pts',(-0.208064266452075,0.00545499835628659,
0.0101850488681411));
#31027=CARTESIAN_POINT('Ctrl Pts',(-0.208075055741243,0.00578480551874336,
0.0102504392329819));
#31028=CARTESIAN_POINT('Ctrl Pts',(-0.208080378153632,0.00590756155050767,
0.0102719761801877));
#31029=CARTESIAN_POINT('Ctrl Pts',(-0.208080872472194,0.00591873554374485,
0.0102739153516223));
#31030=CARTESIAN_POINT('',(-0.2090933136672,0.00261035295544765,0.00903306981791057));
#31031=CARTESIAN_POINT('Ctrl Pts',(-0.208879854976475,0.00591693841052602,
0.0102914751265115));
#31032=CARTESIAN_POINT('Ctrl Pts',(-0.208879403882135,0.00590656011569423,
0.0102896689662938));
#31033=CARTESIAN_POINT('Ctrl Pts',(-0.208874225719035,0.00578512936524486,
0.0102683205164887));
#31034=CARTESIAN_POINT('Ctrl Pts',(-0.208863665925877,0.00545665484873855,
0.0102031715204708));
#31035=CARTESIAN_POINT('Ctrl Pts',(-0.208860006423808,0.0049627509677495,
0.0100807435638028));
#31036=CARTESIAN_POINT('Ctrl Pts',(-0.208879357400325,0.00443027031107117,
0.00990816157715126));
#31037=CARTESIAN_POINT('Ctrl Pts',(-0.20890726143644,0.00405355877387217,
0.00976467967278848));
#31038=CARTESIAN_POINT('Ctrl Pts',(-0.208938745865106,0.00373216391169831,
0.00962896700904035));
#31039=CARTESIAN_POINT('Ctrl Pts',(-0.208964558210369,0.00351545759703801,
0.00952812730521938));
#31040=CARTESIAN_POINT('Ctrl Pts',(-0.20898919858518,0.00332310641781344,
0.00943366189332718));
#31041=CARTESIAN_POINT('Ctrl Pts',(-0.209012687715841,0.00315201860638895,
0.00934483181569398));
#31042=CARTESIAN_POINT('Ctrl Pts',(-0.209025296557779,0.00306411948254137,
0.00929738914424859));
#31043=CARTESIAN_POINT('Ctrl Pts',(-0.20905154854399,0.00288399129561906,
0.00919774726681492));
#31044=CARTESIAN_POINT('Ctrl Pts',(-0.209075122591561,0.00272802036343885,
0.00910608875383453));
#31045=CARTESIAN_POINT('Ctrl Pts',(-0.2090933136672,0.00261035295544765,
0.00903306981791057));
#31046=CARTESIAN_POINT('',(-0.210295195412647,0.00261161233680568,0.00905772513090701));
#31047=CARTESIAN_POINT('',(-0.209093313783645,0.00261035660874823,0.00903306395929884));
#31048=CARTESIAN_POINT('Ctrl Pts',(-0.210295195412647,0.00261161233680569,
0.00905772513090701));
#31049=CARTESIAN_POINT('Ctrl Pts',(-0.210276894963234,0.00272994295497824,
0.00913133389119312));
#31050=CARTESIAN_POINT('Ctrl Pts',(-0.210253240828118,0.00288629398964245,
0.00922339455195382));
#31051=CARTESIAN_POINT('Ctrl Pts',(-0.210226962421796,0.00306614095590343,
0.00932306899945819));
#31052=CARTESIAN_POINT('Ctrl Pts',(-0.210214549298879,0.00315232223911781,
0.00936969988198298));
#31053=CARTESIAN_POINT('Ctrl Pts',(-0.210190769979594,0.00332456621842443,
0.00945934060833127));
#31054=CARTESIAN_POINT('Ctrl Pts',(-0.210165926230228,0.00351714624291661,
0.00955409089556758));
#31055=CARTESIAN_POINT('Ctrl Pts',(-0.21013992137214,0.00373332555747361,
0.00965489747215478));
#31056=CARTESIAN_POINT('Ctrl Pts',(-0.210107902642912,0.0040555984786723,
0.00979120813717689));
#31057=CARTESIAN_POINT('Ctrl Pts',(-0.210079607338285,0.00442978955791621,
0.00993395826629711));
#31058=CARTESIAN_POINT('Ctrl Pts',(-0.210059670420687,0.00496117514435055,
0.0101067070575915));
#31059=CARTESIAN_POINT('Ctrl Pts',(-0.210063175312016,0.00545645643098748,
0.0102297840556843));
#31060=CARTESIAN_POINT('Ctrl Pts',(-0.210073732641992,0.00578430958237604,
0.010294942762644));
#31061=CARTESIAN_POINT('Ctrl Pts',(-0.210078893244153,0.00590490128356823,
0.010316200616972));
#31062=CARTESIAN_POINT('Ctrl Pts',(-0.21007929998055,0.00591424122749678,
0.0103178320466886));
#31063=CARTESIAN_POINT('',(-0.21109423145639,0.00261222360480081,0.00907399364715958));
#31064=CARTESIAN_POINT('Ctrl Pts',(-0.210878462469796,0.00591244389125894,
0.0103353945802353));
#31065=CARTESIAN_POINT('Ctrl Pts',(-0.210878081781242,0.00590353255855026,
0.0103338336933755));
#31066=CARTESIAN_POINT('Ctrl Pts',(-0.210873054175543,0.00578382770812169,
0.010312682318795));
#31067=CARTESIAN_POINT('Ctrl Pts',(-0.21086273938801,0.00545688672168629,
0.0102476370857249));
#31068=CARTESIAN_POINT('Ctrl Pts',(-0.21085947521624,0.00496214926258382,
0.0101245977556503));
#31069=CARTESIAN_POINT('Ctrl Pts',(-0.21087951803606,0.00442942772142485,
0.00995120290508484));
#31070=CARTESIAN_POINT('Ctrl Pts',(-0.210907778127693,0.00405467894669112,
0.00980797983942088));
#31071=CARTESIAN_POINT('Ctrl Pts',(-0.210939660748439,0.00373214570960748,
0.00967129247182057));
#31072=CARTESIAN_POINT('Ctrl Pts',(-0.210965515951445,0.00351605213693032,
0.00957032405479985));
#31073=CARTESIAN_POINT('Ctrl Pts',(-0.210990200367711,0.00332387153922504,
0.00947557360729596));
#31074=CARTESIAN_POINT('Ctrl Pts',(-0.21101367907488,0.00315310641654562,
0.0093865593121067));
#31075=CARTESIAN_POINT('Ctrl Pts',(-0.211026321387228,0.00306503577488379,
0.00933883439822843));
#31076=CARTESIAN_POINT('Ctrl Pts',(-0.21105255883218,0.00288513131503311,
0.00923890762798111));
#31077=CARTESIAN_POINT('Ctrl Pts',(-0.211076088510623,0.00272952577556201,
0.00914708390503086));
#31078=CARTESIAN_POINT('Ctrl Pts',(-0.21109423145639,0.00261222360480081,
0.00907399364715958));
#31079=CARTESIAN_POINT('',(-0.212296004165384,0.00261384219706213,0.0090989278724998));
#31080=CARTESIAN_POINT('',(-0.211094231575152,0.00261222733769334,0.00907398768525308));
#31081=CARTESIAN_POINT('Ctrl Pts',(-0.212296004165384,0.00261384219706213,
0.0090989278724998));
#31082=CARTESIAN_POINT('Ctrl Pts',(-0.212277735923486,0.00273194228337272,
0.00917268275309667));
#31083=CARTESIAN_POINT('Ctrl Pts',(-0.212261985492411,0.00283608798183092,
0.00923414686528063));
#31084=CARTESIAN_POINT('Ctrl Pts',(-0.212247974568846,0.00293067459298826,
0.00928807357720397));
#31085=CARTESIAN_POINT('Ctrl Pts',(-0.212240969072873,0.00297796812938874,
0.00931503706476419));
#31086=CARTESIAN_POINT('Ctrl Pts',(-0.212234399475194,0.00302290207516733,
0.00934006570537844));
#31087=CARTESIAN_POINT('Ctrl Pts',(-0.212229041039002,0.00305981228032552,
0.00936033052343684));
#31088=CARTESIAN_POINT('Ctrl Pts',(-0.212223682602811,0.00309672248548371,
0.00938059534149524));
#31089=CARTESIAN_POINT('Ctrl Pts',(-0.212219532847886,0.00312554135293767,
0.00939621760162779));
#31090=CARTESIAN_POINT('Ctrl Pts',(-0.212213495110603,0.00316856811982108,
0.00941909623229276));
#31091=CARTESIAN_POINT('Ctrl Pts',(-0.212207457373319,0.0032115948867045,
0.00944197486295772));
#31092=CARTESIAN_POINT('Ctrl Pts',(-0.212199536090053,0.00326894492966083,
0.00947189457532482));
#31093=CARTESIAN_POINT('Ctrl Pts',(-0.212192466189656,0.00332170276326728,
0.0094986935446409));
#31094=CARTESIAN_POINT('Ctrl Pts',(-0.212185396289258,0.00337446059687373,
0.00952549251395698));
#31095=CARTESIAN_POINT('Ctrl Pts',(-0.212179174818905,0.00342255601183432,
0.00954931216789045));
#31096=CARTESIAN_POINT('Ctrl Pts',(-0.212173291629739,0.00346902581832251,
0.00957188405703276));
#31097=CARTESIAN_POINT('Ctrl Pts',(-0.212161525251405,0.0035619654312989,
0.00961702783531737));
#31098=CARTESIAN_POINT('Ctrl Pts',(-0.212151109901664,0.00364834124124333,
0.00965728405441869));
#31099=CARTESIAN_POINT('Ctrl Pts',(-0.212140505592993,0.00374529742170372,
0.00970048237318596));
#31100=CARTESIAN_POINT('Ctrl Pts',(-0.212129901284321,0.00384225360216411,
0.00974368069195322));
#31101=CARTESIAN_POINT('Ctrl Pts',(-0.212119116554359,0.00394997858201931,
0.00978941616389929));
#31102=CARTESIAN_POINT('Ctrl Pts',(-0.212110151027643,0.00405046555875387,
0.00982991641873049));
#31103=CARTESIAN_POINT('Ctrl Pts',(-0.212105013763328,0.00410804479263682,
0.00985312314383084));
#31104=CARTESIAN_POINT('Ctrl Pts',(-0.212100471309807,0.00416321195017911,
0.00987469792720441));
#31105=CARTESIAN_POINT('Ctrl Pts',(-0.212096372540523,0.00421814681610697,
0.00989559901519815));
#31106=CARTESIAN_POINT('Ctrl Pts',(-0.212093318159167,0.00425908398983895,
0.00991117439625962));
#31107=CARTESIAN_POINT('Ctrl Pts',(-0.212090510162419,0.00429989388723458,
0.00992637191619471));
#31108=CARTESIAN_POINT('Ctrl Pts',(-0.212087886011393,0.00434150293396735,
0.00994152638604518));
#31109=CARTESIAN_POINT('Ctrl Pts',(-0.212075594849675,0.00453639397381732,
0.0100125078340582));
#31110=CARTESIAN_POINT('Ctrl Pts',(-0.212067360748948,0.00474904926940472,
0.0100818793281687));
#31111=CARTESIAN_POINT('Ctrl Pts',(-0.212063881613349,0.00495460319093813,
0.0101409226567405));
#31112=CARTESIAN_POINT('Ctrl Pts',(-0.21206040247775,0.00516015711247153,
0.0101999659853123));
#31113=CARTESIAN_POINT('Ctrl Pts',(-0.212061656540207,0.00535834953744217,
0.0102496659483022));
#31114=CARTESIAN_POINT('Ctrl Pts',(-0.212066560444648,0.00556611709299906,
0.0102944330158904));
#31115=CARTESIAN_POINT('Ctrl Pts',(-0.212069012396869,0.00567000087077749,
0.0103168165496846));
#31116=CARTESIAN_POINT('Ctrl Pts',(-0.212072378553916,0.00577628596176437,
0.0103378898590875));
#31117=CARTESIAN_POINT('Ctrl Pts',(-0.212076975297797,0.00588702112727913,
0.0103577274103283));
#31118=CARTESIAN_POINT('Ctrl Pts',(-0.21207728891332,0.00589457609831334,
0.0103590808387926));
#31119=CARTESIAN_POINT('Ctrl Pts',(-0.212077608279109,0.00590215187063596,
0.0103604284012948));
#31120=CARTESIAN_POINT('Ctrl Pts',(-0.212077933064703,0.00590974366334612,
0.0103617691152544));
#31121=CARTESIAN_POINT('',(-0.213095020058853,0.0026146493650334,0.00911535572166111));
#31122=CARTESIAN_POINT('Ctrl Pts',(-0.212877121847906,0.00590794924227077,
0.0103793151952651));
#31123=CARTESIAN_POINT('Ctrl Pts',(-0.212876817456775,0.00590068523348327,
0.0103780347325747));
#31124=CARTESIAN_POINT('Ctrl Pts',(-0.212871947615568,0.00578279537987255,
0.0103571043018428));
#31125=CARTESIAN_POINT('Ctrl Pts',(-0.212861880781934,0.00545750062331711,
0.0102921968347704));
#31126=CARTESIAN_POINT('Ctrl Pts',(-0.212858979669491,0.00496282289052902,
0.010168825226635));
#31127=CARTESIAN_POINT('Ctrl Pts',(-0.212879715250166,0.00442960172647075,
0.00999463393014085));
#31128=CARTESIAN_POINT('Ctrl Pts',(-0.212908265302508,0.00405688428523701,
0.00985175853701584));
#31129=CARTESIAN_POINT('Ctrl Pts',(-0.212940510942374,0.00373315259093314,
0.00971412549795729));
#31130=CARTESIAN_POINT('Ctrl Pts',(-0.212966389766975,0.00351758829891117,
0.00961302767103597));
#31131=CARTESIAN_POINT('Ctrl Pts',(-0.21299110390974,0.00332551002962964,
0.00951799089112226));
#31132=CARTESIAN_POINT('Ctrl Pts',(-0.213014561259845,0.00315500318886664,
0.00942878763037121));
#31133=CARTESIAN_POINT('Ctrl Pts',(-0.213027232407688,0.00306672600484153,
0.00938077473444571));
#31134=CARTESIAN_POINT('Ctrl Pts',(-0.213053447606084,0.00288696467213194,
0.0092805471432282));
#31135=CARTESIAN_POINT('Ctrl Pts',(-0.213076928211355,0.00273164707469549,
0.00918853718936164));
#31136=CARTESIAN_POINT('Ctrl Pts',(-0.213095020058853,0.0026146493650334,
0.00911535572166111));
#31137=CARTESIAN_POINT('',(-0.214296906974989,0.00261538462477282,0.00913979240089912));
#31138=CARTESIAN_POINT('',(-0.213095020167502,0.00261465278607558,0.00911535027878834));
#31139=CARTESIAN_POINT('Ctrl Pts',(-0.214296906974989,0.00261538462477282,
0.00913979240089912));
#31140=CARTESIAN_POINT('Ctrl Pts',(-0.214278683661499,0.0027331943743573,
0.00921366437608414));
#31141=CARTESIAN_POINT('Ctrl Pts',(-0.214262960945703,0.00283716004480444,
0.00927527307807957));
#31142=CARTESIAN_POINT('Ctrl Pts',(-0.214248964299891,0.00293164466650735,
0.00932935789200659));
#31143=CARTESIAN_POINT('Ctrl Pts',(-0.214241965944719,0.00297888719516994,
0.00935640042364937));
#31144=CARTESIAN_POINT('Ctrl Pts',(-0.214235400126686,0.00302378966695629,
0.00938151165815695));
#31145=CARTESIAN_POINT('Ctrl Pts',(-0.214230038337221,0.00306071935690244,
0.00940186736996042));
#31146=CARTESIAN_POINT('Ctrl Pts',(-0.214224676547756,0.00309764904684859,
0.00942222308176389));
#31147=CARTESIAN_POINT('Ctrl Pts',(-0.214220516304366,0.00312653814109853,
0.00943794444374524));
#31148=CARTESIAN_POINT('Ctrl Pts',(-0.214214476041821,0.00316955964443814,
0.00946090868045039));
#31149=CARTESIAN_POINT('Ctrl Pts',(-0.214208435779277,0.00321258114777775,
0.00948387291715554));
#31150=CARTESIAN_POINT('Ctrl Pts',(-0.214200519934111,0.00326985069535863,
0.00951386507025742));
#31151=CARTESIAN_POINT('Ctrl Pts',(-0.21419344857914,0.00332255570074024,
0.00954073938679254));
#31152=CARTESIAN_POINT('Ctrl Pts',(-0.214186377224168,0.00337526070612183,
0.00956761370332765));
#31153=CARTESIAN_POINT('Ctrl Pts',(-0.214180147412035,0.00342333094238063,
0.00959151115435043));
#31154=CARTESIAN_POINT('Ctrl Pts',(-0.214174255823015,0.00346976009689579,
0.00961414826400449));
#31155=CARTESIAN_POINT('Ctrl Pts',(-0.214162472644975,0.00356261840592612,
0.00965942248331261));
#31156=CARTESIAN_POINT('Ctrl Pts',(-0.214152040175484,0.00364884865052032,
0.00969976288009719));
#31157=CARTESIAN_POINT('Ctrl Pts',(-0.214141374430434,0.0037458485751099,
0.00974313915376534));
#31158=CARTESIAN_POINT('Ctrl Pts',(-0.214130708685383,0.00384284849969948,
0.0097865154274335));
#31159=CARTESIAN_POINT('Ctrl Pts',(-0.214119818429043,0.00395081202920119,
0.00983251236920754));
#31160=CARTESIAN_POINT('Ctrl Pts',(-0.214110754468016,0.00405125305607647,
0.00987313187882039));
#31161=CARTESIAN_POINT('Ctrl Pts',(-0.21410584648218,0.00410564022033151,
0.00989512667526963));
#31162=CARTESIAN_POINT('Ctrl Pts',(-0.214101471672964,0.00415778941429641,
0.00991562349899335));
#31163=CARTESIAN_POINT('Ctrl Pts',(-0.214097498720132,0.00420960497907179,
0.00993546753367953));
#31164=CARTESIAN_POINT('Ctrl Pts',(-0.214094134510461,0.00425348126742845,
0.00995227102876493));
#31165=CARTESIAN_POINT('Ctrl Pts',(-0.214091058445176,0.00429711967373464,
0.00996860379932433));
#31166=CARTESIAN_POINT('Ctrl Pts',(-0.21408819079082,0.00434170808743411,
0.00998489955126376));
#31167=CARTESIAN_POINT('Ctrl Pts',(-0.214075682387318,0.00453619800875275,
0.0100559798891715));
#31168=CARTESIAN_POINT('Ctrl Pts',(-0.214067163840417,0.00474900888568837,
0.0101256532944664));
#31169=CARTESIAN_POINT('Ctrl Pts',(-0.214063467913489,0.00495457669098817,
0.0101849000646645));
#31170=CARTESIAN_POINT('Ctrl Pts',(-0.214059771986562,0.00516014449628797,
0.0102441468348626));
#31171=CARTESIAN_POINT('Ctrl Pts',(-0.214060876327417,0.00535820131743478,
0.0102939778670901));
#31172=CARTESIAN_POINT('Ctrl Pts',(-0.214065643033967,0.00556593470413897,
0.010338888699365));
#31173=CARTESIAN_POINT('Ctrl Pts',(-0.214068026387243,0.00566980139749106,
0.0103613441155025));
#31174=CARTESIAN_POINT('Ctrl Pts',(-0.214071327128676,0.00577609514550041,
0.0103824901485091));
#31175=CARTESIAN_POINT('Ctrl Pts',(-0.214075858954125,0.00588681471194534,
0.0104023917424961));
#31176=CARTESIAN_POINT('Ctrl Pts',(-0.214076109948858,0.00589294690488345,
0.0104034939904368));
#31177=CARTESIAN_POINT('Ctrl Pts',(-0.21407636473448,0.00589909273188374,
0.0104045923486797));
#31178=CARTESIAN_POINT('Ctrl Pts',(-0.214076623138809,0.00590524964646623,
0.0104056862898775));
#31179=CARTESIAN_POINT('',(-0.215095387779062,0.00254083911603525,0.00910817608666392));
#31180=CARTESIAN_POINT('Ctrl Pts',(-0.214881405086202,0.00590343232515273,
0.010423413516648));
#31181=CARTESIAN_POINT('Ctrl Pts',(-0.214880634996676,0.0058860381335411,
0.0104203038817212));
#31182=CARTESIAN_POINT('Ctrl Pts',(-0.214875181880235,0.00575899415021333,
0.0103971687692641));
#31183=CARTESIAN_POINT('Ctrl Pts',(-0.214863259396212,0.00540815197451475,
0.0103257881481459));
#31184=CARTESIAN_POINT('Ctrl Pts',(-0.21485881772863,0.00492199098674758,
0.0102003515580181));
#31185=CARTESIAN_POINT('Ctrl Pts',(-0.214879521846151,0.00428142262289701,
0.00998901365476671));
#31186=CARTESIAN_POINT('Ctrl Pts',(-0.21492306243039,0.00377039219960215,
0.00977517598710994));
#31187=CARTESIAN_POINT('Ctrl Pts',(-0.214961186236713,0.00345337595410416,
0.00962364176435926));
#31188=CARTESIAN_POINT('Ctrl Pts',(-0.214986535367109,0.00326005586289953,
0.00952561866829564));
#31189=CARTESIAN_POINT('Ctrl Pts',(-0.215011018507601,0.00308691740069967,
0.00943286197251718));
#31190=CARTESIAN_POINT('Ctrl Pts',(-0.215024066419253,0.00299903924354964,
0.00938388910997964));
#31191=CARTESIAN_POINT('Ctrl Pts',(-0.215051493871513,0.00281738091061636,
0.00928015442866946));
#31192=CARTESIAN_POINT('Ctrl Pts',(-0.215076239262129,0.00265981257200034,
0.0091845066913352));
#31193=CARTESIAN_POINT('Ctrl Pts',(-0.21509538156927,0.00254083793378764,
0.00910817641020345));
#31194=CARTESIAN_POINT('',(-0.216305478212088,0.00249450055261697,0.0091019248989092));
#31195=CARTESIAN_POINT('',(-0.216305478212094,0.00249450055261262,0.00910192489890646));
#31196=CARTESIAN_POINT('',(-0.216062907480361,0.00488362583018296,0.0102080439741779));
#31197=CARTESIAN_POINT('Ctrl Pts',(-0.216305476043056,0.00249442883403143,
0.00910203441955642));
#31198=CARTESIAN_POINT('Ctrl Pts',(-0.216285528067716,0.00261530638056923,
0.00918082306942033));
#31199=CARTESIAN_POINT('Ctrl Pts',(-0.216268407797524,0.00272160085692102,
0.00924619788180913));
#31200=CARTESIAN_POINT('Ctrl Pts',(-0.216253248996245,0.00281784221559503,
0.00930336533804196));
#31201=CARTESIAN_POINT('Ctrl Pts',(-0.216245669595605,0.00286596289493204,
0.00933194906615837));
#31202=CARTESIAN_POINT('Ctrl Pts',(-0.216238581667216,0.0029116046264753,
0.00935842590971943));
#31203=CARTESIAN_POINT('Ctrl Pts',(-0.216232848132246,0.00294879195706751,
0.00937969025108412));
#31204=CARTESIAN_POINT('Ctrl Pts',(-0.216227114597277,0.00298597928765971,
0.00940095459244882));
#31205=CARTESIAN_POINT('Ctrl Pts',(-0.216222732797858,0.00301463648393093,
0.00941713680921905));
#31206=CARTESIAN_POINT('Ctrl Pts',(-0.216216255707853,0.00305825974051661,
0.00944129560807781));
#31207=CARTESIAN_POINT('Ctrl Pts',(-0.216209778617848,0.00310188299710228,
0.00946545440693656));
#31208=CARTESIAN_POINT('Ctrl Pts',(-0.216201211043208,0.00316060313598794,
0.00949735579945492));
#31209=CARTESIAN_POINT('Ctrl Pts',(-0.216193623289001,0.00321437996309083,
0.00952579235973773));
#31210=CARTESIAN_POINT('Ctrl Pts',(-0.216186035534794,0.00326815679019373,
0.00955422892002053));
#31211=CARTESIAN_POINT('Ctrl Pts',(-0.216179424282587,0.00331690730906704,
0.00957936016153829));
#31212=CARTESIAN_POINT('Ctrl Pts',(-0.216173121802343,0.00336460771594108,
0.00960347034857651));
#31213=CARTESIAN_POINT('Ctrl Pts',(-0.216160516841855,0.00346000852968916,
0.00965169072265294));
#31214=CARTESIAN_POINT('Ctrl Pts',(-0.216149147333713,0.00355120858816052,
0.00969581189039489));
#31215=CARTESIAN_POINT('Ctrl Pts',(-0.21613851162561,0.00364634481300223,
0.00973989636120167));
#31216=CARTESIAN_POINT('Ctrl Pts',(-0.2161190043515,0.00382083704217086,
0.00982075302327328));
#31217=CARTESIAN_POINT('Ctrl Pts',(-0.216101977184963,0.00400880962548444,
0.00990097638128006));
#31218=CARTESIAN_POINT('Ctrl Pts',(-0.216089367063548,0.0042011026592489,
0.00997515160791293));
#31219=CARTESIAN_POINT('Ctrl Pts',(-0.216088226666079,0.00421849269713606,
0.00998185965123713));
#31220=CARTESIAN_POINT('Ctrl Pts',(-0.216087122393437,0.00423591729012979,
0.00998851982343922));
#31221=CARTESIAN_POINT('Ctrl Pts',(-0.216086055678229,0.00425336915853703,
0.00999512922278139));
#31222=CARTESIAN_POINT('Ctrl Pts',(-0.216073203026403,0.00446364345351091,
0.0100747646379956));
#31223=CARTESIAN_POINT('Ctrl Pts',(-0.216065801916377,0.00467803753865652,
0.0101467659415394));
#31224=CARTESIAN_POINT('Ctrl Pts',(-0.216062907480361,0.00488362583018296,
0.0102080439741779));
#31225=CARTESIAN_POINT('Ctrl Pts',(-0.216062901115481,0.00488407842295695,
0.0102081788612459));
#31226=CARTESIAN_POINT('Ctrl Pts',(-0.216060011174114,0.0050898046430285,
0.010269486110157));
#31227=CARTESIAN_POINT('Ctrl Pts',(-0.216061613315435,0.00528640638840204,
0.010320988079685));
#31228=CARTESIAN_POINT('Ctrl Pts',(-0.216067188608646,0.00550199323050043,
0.0103693743259898));
#31229=CARTESIAN_POINT('Ctrl Pts',(-0.216069976255251,0.00560978665154961,
0.0103935674491422));
#31230=CARTESIAN_POINT('Ctrl Pts',(-0.216073762550609,0.00572237856012717,
0.0104167410336067));
#31231=CARTESIAN_POINT('Ctrl Pts',(-0.216078386138244,0.00583381988821942,
0.0104375135503685));
#31232=CARTESIAN_POINT('Ctrl Pts',(-0.21607930894028,0.00585606198517916,
0.0104416594479437));
#31233=CARTESIAN_POINT('Ctrl Pts',(-0.216080264909954,0.00587825743762793,
0.0104457133990444));
#31234=CARTESIAN_POINT('Ctrl Pts',(-0.216081273279547,0.00590074222848906,
0.0104497344249182));
#31235=CARTESIAN_POINT('',(-0.216863172025247,0.00484538612872985,0.0102141167849625));
#31236=CARTESIAN_POINT('Ctrl Pts',(-0.216882060774437,0.00589894167293226,
0.0104673301115656));
#31237=CARTESIAN_POINT('Ctrl Pts',(-0.21688064798073,0.00586753673964817,
0.0104617001234162));
#31238=CARTESIAN_POINT('Ctrl Pts',(-0.216879344316105,0.00583690163752463,
0.0104560440440929));
#31239=CARTESIAN_POINT('Ctrl Pts',(-0.216878102848578,0.00580618452906231,
0.0104502144772882));
#31240=CARTESIAN_POINT('Ctrl Pts',(-0.216873527769665,0.00569298527727355,
0.0104287312507224));
#31241=CARTESIAN_POINT('Ctrl Pts',(-0.216869802272862,0.00557869658909491,
0.0104047720299247));
#31242=CARTESIAN_POINT('Ctrl Pts',(-0.216867065285671,0.00546980918598949,
0.0103798919273287));
#31243=CARTESIAN_POINT('Ctrl Pts',(-0.216861591311289,0.00525203437977865,
0.0103301317221365));
#31244=CARTESIAN_POINT('Ctrl Pts',(-0.216860045750518,0.00505561827550841,
0.0102778374033075));
#31245=CARTESIAN_POINT('Ctrl Pts',(-0.216863157842011,0.00484633783112493,
0.0102144052983154));
#31246=CARTESIAN_POINT('',(-0.217119273430717,0.0024305071256748,0.00907584540398619));
#31247=CARTESIAN_POINT('Ctrl Pts',(-0.216863172025247,0.00484538612872985,
0.0102141167849625));
#31248=CARTESIAN_POINT('Ctrl Pts',(-0.216866293584769,0.00463638521299101,
0.010150743228241));
#31249=CARTESIAN_POINT('Ctrl Pts',(-0.216874088025862,0.00441498954598536,
0.0100749918698983));
#31250=CARTESIAN_POINT('Ctrl Pts',(-0.216887342836659,0.00420167942231494,
0.00999259466276242));
#31251=CARTESIAN_POINT('Ctrl Pts',(-0.216900617768194,0.00398804549490104,
0.00991007237706179));
#31252=CARTESIAN_POINT('Ctrl Pts',(-0.216919362976275,0.0037823580735198,
0.00982120221383172));
#31253=CARTESIAN_POINT('Ctrl Pts',(-0.216941537033173,0.00359082137253702,
0.00973075178358121));
#31254=CARTESIAN_POINT('Ctrl Pts',(-0.216952624061622,0.00349505302204562,
0.00968552656845596));
#31255=CARTESIAN_POINT('Ctrl Pts',(-0.216964565666134,0.00340276546101606,
0.00964003070473679));
#31256=CARTESIAN_POINT('Ctrl Pts',(-0.216977870016699,0.0033064635405045,
0.00959041939952468));
#31257=CARTESIAN_POINT('Ctrl Pts',(-0.216984522191982,0.00325831258024871,
0.00956561374691862));
#31258=CARTESIAN_POINT('Ctrl Pts',(-0.216991514963515,0.00320915775019089,
0.00953978303292521));
#31259=CARTESIAN_POINT('Ctrl Pts',(-0.216999509061169,0.00315526226612399,
0.00951073631106921));
#31260=CARTESIAN_POINT('Ctrl Pts',(-0.217007503158823,0.00310136678205709,
0.00948168958921321));
#31261=CARTESIAN_POINT('Ctrl Pts',(-0.217016501721846,0.00304281090104423,
0.00944927559171635));
#31262=CARTESIAN_POINT('Ctrl Pts',(-0.217023463140776,0.00299839750608262,
0.00942420754471762));
#31263=CARTESIAN_POINT('Ctrl Pts',(-0.217030424559705,0.002953984111121,
0.00939913949771888));
#31264=CARTESIAN_POINT('Ctrl Pts',(-0.217035344236295,0.00292358530827852,
0.00938164187589816));
#31265=CARTESIAN_POINT('Ctrl Pts',(-0.217041614060813,0.00288528083541392,
0.00935929849242598));
#31266=CARTESIAN_POINT('Ctrl Pts',(-0.217047883885331,0.00284697636254933,
0.00933695510895381));
#31267=CARTESIAN_POINT('Ctrl Pts',(-0.217055506430902,0.00280084130501947,
0.0093096393351554));
#31268=CARTESIAN_POINT('Ctrl Pts',(-0.217063632569623,0.00275245324254402,
0.00928030736224485));
#31269=CARTESIAN_POINT('Ctrl Pts',(-0.217079884271406,0.00265568054541311,
0.00922164549430653));
#31270=CARTESIAN_POINT('Ctrl Pts',(-0.217098146072681,0.00254976472927551,
0.00915512598934796));
#31271=CARTESIAN_POINT('Ctrl Pts',(-0.217119270108823,0.00243050678069039,
0.00907584503782427));
#31272=CARTESIAN_POINT('',(-0.217721579458628,0.00223307602259744,0.00895185568871232));
#31273=CARTESIAN_POINT('Ctrl Pts',(-0.21711927235356,0.00243049410780578,
0.00907583661306065));
#31274=CARTESIAN_POINT('Ctrl Pts',(-0.21715405112409,0.0024102994618794,
0.00906302774800916));
#31275=CARTESIAN_POINT('Ctrl Pts',(-0.217180991959541,0.00239439998998887,
0.009052830909679));
#31276=CARTESIAN_POINT('Ctrl Pts',(-0.217281466712797,0.00234147243426244,
0.00901889238814732));
#31277=CARTESIAN_POINT('Ctrl Pts',(-0.21740416090901,0.00229616636516378,
0.00898995712725975));
#31278=CARTESIAN_POINT('Ctrl Pts',(-0.217546627510568,0.00225882515584664,
0.00896664401489687));
#31279=CARTESIAN_POINT('Ctrl Pts',(-0.217667742709476,0.00223981443389805,
0.00895557566262542));
#31280=CARTESIAN_POINT('Ctrl Pts',(-0.217721023725957,0.00223314551106483,
0.0089518940398779));
#31281=CARTESIAN_POINT('',(-0.218374009456864,0.00220395340354362,0.00894382805299407));
#31282=CARTESIAN_POINT('Ctrl Pts',(-0.217721579458628,0.00223307602259744,
0.00895185568871232));
#31283=CARTESIAN_POINT('Ctrl Pts',(-0.21777462485247,0.00222644993024188,
0.00894819969666044));
#31284=CARTESIAN_POINT('Ctrl Pts',(-0.217843500492621,0.00222071614871092,
0.00894546415784734));
#31285=CARTESIAN_POINT('Ctrl Pts',(-0.21795203985176,0.00221399343120396,
0.00894279214610887));
#31286=CARTESIAN_POINT('Ctrl Pts',(-0.218059615657004,0.00221007637826625,
0.00894209068652028));
#31287=CARTESIAN_POINT('Ctrl Pts',(-0.218090952814536,0.00220943320496267,
0.00894224077459141));
#31288=CARTESIAN_POINT('Ctrl Pts',(-0.218193344854828,0.00220709767477518,
0.00894256413753163));
#31289=CARTESIAN_POINT('Ctrl Pts',(-0.218292688378998,0.00220532673074213,
0.00894322944625219));
#31290=CARTESIAN_POINT('Ctrl Pts',(-0.218374009477688,0.0022039549723325,
0.00894382881947807));
#31291=CARTESIAN_POINT('Ctrl Pts',(-0.21837401321167,0.00220395490934618,
0.00894382884699923));
#31292=CARTESIAN_POINT('Ctrl Pts',(-0.218347327019386,0.00233073163754938,
0.00903391891599098));
#31293=CARTESIAN_POINT('Ctrl Pts',(-0.218313244025542,0.00249725023685972,
0.00914542258472829));
#31294=CARTESIAN_POINT('Ctrl Pts',(-0.218276224804953,0.00268641686649291,
0.00926436126954177));
#31295=CARTESIAN_POINT('Ctrl Pts',(-0.218259608411032,0.00277265227047954,
0.00931734129371121));
#31296=CARTESIAN_POINT('Ctrl Pts',(-0.218226397494956,0.00295607982361697,
0.00942555592083442));
#31297=CARTESIAN_POINT('Ctrl Pts',(-0.218193056409799,0.00315860668144401,
0.00953855943967181));
#31298=CARTESIAN_POINT('Ctrl Pts',(-0.218143468698842,0.00350244065109768,
0.00971834447840922));
#31299=CARTESIAN_POINT('Ctrl Pts',(-0.218096988684672,0.00398464218054674,
0.00994167473146692));
#31300=CARTESIAN_POINT('Ctrl Pts',(-0.218064351217329,0.00472231338075253,
0.0102132450057751));
#31301=CARTESIAN_POINT('Ctrl Pts',(-0.218061145319316,0.00533446433286351,
0.010381457620077));
#31302=CARTESIAN_POINT('Ctrl Pts',(-0.218071819718671,0.00573502223192124,
0.0104641816390526));
#31303=CARTESIAN_POINT('Ctrl Pts',(-0.218078126203157,0.00589629686000176,
0.0104933642872807));
#31304=CARTESIAN_POINT('',(-0.218872841325269,0.00457002221966434,0.0101695959270065));
#31305=CARTESIAN_POINT('Ctrl Pts',(-0.218877735683465,0.00589448248302666,
0.0105110260225545));
#31306=CARTESIAN_POINT('Ctrl Pts',(-0.218869908846724,0.00569722419377274,
0.0104751900008672));
#31307=CARTESIAN_POINT('Ctrl Pts',(-0.21885909932305,0.00524620508486855,
0.0103787976603652));
#31308=CARTESIAN_POINT('Ctrl Pts',(-0.218864452106764,0.00481504949286933,
0.0102534457740855));
#31309=CARTESIAN_POINT('Ctrl Pts',(-0.218872841325269,0.00457002221966434,
0.0101695959270065));
#31310=CARTESIAN_POINT('',(-0.219237122161378,0.00196588366579876,0.00878419704042442));
#31311=CARTESIAN_POINT('Ctrl Pts',(-0.218872841325269,0.00457002221966434,
0.0101695959270065));
#31312=CARTESIAN_POINT('Ctrl Pts',(-0.21887288147815,0.00456884945835792,
0.0101691946008402));
#31313=CARTESIAN_POINT('Ctrl Pts',(-0.218881377447727,0.0043214277508718,
0.0100844669395035));
#31314=CARTESIAN_POINT('Ctrl Pts',(-0.218909465557103,0.00380701625999766,
0.00988371263113285));
#31315=CARTESIAN_POINT('Ctrl Pts',(-0.218965255863169,0.00330128827775189,
0.00963459578682774));
#31316=CARTESIAN_POINT('Ctrl Pts',(-0.219023132009435,0.00294578045365914,
0.00943649611216199));
#31317=CARTESIAN_POINT('Ctrl Pts',(-0.219062281129155,0.00273678173079582,
0.00931208982376108));
#31318=CARTESIAN_POINT('Ctrl Pts',(-0.219100727104508,0.00255057403123827,
0.00919488413309952));
#31319=CARTESIAN_POINT('Ctrl Pts',(-0.219121593502578,0.00245608880301823,
0.00913290506119713));
#31320=CARTESIAN_POINT('Ctrl Pts',(-0.219165689106097,0.00226104671154717,
0.0090016478891487));
#31321=CARTESIAN_POINT('Ctrl Pts',(-0.219205899434897,0.00209250238596427,
0.00888065413454422));
#31322=CARTESIAN_POINT('Ctrl Pts',(-0.219237120080246,0.00196588454101197,
0.00878419780604263));
#31323=CARTESIAN_POINT('',(-0.220515396330818,0.00171983677662007,0.00861251054687271));
#31324=CARTESIAN_POINT('Ctrl Pts',(-0.219237121894096,0.00196588334575157,
0.00878419692442275));
#31325=CARTESIAN_POINT('Ctrl Pts',(-0.219299626976512,0.00192469477845702,
0.00875381637932707));
#31326=CARTESIAN_POINT('Ctrl Pts',(-0.219328791989107,0.00190449437925005,
0.00873852202848415));
#31327=CARTESIAN_POINT('Ctrl Pts',(-0.219370104955956,0.00188158207234747,
0.00872130386843637));
#31328=CARTESIAN_POINT('Ctrl Pts',(-0.219411418322426,0.0018586695438135,
0.00870408554183684));
#31329=CARTESIAN_POINT('Ctrl Pts',(-0.21946488229829,0.00183314526670501,
0.00868481535297067));
#31330=CARTESIAN_POINT('Ctrl Pts',(-0.219515065969969,0.00181363474941354,
0.00867012142979744));
#31331=CARTESIAN_POINT('Ctrl Pts',(-0.219565249641647,0.00179412423212207,
0.00865542750662421));
#31332=CARTESIAN_POINT('Ctrl Pts',(-0.219612152255416,0.00178059461885503,
0.00864535024413309));
#31333=CARTESIAN_POINT('Ctrl Pts',(-0.219667138977168,0.0017684847471806,
0.00863654086155548));
#31334=CARTESIAN_POINT('Ctrl Pts',(-0.21972212569892,0.00175637487550616,
0.00862773147897786));
#31335=CARTESIAN_POINT('Ctrl Pts',(-0.219785196792223,0.00174569649105899,
0.0086201757710797));
#31336=CARTESIAN_POINT('Ctrl Pts',(-0.219840326400044,0.00173864261881232,
0.00861542023136484));
#31337=CARTESIAN_POINT('Ctrl Pts',(-0.219895456007866,0.00173158874656564,
0.00861066469164997));
#31338=CARTESIAN_POINT('Ctrl Pts',(-0.219942644030734,0.00172815491285034,
0.00860871469223284));
#31339=CARTESIAN_POINT('Ctrl Pts',(-0.219995935354278,0.00172516870068701,
0.00860724722282935));
#31340=CARTESIAN_POINT('Ctrl Pts',(-0.22002258101605,0.00172367559460533,
0.00860651348812759));
#31341=CARTESIAN_POINT('Ctrl Pts',(-0.220050752516637,0.00172229500271428,
0.00860589965062664));
#31342=CARTESIAN_POINT('Ctrl Pts',(-0.2200834455773,0.00172127519818041,
0.00860566665592181));
#31343=CARTESIAN_POINT('Ctrl Pts',(-0.220116138637963,0.00172025539364654,
0.00860543366121698));
#31344=CARTESIAN_POINT('Ctrl Pts',(-0.220153353257484,0.00171959632170309,
0.00860558157489872));
#31345=CARTESIAN_POINT('Ctrl Pts',(-0.220177426297593,0.0017192735952131,
0.00860576272676545));
#31346=CARTESIAN_POINT('Ctrl Pts',(-0.220201499337701,0.00171895086872311,
0.00860594387863219));
#31347=CARTESIAN_POINT('Ctrl Pts',(-0.220212430798545,0.00171896449443078,
0.00860615826066572));
#31348=CARTESIAN_POINT('Ctrl Pts',(-0.220231151258488,0.00171895355001152,
0.00860649716681914));
#31349=CARTESIAN_POINT('Ctrl Pts',(-0.220249871718431,0.00171894260559226,
0.00860683607297256));
#31350=CARTESIAN_POINT('Ctrl Pts',(-0.220276381177714,0.00171890710174357,
0.0086072994902706));
#31351=CARTESIAN_POINT('Ctrl Pts',(-0.220305446991561,0.00171893726234777,
0.00860786466002522));
#31352=CARTESIAN_POINT('Ctrl Pts',(-0.220363496787337,0.00171899749864198,
0.00860899340835503));
#31353=CARTESIAN_POINT('Ctrl Pts',(-0.220431743233002,0.00171931965465264,
0.00861052802037448));
#31354=CARTESIAN_POINT('Ctrl Pts',(-0.220515396906419,0.0017198140099196,
0.00861249175807416));
#31355=CARTESIAN_POINT('',(-0.220090123052826,0.00418422702945123,0.0100543441066292));
#31356=CARTESIAN_POINT('Ctrl Pts',(-0.220515730216856,0.00171988949744531,
0.00861256027472298));
#31357=CARTESIAN_POINT('Ctrl Pts',(-0.2204787502135,0.00185191957789771,
0.00872086836689029));
#31358=CARTESIAN_POINT('Ctrl Pts',(-0.220431475220976,0.00202642732684206,
0.0088552288217874));
#31359=CARTESIAN_POINT('Ctrl Pts',(-0.220380060197333,0.00222577410457095,
0.00899883778024211));
#31360=CARTESIAN_POINT('Ctrl Pts',(-0.220356866873776,0.00231728500818783,
0.00906316072720875));
#31361=CARTESIAN_POINT('Ctrl Pts',(-0.220310804517265,0.0025107909266704,
0.00919355179597007));
#31362=CARTESIAN_POINT('Ctrl Pts',(-0.22026427845596,0.00272565546041714,
0.00933016407728968));
#31363=CARTESIAN_POINT('Ctrl Pts',(-0.220214048696187,0.00298877544138231,
0.0094869312743888));
#31364=CARTESIAN_POINT('Ctrl Pts',(-0.220168303850216,0.00329732711792897,
0.00965475980118518));
#31365=CARTESIAN_POINT('Ctrl Pts',(-0.220124020098812,0.00368476694613528,
0.0098472904300802));
#31366=CARTESIAN_POINT('Ctrl Pts',(-0.220100733172946,0.00399954421165778,
0.00998183202500825));
#31367=CARTESIAN_POINT('Ctrl Pts',(-0.220090123052826,0.00418422702945123,
0.0100543441066292));
#31368=CARTESIAN_POINT('Ctrl Pts',(-0.220090123052826,0.00418422702945123,
0.0100543441066292));
#31369=CARTESIAN_POINT('Ctrl Pts',(-0.220085741756582,0.00426048913833528,
0.0100842869260536));
#31370=CARTESIAN_POINT('Ctrl Pts',(-0.22006865820386,0.00459786319220902,
0.0102119119804006));
#31371=CARTESIAN_POINT('Ctrl Pts',(-0.220057266568638,0.00515049295929986,
0.0103826020783711));
#31372=CARTESIAN_POINT('Ctrl Pts',(-0.220068242884761,0.00565866356698218,
0.0104949899253311));
#31373=CARTESIAN_POINT('Ctrl Pts',(-0.220077799936617,0.00589176565002776,
0.0105374974776579));
#31374=CARTESIAN_POINT('',(-0.220878064831259,0.00441518816723556,0.010159021015619));
#31375=CARTESIAN_POINT('Ctrl Pts',(-0.220877304433504,0.005889967920973,
0.0105550654063144));
#31376=CARTESIAN_POINT('Ctrl Pts',(-0.220867873084289,0.00565698015616214,
0.0105124902878897));
#31377=CARTESIAN_POINT('Ctrl Pts',(-0.220857137503969,0.00515102574076155,
0.0104003859982906));
#31378=CARTESIAN_POINT('Ctrl Pts',(-0.220866927623,0.00467143026566601,
0.010252099464527));
#31379=CARTESIAN_POINT('Ctrl Pts',(-0.220878064831259,0.00441518816723555,
0.010159021015619));
#31380=CARTESIAN_POINT('',(-0.22131162872866,0.00171848461492949,0.00862620042871455));
#31381=CARTESIAN_POINT('Ctrl Pts',(-0.220878064831259,0.00441518816723555,
0.010159021015619));
#31382=CARTESIAN_POINT('Ctrl Pts',(-0.220878125769484,0.00441378611580685,
0.0101585117286085));
#31383=CARTESIAN_POINT('Ctrl Pts',(-0.220889418682641,0.00415468323385347,
0.0100643205656675));
#31384=CARTESIAN_POINT('Ctrl Pts',(-0.220915691899767,0.00375090589786667,
0.00989718271122343));
#31385=CARTESIAN_POINT('Ctrl Pts',(-0.220966875360685,0.00329663029328944,
0.00967108003973233));
#31386=CARTESIAN_POINT('Ctrl Pts',(-0.221011932596698,0.00298750926251152,
0.00950262161274992));
#31387=CARTESIAN_POINT('Ctrl Pts',(-0.221061613606449,0.00272319363643506,
0.00934478944388032));
#31388=CARTESIAN_POINT('Ctrl Pts',(-0.221107658471592,0.00250831974463547,
0.00920780036239895));
#31389=CARTESIAN_POINT('Ctrl Pts',(-0.22115290161688,0.00231659335985024,
0.00907833412010607));
#31390=CARTESIAN_POINT('Ctrl Pts',(-0.221176749851974,0.0022219001842754,
0.0090116372053751));
#31391=CARTESIAN_POINT('Ctrl Pts',(-0.221228087258136,0.00202224227626237,
0.00886734674608652));
#31392=CARTESIAN_POINT('Ctrl Pts',(-0.221275053893402,0.0018488960404024,
0.00873344289084019));
#31393=CARTESIAN_POINT('Ctrl Pts',(-0.221311628647049,0.00171848099653553,
0.00862620480166822));
#31394=CARTESIAN_POINT('',(-0.222515290917713,0.00171959987501164,0.00864956777322578));
#31395=CARTESIAN_POINT('',(-0.222515294138235,0.0017195974700428,0.00864957427254232));
#31396=CARTESIAN_POINT('',(-0.222078164866776,0.00441016936810972,0.0101832963470285));
#31397=CARTESIAN_POINT('Ctrl Pts',(-0.222515294294555,0.001719604422929,
0.00864956589294009));
#31398=CARTESIAN_POINT('Ctrl Pts',(-0.222478295083331,0.00185148585221865,
0.00875829495302256));
#31399=CARTESIAN_POINT('Ctrl Pts',(-0.222431004461355,0.00202580118070899,
0.00889315927644579));
#31400=CARTESIAN_POINT('Ctrl Pts',(-0.222379582487375,0.00222492582905654,
0.00903728689367557));
#31401=CARTESIAN_POINT('Ctrl Pts',(-0.222356400503344,0.00231628042355402,
0.00910180240101161));
#31402=CARTESIAN_POINT('Ctrl Pts',(-0.222310329407263,0.00250961375404974,
0.00923268188529682));
#31403=CARTESIAN_POINT('Ctrl Pts',(-0.222263805202746,0.00272427901799516,
0.00936978963283741));
#31404=CARTESIAN_POINT('Ctrl Pts',(-0.222213573950343,0.00298724356776438,
0.00952716266338013));
#31405=CARTESIAN_POINT('Ctrl Pts',(-0.222167882126563,0.00329538526363372,
0.00969550364880327));
#31406=CARTESIAN_POINT('Ctrl Pts',(-0.222116050585726,0.00374888191031054,
0.00992184840756128));
#31407=CARTESIAN_POINT('Ctrl Pts',(-0.22208954781103,0.00415219063406005,
0.0100892050101901));
#31408=CARTESIAN_POINT('Ctrl Pts',(-0.222078164866776,0.00441016936810972,
0.0101832963470285));
#31409=CARTESIAN_POINT('Ctrl Pts',(-0.222078164866776,0.00441016936810972,
0.0101832963470285));
#31410=CARTESIAN_POINT('Ctrl Pts',(-0.222066781922521,0.00466814810215939,
0.010277387683867));
#31411=CARTESIAN_POINT('Ctrl Pts',(-0.222056884058924,0.00514792738117401,
0.0104261488910504));
#31412=CARTESIAN_POINT('Ctrl Pts',(-0.222067759901967,0.00565493991166382,
0.0105388114001075));
#31413=CARTESIAN_POINT('Ctrl Pts',(-0.222077231673906,0.00588727068028781,
0.0105814273450436));
#31414=CARTESIAN_POINT('',(-0.222877366335621,0.00441446037918135,0.010202254105996));
#31415=CARTESIAN_POINT('Ctrl Pts',(-0.222876594854072,0.00588547347265862,
0.0105989910637735));
#31416=CARTESIAN_POINT('Ctrl Pts',(-0.222867236637191,0.0056535094866434,
0.0105563517608772));
#31417=CARTESIAN_POINT('Ctrl Pts',(-0.222856543043364,0.00514894106148145,
0.0104440457130052));
#31418=CARTESIAN_POINT('Ctrl Pts',(-0.222866259370916,0.00467063128315652,
0.0102956405003283));
#31419=CARTESIAN_POINT('Ctrl Pts',(-0.222877366335621,0.00441446037918135,
0.010202254105996));
#31420=CARTESIAN_POINT('',(-0.223310598441629,0.00172037808899711,0.00866504596072886));
#31421=CARTESIAN_POINT('Ctrl Pts',(-0.222877366335621,0.00441446037918135,
0.010202254105996));
#31422=CARTESIAN_POINT('Ctrl Pts',(-0.222877427216057,0.00441305623351044,
0.0102017422285763));
#31423=CARTESIAN_POINT('Ctrl Pts',(-0.222888689808771,0.00415402014935639,
0.0101072373799785));
#31424=CARTESIAN_POINT('Ctrl Pts',(-0.222914911877449,0.00375031358671893,
0.00993952094031038));
#31425=CARTESIAN_POINT('Ctrl Pts',(-0.222966020223457,0.00329641991277213,
0.00971274202800391));
#31426=CARTESIAN_POINT('Ctrl Pts',(-0.223010999642036,0.00298774591557504,
0.00954388284591602));
#31427=CARTESIAN_POINT('Ctrl Pts',(-0.223060660360825,0.00272361201166209,
0.00938554249185679));
#31428=CARTESIAN_POINT('Ctrl Pts',(-0.22310667914932,0.00250900816207285,
0.00924817752991824));
#31429=CARTESIAN_POINT('Ctrl Pts',(-0.223151897149871,0.00231757035963003,
0.00911838245209231));
#31430=CARTESIAN_POINT('Ctrl Pts',(-0.223175741921343,0.00222299932167633,
0.00905149866904686));
#31431=CARTESIAN_POINT('Ctrl Pts',(-0.223227067761469,0.00202363190136062,
0.00890682204395355));
#31432=CARTESIAN_POINT('Ctrl Pts',(-0.223274027990358,0.00185055987416555,
0.008772564000113));
#31433=CARTESIAN_POINT('Ctrl Pts',(-0.223310598360652,0.00172037449465496,
0.00866505028583386));
#31434=CARTESIAN_POINT('',(-0.22451413759973,0.00172149826865404,0.00868849301140827));
#31435=CARTESIAN_POINT('',(-0.224514141137082,0.00172149591023567,0.00868849946384148));
#31436=CARTESIAN_POINT('',(-0.224077512165814,0.00440948083533129,0.0102265543111367));
#31437=CARTESIAN_POINT('Ctrl Pts',(-0.224514141292166,0.00172150281505916,
0.00868849117770473));
#31438=CARTESIAN_POINT('Ctrl Pts',(-0.224477127539949,0.00185316341858383,
0.00879750297306098));
#31439=CARTESIAN_POINT('Ctrl Pts',(-0.224429821708012,0.0020272114172923,
0.00893272203677245));
#31440=CARTESIAN_POINT('Ctrl Pts',(-0.224378393526143,0.00222604404169074,
0.00907722494518334));
#31441=CARTESIAN_POINT('Ctrl Pts',(-0.224355212184233,0.00231725880918394,
0.00914190243096556));
#31442=CARTESIAN_POINT('Ctrl Pts',(-0.224309153980272,0.00251031221158726,
0.0092731150758879));
#31443=CARTESIAN_POINT('Ctrl Pts',(-0.224262658189644,0.00272469317168506,
0.00941058427657283));
#31444=CARTESIAN_POINT('Ctrl Pts',(-0.224212448790665,0.00298758394571889,
0.00956851511516764));
#31445=CARTESIAN_POINT('Ctrl Pts',(-0.22416695331413,0.00329483890266449,
0.00973701079873431));
#31446=CARTESIAN_POINT('Ctrl Pts',(-0.224115276532478,0.00374784709684887,
0.00996400980407875));
#31447=CARTESIAN_POINT('Ctrl Pts',(-0.224088854784422,0.00415138504334779,
0.0101320881672501));
#31448=CARTESIAN_POINT('Ctrl Pts',(-0.224077512165814,0.00440948083533129,
0.0102265543111367));
#31449=CARTESIAN_POINT('Ctrl Pts',(-0.224077512165814,0.00440948083533129,
0.0102265543111367));
#31450=CARTESIAN_POINT('Ctrl Pts',(-0.224066169547205,0.00466757662731479,
0.0103210204550233));
#31451=CARTESIAN_POINT('Ctrl Pts',(-0.224056346761501,0.00514637502274445,
0.0104699487051214));
#31452=CARTESIAN_POINT('Ctrl Pts',(-0.224067139686817,0.00565155572807021,
0.0105826959046413));
#31453=CARTESIAN_POINT('Ctrl Pts',(-0.224076522719914,0.00588277614622425,
0.010625353510046));
#31454=CARTESIAN_POINT('',(-0.224861013570565,0.00514872644714179,0.0104774172001444));
#31455=CARTESIAN_POINT('Ctrl Pts',(-0.224876132721504,0.00588096715315318,
0.010642983684972));
#31456=CARTESIAN_POINT('Ctrl Pts',(-0.224873876977941,0.00582530573000602,
0.0106327721265318));
#31457=CARTESIAN_POINT('Ctrl Pts',(-0.224871939109516,0.00577104612314958,
0.0106222934022558));
#31458=CARTESIAN_POINT('Ctrl Pts',(-0.224870228490649,0.00571703883957485,
0.0106113664450536));
#31459=CARTESIAN_POINT('Ctrl Pts',(-0.224864186040655,0.00552626793404857,
0.0105727689563051));
#31460=CARTESIAN_POINT('Ctrl Pts',(-0.224860982253214,0.0053386745032014,
0.010528627448495));
#31461=CARTESIAN_POINT('Ctrl Pts',(-0.224861013570565,0.00514872644714179,
0.0104774172001444));
#31462=CARTESIAN_POINT('',(-0.225016038273092,0.00296527551678717,0.00956936417862582));
#31463=CARTESIAN_POINT('Ctrl Pts',(-0.224861013572329,0.00514871576703485,
0.0104774143207667));
#31464=CARTESIAN_POINT('Ctrl Pts',(-0.224861045011535,0.00495876406267532,
0.0104262028476539));
#31465=CARTESIAN_POINT('Ctrl Pts',(-0.224864318374763,0.00476651357778983,
0.0103676238876547));
#31466=CARTESIAN_POINT('Ctrl Pts',(-0.224870299865164,0.00457982853857772,
0.0103039536618325));
#31467=CARTESIAN_POINT('Ctrl Pts',(-0.224874787677354,0.00443976187652935,
0.0102561829564754));
#31468=CARTESIAN_POINT('Ctrl Pts',(-0.224880794323499,0.00430277850927414,
0.0102057344389205));
#31469=CARTESIAN_POINT('Ctrl Pts',(-0.224888888524025,0.00416354177025105,
0.0101504648328106));
#31470=CARTESIAN_POINT('Ctrl Pts',(-0.22489158251621,0.00411719961630877,
0.0101320694537414));
#31471=CARTESIAN_POINT('Ctrl Pts',(-0.224894507758821,0.00407061140369965,
0.0101131309480136));
#31472=CARTESIAN_POINT('Ctrl Pts',(-0.224897685220289,0.00402359104486503,
0.0100935454711003));
#31473=CARTESIAN_POINT('Ctrl Pts',(-0.224910409483873,0.00383529625498036,
0.0100151146944838));
#31474=CARTESIAN_POINT('Ctrl Pts',(-0.224927195735951,0.00364029587212845,
0.00992575724485829));
#31475=CARTESIAN_POINT('Ctrl Pts',(-0.224947037735793,0.00346158123324218,
0.00983655079837782));
#31476=CARTESIAN_POINT('Ctrl Pts',(-0.224966879735635,0.00328286659435591,
0.00974734435189736));
#31477=CARTESIAN_POINT('Ctrl Pts',(-0.224989763415531,0.00312007330588168,
0.00965896274411867));
#31478=CARTESIAN_POINT('Ctrl Pts',(-0.225016038256768,0.00296527508664285,
0.00956936496560957));
#31479=CARTESIAN_POINT('',(-0.224916806541977,0.00225236367453649,0.00910630060086145));
#31480=CARTESIAN_POINT('Ctrl Pts',(-0.224916806541977,0.00225236367453649,
0.00910630060086145));
#31481=CARTESIAN_POINT('Ctrl Pts',(-0.224925107451042,0.0022867865741508,
0.00913108304394155));
#31482=CARTESIAN_POINT('Ctrl Pts',(-0.224934577499929,0.00232677962479607,
0.00915938195723326));
#31483=CARTESIAN_POINT('Ctrl Pts',(-0.224940840264972,0.00235358065782448,
0.00917812690403259));
#31484=CARTESIAN_POINT('Ctrl Pts',(-0.224943971647494,0.00236698117433867,
0.00918749937743225));
#31485=CARTESIAN_POINT('Ctrl Pts',(-0.224946300530641,0.00237706002817518,
0.00919451756818138));
#31486=CARTESIAN_POINT('Ctrl Pts',(-0.224949803337872,0.00239269484820365,
0.00920532904796304));
#31487=CARTESIAN_POINT('Ctrl Pts',(-0.224953306145103,0.00240832966823212,
0.00921614052774471));
#31488=CARTESIAN_POINT('Ctrl Pts',(-0.224957983354394,0.00242953672177531,
0.0092307213123541));
#31489=CARTESIAN_POINT('Ctrl Pts',(-0.224962642765517,0.0024523455269545,
0.00924621970596788));
#31490=CARTESIAN_POINT('Ctrl Pts',(-0.224967302176641,0.00247515433213368,
0.00926171809958165));
#31491=CARTESIAN_POINT('Ctrl Pts',(-0.224971944115544,0.00249957632337157,
0.00927811764714866));
#31492=CARTESIAN_POINT('Ctrl Pts',(-0.22497502021215,0.002516263112879,
0.00928924524523537));
#31493=CARTESIAN_POINT('Ctrl Pts',(-0.224978096308756,0.00253294990238644,
0.00930037284332207));
#31494=CARTESIAN_POINT('Ctrl Pts',(-0.224979605738828,0.00254187416662664,
0.00930626963940711));
#31495=CARTESIAN_POINT('Ctrl Pts',(-0.224981323970798,0.00255244156080663,
0.00931323962525843));
#31496=CARTESIAN_POINT('Ctrl Pts',(-0.224984760434737,0.00257357634916661,
0.00932717959696107));
#31497=CARTESIAN_POINT('Ctrl Pts',(-0.224989033102982,0.00260131561018695,
0.00934536288226375));
#31498=CARTESIAN_POINT('Ctrl Pts',(-0.224993267136316,0.00263670970994627,
0.00936812186650835));
#31499=CARTESIAN_POINT('Ctrl Pts',(-0.22499750116965,0.00267210380970558,
0.00939088085075294));
#31500=CARTESIAN_POINT('Ctrl Pts',(-0.225001697732016,0.00271519019647569,
0.00941815775499642));
#31501=CARTESIAN_POINT('Ctrl Pts',(-0.225004924284085,0.00275672452315482,
0.00944392421210905));
#31502=CARTESIAN_POINT('Ctrl Pts',(-0.225011377388222,0.00283979317651308,
0.0094954571263343));
#31503=CARTESIAN_POINT('Ctrl Pts',(-0.225013949525124,0.00291662592926665,
0.00954099361814959));
#31504=CARTESIAN_POINT('Ctrl Pts',(-0.225016038255883,0.00296527505804455,
0.00956936494893859));
#31505=CARTESIAN_POINT('',(-0.224893951312673,0.00215954182917785,0.00903842305818316));
#31506=CARTESIAN_POINT('Ctrl Pts',(-0.224894117235589,0.00215936362032008,
0.0090384489139208));
#31507=CARTESIAN_POINT('Ctrl Pts',(-0.224901382162618,0.00218904986783135,
0.00906039555723563));
#31508=CARTESIAN_POINT('Ctrl Pts',(-0.22490851174212,0.00221796610908876,
0.00908153639687648));
#31509=CARTESIAN_POINT('Ctrl Pts',(-0.224916806541977,0.00225236367453649,
0.00910630060086145));
#31510=CARTESIAN_POINT('',(-0.225192864116067,0.00215336578416129,0.0090401066669318));
#31511=CARTESIAN_POINT('Ctrl Pts',(-0.225192864116067,0.00215336578416129,
0.0090401066669318));
#31512=CARTESIAN_POINT('Ctrl Pts',(-0.225178650597281,0.00215018411373376,
0.0090375238652442));
#31513=CARTESIAN_POINT('Ctrl Pts',(-0.225106377344745,0.00214366180682612,
0.00903105599729165));
#31514=CARTESIAN_POINT('Ctrl Pts',(-0.225029554110752,0.00214766777237138,
0.00903226288021996));
#31515=CARTESIAN_POINT('Ctrl Pts',(-0.224982815408334,0.0021501049729653,
0.00903299713910372));
#31516=CARTESIAN_POINT('Ctrl Pts',(-0.224934623015444,0.00215576840919723,
0.00903656911590101));
#31517=CARTESIAN_POINT('Ctrl Pts',(-0.224894101884154,0.00215924465310947,
0.0090384761514828));
#31518=CARTESIAN_POINT('',(-0.225309762150681,0.00172192258384158,0.00870374069204483));
#31519=CARTESIAN_POINT('Ctrl Pts',(-0.225309727116455,0.00172192354877486,
0.0087037407145231));
#31520=CARTESIAN_POINT('Ctrl Pts',(-0.22530317830787,0.00174518401655161,
0.00872303397847708));
#31521=CARTESIAN_POINT('Ctrl Pts',(-0.225294343614693,0.00177668638927144,
0.00874892851577175));
#31522=CARTESIAN_POINT('Ctrl Pts',(-0.225285108854914,0.0018098826098087,
0.0087757558166547));
#31523=CARTESIAN_POINT('Ctrl Pts',(-0.225275874095134,0.00184307883034596,
0.00880258311753764));
#31524=CARTESIAN_POINT('Ctrl Pts',(-0.225266236284159,0.00187783685288663,
0.00883050216082895));
#31525=CARTESIAN_POINT('Ctrl Pts',(-0.225250743755804,0.00193502853970644,
0.00887505746406453));
#31526=CARTESIAN_POINT('Ctrl Pts',(-0.225242997491627,0.00196362438311634,
0.00889733511568232));
#31527=CARTESIAN_POINT('Ctrl Pts',(-0.22523378933279,0.00199790200373627,
0.00892367851192004));
#31528=CARTESIAN_POINT('Ctrl Pts',(-0.225226379114346,0.00202573868501456,
0.00894479940232736));
#31529=CARTESIAN_POINT('Ctrl Pts',(-0.225218968895902,0.00205357536629284,
0.00896592029273469));
#31530=CARTESIAN_POINT('Ctrl Pts',(-0.225213355324292,0.00207492092211016,
0.00898188540034371));
#31531=CARTESIAN_POINT('Ctrl Pts',(-0.225208692897504,0.0020927133473497,
0.00899512574048781));
#31532=CARTESIAN_POINT('Ctrl Pts',(-0.225199368044517,0.00212829819557704,
0.00902160641910038));
#31533=CARTESIAN_POINT('Ctrl Pts',(-0.225193848093542,0.00214968062354274,
0.00903717209931391));
#31534=CARTESIAN_POINT('Ctrl Pts',(-0.225192867237934,0.00215347928706473,
0.00903994966696521));
#31535=CARTESIAN_POINT('',(-0.226513589418857,0.00172251996741961,0.00872682375665345));
#31536=CARTESIAN_POINT('',(-0.226513566923304,0.00172248770006411,0.00872680494013574));
#31537=CARTESIAN_POINT('',(-0.226388511915541,0.00218154661642265,0.00908391582781536));
#31538=CARTESIAN_POINT('Origin',(-0.227809208820185,0.0077947739147323,
0.00186791552810384));
#31539=CARTESIAN_POINT('',(-0.227126457729194,0.00216864693516063,0.00908890020183529));
#31540=CARTESIAN_POINT('Ctrl Pts',(-0.227126457686547,0.00216864674301375,
0.00908890049261823));
#31541=CARTESIAN_POINT('Ctrl Pts',(-0.227069511598769,0.00216683783452681,
0.00908645418986856));
#31542=CARTESIAN_POINT('Ctrl Pts',(-0.226996374298308,0.00216473238471204,
0.00908347211408987));
#31543=CARTESIAN_POINT('Ctrl Pts',(-0.226950724459553,0.00216328058498747,
0.00908150913472941));
#31544=CARTESIAN_POINT('Ctrl Pts',(-0.226927899540175,0.00216255468512519,
0.00908052764504917));
#31545=CARTESIAN_POINT('Ctrl Pts',(-0.226911946486128,0.00216199220282908,
0.0090798009302647));
#31546=CARTESIAN_POINT('Ctrl Pts',(-0.226878445021426,0.00216151559286356,
0.00907879431088333));
#31547=CARTESIAN_POINT('Ctrl Pts',(-0.226844943556723,0.00216103898289804,
0.00907778769150196));
#31548=CARTESIAN_POINT('Ctrl Pts',(-0.22679389368015,0.00216064819788032,
0.00907650123031305));
#31549=CARTESIAN_POINT('Ctrl Pts',(-0.226755321775082,0.00216082600807531,
0.0090758780305106));
#31550=CARTESIAN_POINT('Ctrl Pts',(-0.226716749870014,0.00216100381827029,
0.00907525483070816));
#31551=CARTESIAN_POINT('Ctrl Pts',(-0.226690655937283,0.00216175025630935,
0.00907529484930442));
#31552=CARTESIAN_POINT('Ctrl Pts',(-0.226660619377659,0.00216286586100168,
0.00907552918802821));
#31553=CARTESIAN_POINT('Ctrl Pts',(-0.226645601097847,0.00216342366334784,
0.0090756463573901));
#31554=CARTESIAN_POINT('Ctrl Pts',(-0.226629597161646,0.00216407376972869,
0.00907581208977323));
#31555=CARTESIAN_POINT('Ctrl Pts',(-0.226616481400393,0.00216469456716155,
0.00907601255758363));
#31556=CARTESIAN_POINT('Ctrl Pts',(-0.22660336563914,0.0021653153645944,
0.00907621302539404));
#31557=CARTESIAN_POINT('Ctrl Pts',(-0.226593138052681,0.0021659068472081,
0.00907644823658608));
#31558=CARTESIAN_POINT('Ctrl Pts',(-0.226584540496384,0.0021663878207974,
0.00907663392975817));
#31559=CARTESIAN_POINT('Ctrl Pts',(-0.226575942940087,0.00216686879438671,
0.00907681962293026));
#31560=CARTESIAN_POINT('Ctrl Pts',(-0.226568975411353,0.00216723916088945,
0.00907695593104604));
#31561=CARTESIAN_POINT('Ctrl Pts',(-0.226550639842415,0.00216850438230813,
0.00907752745248047));
#31562=CARTESIAN_POINT('Ctrl Pts',(-0.226532304273477,0.00216976960372682,
0.00907809897391489));
#31563=CARTESIAN_POINT('Ctrl Pts',(-0.226502600673821,0.00217193003788991,
0.00907910522340853));
#31564=CARTESIAN_POINT('Ctrl Pts',(-0.226479110584875,0.00217375905389338,
0.00907998802605441));
#31565=CARTESIAN_POINT('Ctrl Pts',(-0.226432130408324,0.00217741708579578,
0.00908175363129572));
#31566=CARTESIAN_POINT('Ctrl Pts',(-0.226410004232402,0.00217974791219932,
0.00908302753406069));
#31567=CARTESIAN_POINT('Ctrl Pts',(-0.226389230132104,0.00218171579433513,
0.0090840616145203));
#31568=CARTESIAN_POINT('',(-0.227456889100304,0.00310986692736372,0.00970247513229321));
#31569=CARTESIAN_POINT('Ctrl Pts',(-0.227126457802366,0.00216864671205002,
0.00908890047209336));
#31570=CARTESIAN_POINT('Ctrl Pts',(-0.227159535805671,0.00227599956143099,
0.00916856953561649));
#31571=CARTESIAN_POINT('Ctrl Pts',(-0.227187513613841,0.00236732543188503,
0.00923287923821631));
#31572=CARTESIAN_POINT('Ctrl Pts',(-0.227212366497972,0.00244695262818679,
0.00928748991883584));
#31573=CARTESIAN_POINT('Ctrl Pts',(-0.227224792950202,0.0024867662589028,
0.00931479528147973));
#31574=CARTESIAN_POINT('Ctrl Pts',(-0.227236439141077,0.00252368956619642,
0.00933962692867829));
#31575=CARTESIAN_POINT('Ctrl Pts',(-0.227245326881853,0.00255182296877999,
0.0093583577637486));
#31576=CARTESIAN_POINT('Ctrl Pts',(-0.227254214622629,0.00257995637136356,
0.0093770885988189));
#31577=CARTESIAN_POINT('Ctrl Pts',(-0.227260341931496,0.00259923427900408,
0.00938981725628631));
#31578=CARTESIAN_POINT('Ctrl Pts',(-0.227271624596063,0.00263280783658688,
0.00941167475306709));
#31579=CARTESIAN_POINT('Ctrl Pts',(-0.22728290726063,0.00266638139416968,
0.00943353224984788));
#31580=CARTESIAN_POINT('Ctrl Pts',(-0.227299349172753,0.00271437568475871,
0.00946432593436038));
#31581=CARTESIAN_POINT('Ctrl Pts',(-0.227313897631145,0.00275564085759007,
0.00949028007023457));
#31582=CARTESIAN_POINT('Ctrl Pts',(-0.227328446089537,0.00279690603042142,
0.00951623420610876));
#31583=CARTESIAN_POINT('Ctrl Pts',(-0.227341097755956,0.00283134072815765,
0.00953751239998761));
#31584=CARTESIAN_POINT('Ctrl Pts',(-0.227355539970987,0.00286855708676149,
0.00956020192181762));
#31585=CARTESIAN_POINT('Ctrl Pts',(-0.227384424401048,0.00294298980396916,
0.00960558096547763));
#31586=CARTESIAN_POINT('Ctrl Pts',(-0.227420479239962,0.00302878982864503,
0.00965620512905418));
#31587=CARTESIAN_POINT('Ctrl Pts',(-0.227454425262618,0.00310438966814835,
0.00969935154573664));
#31588=CARTESIAN_POINT('Ctrl Pts',(-0.227455247752368,0.00310622140242,
0.0097003969549684));
#31589=CARTESIAN_POINT('Ctrl Pts',(-0.227456068999624,0.00310804702874932,
0.0097014381899936));
#31590=CARTESIAN_POINT('Ctrl Pts',(-0.227456889100304,0.00310986692736372,
0.00970247513229321));
#31591=CARTESIAN_POINT('',(-0.227996742054428,0.00407722443014096,0.010182633458461));
#31592=CARTESIAN_POINT('Ctrl Pts',(-0.227456889100304,0.00310986692736372,
0.00970247513229321));
#31593=CARTESIAN_POINT('Ctrl Pts',(-0.227489916419944,0.00318315234385685,
0.0097442455461831));
#31594=CARTESIAN_POINT('Ctrl Pts',(-0.227521084158742,0.00324691103035285,
0.00977946177872144));
#31595=CARTESIAN_POINT('Ctrl Pts',(-0.227556657287862,0.00331641920530898,
0.00981682420858073));
#31596=CARTESIAN_POINT('Ctrl Pts',(-0.227593113732605,0.00338765333629757,
0.00985511438415112));
#31597=CARTESIAN_POINT('Ctrl Pts',(-0.227634201182863,0.0034650263648679,
0.00989546321334494));
#31598=CARTESIAN_POINT('Ctrl Pts',(-0.227677579152443,0.00354337392575307,
0.00993486812925494));
#31599=CARTESIAN_POINT('Ctrl Pts',(-0.227720957122022,0.00362172148663825,
0.00997427304516493));
#31600=CARTESIAN_POINT('Ctrl Pts',(-0.227766623657143,0.00370099813863763,
0.0100128262267389));
#31601=CARTESIAN_POINT('Ctrl Pts',(-0.22781719085636,0.0037856188794736,
0.0100523849767061));
#31602=CARTESIAN_POINT('Ctrl Pts',(-0.227867758055577,0.00387023962030957,
0.0100919437266733));
#31603=CARTESIAN_POINT('Ctrl Pts',(-0.227923229539478,0.003960286039776,
0.0101323378246218));
#31604=CARTESIAN_POINT('Ctrl Pts',(-0.227975492399613,0.00404349318073738,
0.01016818210575));
#31605=CARTESIAN_POINT('Ctrl Pts',(-0.227982632850327,0.00405486141599234,
0.0101730793563429));
#31606=CARTESIAN_POINT('Ctrl Pts',(-0.227989713277371,0.0040661009235916,
0.0101778942512805));
#31607=CARTESIAN_POINT('Ctrl Pts',(-0.227996742054428,0.00407722443014096,
0.010182633458461));
#31608=CARTESIAN_POINT('',(-0.229324382301549,0.00587096534799219,0.0107407249786847));
#31609=CARTESIAN_POINT('Ctrl Pts',(-0.227996742054428,0.00407722443014096,
0.010182633458461));
#31610=CARTESIAN_POINT('Ctrl Pts',(-0.228012423148243,0.00410204034163872,
0.0101932074978731));
#31611=CARTESIAN_POINT('Ctrl Pts',(-0.228027847164962,0.00412627831447172,
0.0102034059753793));
#31612=CARTESIAN_POINT('Ctrl Pts',(-0.22804310708817,0.00415007794112182,
0.0102133064578917));
#31613=CARTESIAN_POINT('Ctrl Pts',(-0.228121134654993,0.00427177101477283,
0.0102639299472963));
#31614=CARTESIAN_POINT('Ctrl Pts',(-0.228194871969436,0.0043818969845919,
0.0103070169724305));
#31615=CARTESIAN_POINT('Ctrl Pts',(-0.228276749669893,0.00450012916764758,
0.0103506786545054));
#31616=CARTESIAN_POINT('Ctrl Pts',(-0.228381817769972,0.00465184850969786,
0.0104067067299922));
#31617=CARTESIAN_POINT('Ctrl Pts',(-0.228500318179664,0.00481723537212066,
0.0104627171434107));
#31618=CARTESIAN_POINT('Ctrl Pts',(-0.228612318903402,0.00496837639600633,
0.0105095656396236));
#31619=CARTESIAN_POINT('Ctrl Pts',(-0.22872431962714,0.00511951741989199,
0.0105564141358366));
#31620=CARTESIAN_POINT('Ctrl Pts',(-0.228829799907357,0.00525615538408106,
0.0105950375950328));
#31621=CARTESIAN_POINT('Ctrl Pts',(-0.228946501527974,0.00540372976852625,
0.0106330700434848));
#31622=CARTESIAN_POINT('Ctrl Pts',(-0.22906320314859,0.00555130415297142,
0.0106711024919367));
#31623=CARTESIAN_POINT('Ctrl Pts',(-0.229191139018856,0.00570993073471519,
0.0107079668985551));
#31624=CARTESIAN_POINT('Ctrl Pts',(-0.229324382301549,0.00587096534799219,
0.0107407249786847));
#31625=CARTESIAN_POINT('',(-0.224906597392078,-0.00157591257448374,-2.26466145009483E-7));
#31626=CARTESIAN_POINT('Ctrl Pts',(-0.229324382301549,0.00587096534799201,
0.0107407249786846));
#31627=CARTESIAN_POINT('Ctrl Pts',(-0.229485744817183,0.0056945111294132,
0.0107117116946865));
#31628=CARTESIAN_POINT('Ctrl Pts',(-0.229627896419902,0.00553927467669799,
0.0106807434520244));
#31629=CARTESIAN_POINT('Ctrl Pts',(-0.229747893835773,0.00540811338586742,
0.0106519514001228));
#31630=CARTESIAN_POINT('Ctrl Pts',(-0.229807892543708,0.00534253274045213,
0.010637555374172));
#31631=CARTESIAN_POINT('Ctrl Pts',(-0.229862352234134,0.00528296668078184,
0.0106237244445399));
#31632=CARTESIAN_POINT('Ctrl Pts',(-0.229914217593376,0.00522607416888484,
0.0106099639475152));
#31633=CARTESIAN_POINT('Ctrl Pts',(-0.229940150272997,0.00519762791293634,
0.0106030836990029));
#31634=CARTESIAN_POINT('Ctrl Pts',(-0.229965434797737,0.00516985488092608,
0.0105962018001159));
#31635=CARTESIAN_POINT('Ctrl Pts',(-0.229986021469801,0.00514724062456104,
0.0105905104176317));
#31636=CARTESIAN_POINT('Ctrl Pts',(-0.230006608141864,0.005124626368196,
0.0105848190351475));
#31637=CARTESIAN_POINT('Ctrl Pts',(-0.230022495585796,0.00510715427844391,
0.0105803802154135));
#31638=CARTESIAN_POINT('Ctrl Pts',(-0.23005025334464,0.00507646845205036,
0.0105723820814782));
#31639=CARTESIAN_POINT('Ctrl Pts',(-0.230078011103483,0.00504578262565681,
0.0105643839475428));
#31640=CARTESIAN_POINT('Ctrl Pts',(-0.230117641989443,0.0050019184211765,
0.0105526994501915));
#31641=CARTESIAN_POINT('Ctrl Pts',(-0.230153258691976,0.00496237482800372,
0.0105418193756453));
#31642=CARTESIAN_POINT('Ctrl Pts',(-0.230188875394509,0.00492283123483093,
0.0105309393010992));
#31643=CARTESIAN_POINT('Ctrl Pts',(-0.230220475803366,0.00488757956722113,
0.0105209592922955));
#31644=CARTESIAN_POINT('Ctrl Pts',(-0.230251831073634,0.00485249570357078,
0.0105108075114764));
#31645=CARTESIAN_POINT('Ctrl Pts',(-0.23031454161417,0.00478232797627009,
0.010490503949838));
#31646=CARTESIAN_POINT('Ctrl Pts',(-0.230376273367701,0.0047128594595253,
0.010469432600821));
#31647=CARTESIAN_POINT('Ctrl Pts',(-0.230435676939916,0.0046452906084165,
0.0104480309058724));
#31648=CARTESIAN_POINT('Ctrl Pts',(-0.230495080512131,0.0045777217573077,
0.0104266292109238));
#31649=CARTESIAN_POINT('Ctrl Pts',(-0.230552156757354,0.00451206165996326,
0.0104048588721916));
#31650=CARTESIAN_POINT('Ctrl Pts',(-0.230601790943484,0.00445464998250786,
0.0103851864819408));
#31651=CARTESIAN_POINT('Ctrl Pts',(-0.230651425129614,0.00439723830505247,
0.01036551409169));
#31652=CARTESIAN_POINT('Ctrl Pts',(-0.230693612158977,0.00434799447567126,
0.0103481724261956));
#31653=CARTESIAN_POINT('Ctrl Pts',(-0.230750173084339,0.00428034173840896,
0.0103233211117964));
#31654=CARTESIAN_POINT('Ctrl Pts',(-0.230785698409411,0.00423784976240384,
0.0103077122613954));
#31655=CARTESIAN_POINT('Ctrl Pts',(-0.230826898018337,0.00418813941981296,
0.0102890255602644));
#31656=CARTESIAN_POINT('Ctrl Pts',(-0.230868043325356,0.0041380196585314,
0.0102695877777448));
#31657=CARTESIAN_POINT('Ctrl Pts',(-0.230892406683903,0.00410834225902144,
0.0102580780892971));
#31658=CARTESIAN_POINT('Ctrl Pts',(-0.230916751003245,0.00407851845553815,
0.0102463132904993));
#31659=CARTESIAN_POINT('Ctrl Pts',(-0.230939886965452,0.00404993141261438,
0.0102348560676729));
#31660=CARTESIAN_POINT('Ctrl Pts',(-0.231002095384207,0.00397306602351662,
0.010204049667274));
#31661=CARTESIAN_POINT('Ctrl Pts',(-0.231055560302718,0.00390508230307037,
0.0101755863206212));
#31662=CARTESIAN_POINT('Ctrl Pts',(-0.231107716218532,0.00383663463987516,
0.0101459342198134));
#31663=CARTESIAN_POINT('Ctrl Pts',(-0.231159872134346,0.00376818697667996,
0.0101162821190056));
#31664=CARTESIAN_POINT('Ctrl Pts',(-0.231210722559944,0.00369934908414583,
0.0100852775894019));
#31665=CARTESIAN_POINT('Ctrl Pts',(-0.23125366084358,0.0036401127425717,
0.0100578020810351));
#31666=CARTESIAN_POINT('Ctrl Pts',(-0.231296599127216,0.00358087640099757,
0.0100303265726683));
#31667=CARTESIAN_POINT('Ctrl Pts',(-0.231331618607131,0.00353109481495246,
0.010006692012866));
#31668=CARTESIAN_POINT('Ctrl Pts',(-0.231377720840595,0.0034600055015645,
0.00997160014698702));
#31669=CARTESIAN_POINT('Ctrl Pts',(-0.231423823074059,0.00338891618817653,
0.00993650828110805));
#31670=CARTESIAN_POINT('Ctrl Pts',(-0.23148101976334,0.00329679652888858,
0.00988940692844755));
#31671=CARTESIAN_POINT('Ctrl Pts',(-0.231528065134197,0.00321433493027825,
0.00984527396904159));
#31672=CARTESIAN_POINT('Ctrl Pts',(-0.231575110505053,0.00313187333166792,
0.00980114100963563));
#31673=CARTESIAN_POINT('Ctrl Pts',(-0.231611996080783,0.00305884309754429,
0.00976038232476601));
#31674=CARTESIAN_POINT('Ctrl Pts',(-0.231644324891522,0.00298614562233681,
0.00971846121248706));
#31675=CARTESIAN_POINT('Ctrl Pts',(-0.231676653702261,0.00291344814712933,
0.00967654010020812));
#31676=CARTESIAN_POINT('Ctrl Pts',(-0.231704428636809,0.00284116801872021,
0.00963331648308124));
#31677=CARTESIAN_POINT('Ctrl Pts',(-0.231726500112571,0.00277498507141569,
0.00959250676879874));
#31678=CARTESIAN_POINT('Ctrl Pts',(-0.231748571588332,0.00270880212411118,
0.00955169705451624));
#31679=CARTESIAN_POINT('Ctrl Pts',(-0.231764936016148,0.002648611310996,
0.00951347529255092));
#31680=CARTESIAN_POINT('Ctrl Pts',(-0.231774590797342,0.0025803707591514,
0.00946864508580836));
#31681=CARTESIAN_POINT('Ctrl Pts',(-0.23179390035973,0.00244388965546221,
0.00937898467232322));
#31682=CARTESIAN_POINT('Ctrl Pts',(-0.231786404517407,0.00227626681505629,
0.00926125907006112));
#31683=CARTESIAN_POINT('Ctrl Pts',(-0.231750544825356,0.00213535898381207,
0.00915480893757784));
#31684=CARTESIAN_POINT('Ctrl Pts',(-0.23173261497933,0.00206490506818996,
0.00910158387133621));
#31685=CARTESIAN_POINT('Ctrl Pts',(-0.231707586904214,0.00200084815486611,
0.00905154880698267));
#31686=CARTESIAN_POINT('Ctrl Pts',(-0.231673809741403,0.00193360097644109,
0.00899738195505023));
#31687=CARTESIAN_POINT('Ctrl Pts',(-0.231640032578592,0.00186635379801606,
0.00894321510311779));
#31688=CARTESIAN_POINT('Ctrl Pts',(-0.231597510631657,0.00179609770624624,
0.00888469242584056));
#31689=CARTESIAN_POINT('Ctrl Pts',(-0.231556525129873,0.00173699192756572,
0.00883408314100965));
#31690=CARTESIAN_POINT('Ctrl Pts',(-0.231515539628089,0.0016778861488852,
0.00878347385617874));
#31691=CARTESIAN_POINT('Ctrl Pts',(-0.231476085454303,0.00162970072198407,
0.00874104870017571));
#31692=CARTESIAN_POINT('Ctrl Pts',(-0.231426392419699,0.0015747691240097,
0.00869151559050962));
#31693=CARTESIAN_POINT('Ctrl Pts',(-0.231376699385095,0.00151983752603534,
0.00864198248084354));
#31694=CARTESIAN_POINT('Ctrl Pts',(-0.231316772114654,0.00145838108383666,
0.00858509258491536));
#31695=CARTESIAN_POINT('Ctrl Pts',(-0.23125919197483,0.00140349285592715,
0.00853288079893833));
#31696=CARTESIAN_POINT('Ctrl Pts',(-0.231210636673531,0.00135720754901295,
0.0084888524411187));
#31697=CARTESIAN_POINT('Ctrl Pts',(-0.23116374812206,0.00131548725337962,
0.00844826339887426));
#31698=CARTESIAN_POINT('Ctrl Pts',(-0.231113995310445,0.00127324558096312,
0.00840637618589869));
#31699=CARTESIAN_POINT('Ctrl Pts',(-0.231104747894015,0.00126539423904196,
0.0083985907263659));
#31700=CARTESIAN_POINT('Ctrl Pts',(-0.231095401527076,0.00125752597447957,
0.00839075932832244));
#31701=CARTESIAN_POINT('Ctrl Pts',(-0.231085927115632,0.00124960959671496,
0.00838285012440887));
#31702=CARTESIAN_POINT('Ctrl Pts',(-0.23102547861739,0.00119910164166131,
0.0083323879398523));
#31703=CARTESIAN_POINT('Ctrl Pts',(-0.230959820200585,0.0011467024285488,
0.00827868812707598));
#31704=CARTESIAN_POINT('Ctrl Pts',(-0.230900331854038,0.00110097593680334,
0.00823078821303766));
#31705=CARTESIAN_POINT('Ctrl Pts',(-0.230840843507491,0.00105524944505788,
0.00818288829899935));
#31706=CARTESIAN_POINT('Ctrl Pts',(-0.230787522564886,0.00101604021632565,
0.00814094057038923));
#31707=CARTESIAN_POINT('Ctrl Pts',(-0.230723706818146,0.00097086547440946,
0.00809157173241625));
#31708=CARTESIAN_POINT('Ctrl Pts',(-0.230659891071407,0.000925690732493274,
0.00804220289444327));
#31709=CARTESIAN_POINT('Ctrl Pts',(-0.230585583966631,0.000874763691592227,
0.00798521205356764));
#31710=CARTESIAN_POINT('Ctrl Pts',(-0.230523287813335,0.000833165462424795,
0.0079376563861729));
#31711=CARTESIAN_POINT('Ctrl Pts',(-0.230460991660039,0.000791567233257364,
0.00789010071877815));
#31712=CARTESIAN_POINT('Ctrl Pts',(-0.230410702851443,0.000759054428482579,
0.00785219731383282));
#31713=CARTESIAN_POINT('Ctrl Pts',(-0.230346995596142,0.000718726127249372,
0.00780428928871881));
#31714=CARTESIAN_POINT('Ctrl Pts',(-0.230283288340841,0.00067839782601616,
0.00775638126360478));
#31715=CARTESIAN_POINT('Ctrl Pts',(-0.230206165710844,0.000630473690801921,
0.00769827947888727));
#31716=CARTESIAN_POINT('Ctrl Pts',(-0.230134314763537,0.000586713602453529,
0.00764390620766072));
#31717=CARTESIAN_POINT('Ctrl Pts',(-0.229990612868923,0.000499193425756742,
0.00753515966520764));
#31718=CARTESIAN_POINT('Ctrl Pts',(-0.229867988787896,0.000427617586995964,
0.00744190204492346));
#31719=CARTESIAN_POINT('Ctrl Pts',(-0.229741940634664,0.000354928579326137,
0.00734383067639073));
#31720=CARTESIAN_POINT('Ctrl Pts',(-0.229615892481431,0.00028223957165631,
0.00724575930785799));
#31721=CARTESIAN_POINT('Ctrl Pts',(-0.229486422667975,0.000208701022860158,
0.00714269334481202));
#31722=CARTESIAN_POINT('Ctrl Pts',(-0.229352791967108,0.000133484776569742,
0.0070323021258392));
#31723=CARTESIAN_POINT('Ctrl Pts',(-0.22921916126624,5.82685302793252E-5,
0.00692191090686637));
#31724=CARTESIAN_POINT('Ctrl Pts',(-0.2290813721816,-1.84076324743832E-5,
0.00680402683203074));
#31725=CARTESIAN_POINT('Ctrl Pts',(-0.228955658434579,-8.75292797473743E-5,
0.00669278534604856));
#31726=CARTESIAN_POINT('Ctrl Pts',(-0.228829944687559,-0.000156650927020365,
0.00658154386006638));
#31727=CARTESIAN_POINT('Ctrl Pts',(-0.228716302957634,-0.000218638491031281,
0.00647721522647426));
#31728=CARTESIAN_POINT('Ctrl Pts',(-0.228596767895078,-0.000283494680059439,
0.00636287399597081));
#31729=CARTESIAN_POINT('Ctrl Pts',(-0.228477232832522,-0.000348350869087597,
0.00624853276546736));
#31730=CARTESIAN_POINT('Ctrl Pts',(-0.22835180668064,-0.000415691458055748,
0.0061239593033855));
#31731=CARTESIAN_POINT('Ctrl Pts',(-0.228232000846924,-0.000479070930306836,
0.0059999892371026));
#31732=CARTESIAN_POINT('Ctrl Pts',(-0.228112195013208,-0.000542450402557927,
0.00587601917081969));
#31733=CARTESIAN_POINT('Ctrl Pts',(-0.2279980084523,-0.000602119731771134,
0.00575278162222749));
#31734=CARTESIAN_POINT('Ctrl Pts',(-0.227883788318796,-0.000660850298491323,
0.00562412203559087));
#31735=CARTESIAN_POINT('Ctrl Pts',(-0.227876478715098,-0.000664608805459833,
0.00561588836818488));
#31736=CARTESIAN_POINT('Ctrl Pts',(-0.227869168977206,-0.000668363094667602,
0.00560763228811735));
#31737=CARTESIAN_POINT('Ctrl Pts',(-0.227861859699312,-0.000672112681594339,
0.00559935444695225));
#31738=CARTESIAN_POINT('Ctrl Pts',(-0.227640738892288,-0.000785545458312897,
0.0053489325933084));
#31739=CARTESIAN_POINT('Ctrl Pts',(-0.227420039070301,-0.000894106965719931,
0.00507834839397145));
#31740=CARTESIAN_POINT('Ctrl Pts',(-0.227216211219934,-0.000988261310786297,
0.00480738120895063));
#31741=CARTESIAN_POINT('Ctrl Pts',(-0.227005645720493,-0.00108552798292046,
0.00452745704479274));
#31742=CARTESIAN_POINT('Ctrl Pts',(-0.226813087273762,-0.00116864465803599,
0.00424754273693657));
#31743=CARTESIAN_POINT('Ctrl Pts',(-0.226626103958878,-0.00124135927987506,
0.00394958116680215));
#31744=CARTESIAN_POINT('Ctrl Pts',(-0.226439120643995,-0.00131407390171413,
0.00365161959666774));
#31745=CARTESIAN_POINT('Ctrl Pts',(-0.226257707321489,-0.00137553841474053,
0.00333545181780753));
#31746=CARTESIAN_POINT('Ctrl Pts',(-0.226089207901399,-0.00142040472594693,
0.00300946340189435));
#31747=CARTESIAN_POINT('Ctrl Pts',(-0.226004958191353,-0.00144283788155013,
0.00284646919393776));
#31748=CARTESIAN_POINT('Ctrl Pts',(-0.225923937374762,-0.00146113181346843,
0.00268101115962903));
#31749=CARTESIAN_POINT('Ctrl Pts',(-0.225847547993418,-0.00147482232186643,
0.00251597950542847));
#31750=CARTESIAN_POINT('Ctrl Pts',(-0.225818640550089,-0.00148000311517418,
0.00245352785171381));
#31751=CARTESIAN_POINT('Ctrl Pts',(-0.225790395885862,-0.00148452982481028,
0.00239113705018023));
#31752=CARTESIAN_POINT('Ctrl Pts',(-0.225762905281085,-0.0014883945315704,
0.0023290706209163));
#31753=CARTESIAN_POINT('Ctrl Pts',(-0.225717750572063,-0.00149474250792893,
0.00222712337107818));
#31754=CARTESIAN_POINT('Ctrl Pts',(-0.22567463029465,-0.00150078983555668,
0.00212686157789403));
#31755=CARTESIAN_POINT('Ctrl Pts',(-0.225633948962841,-0.00150645162391577,
0.00202917774223495));
#31756=CARTESIAN_POINT('Ctrl Pts',(-0.225568500459705,-0.00151556036142999,
0.00187202308332373));
#31757=CARTESIAN_POINT('Ctrl Pts',(-0.22550935008619,-0.00152369977831173,
0.00172226264086029));
#31758=CARTESIAN_POINT('Ctrl Pts',(-0.225446995528993,-0.00153173773051723,
0.00155812389680787));
#31759=CARTESIAN_POINT('Ctrl Pts',(-0.225415818250395,-0.00153575670661998,
0.00147605452478166));
#31760=CARTESIAN_POINT('Ctrl Pts',(-0.225383839889912,-0.00153973931552829,
0.00139038950423513));
#31761=CARTESIAN_POINT('Ctrl Pts',(-0.225350428018386,-0.00154367377477953,
0.00129873283310492));
#31762=CARTESIAN_POINT('Ctrl Pts',(-0.225333143387235,-0.00154570914944814,
0.00125131699913256));
#31763=CARTESIAN_POINT('Ctrl Pts',(-0.225315474932153,-0.00154772690563975,
0.00120229607496713));
#31764=CARTESIAN_POINT('Ctrl Pts',(-0.22529824089363,-0.00154961912800569,
0.00115406788678273));
#31765=CARTESIAN_POINT('Ctrl Pts',(-0.225282160858165,-0.00155138464586217,
0.00110906909120891));
#31766=CARTESIAN_POINT('Ctrl Pts',(-0.225266459009404,-0.00155304119210587,
0.00106475974768948));
#31767=CARTESIAN_POINT('Ctrl Pts',(-0.225251799978657,-0.0015545307347765,
0.00102308441757244));
#31768=CARTESIAN_POINT('Ctrl Pts',(-0.225221429894213,-0.00155761671893654,
0.000936742877217953));
#31769=CARTESIAN_POINT('Ctrl Pts',(-0.225195537030683,-0.00156003488278947,
0.000861712337668546));
#31770=CARTESIAN_POINT('Ctrl Pts',(-0.225167559666854,-0.00156240338782803,
0.000779963840828957));
#31771=CARTESIAN_POINT('Ctrl Pts',(-0.22515357098494,-0.00156358764034731,
0.000739089592409159));
#31772=CARTESIAN_POINT('Ctrl Pts',(-0.225139061085489,-0.00156475364739107,
0.000696535807052153));
#31773=CARTESIAN_POINT('Ctrl Pts',(-0.225123079429075,-0.00156594368006901,
0.00064931564366595));
#31774=CARTESIAN_POINT('Ctrl Pts',(-0.225107097772661,-0.00156713371274695,
0.000602095480279747));
#31775=CARTESIAN_POINT('Ctrl Pts',(-0.225089643911978,-0.0015683181027373,
0.000550208270623167));
#31776=CARTESIAN_POINT('Ctrl Pts',(-0.225077025803377,-0.00156911396238647,
0.00051259631297856));
#31777=CARTESIAN_POINT('Ctrl Pts',(-0.225064407694775,-0.00156990982203563,
0.000474984355333953));
#31778=CARTESIAN_POINT('Ctrl Pts',(-0.2250566260427,-0.00157036307013134,
0.000451648374351342));
#31779=CARTESIAN_POINT('Ctrl Pts',(-0.225045952903868,-0.00157095070842386,
0.000419612674057864));
#31780=CARTESIAN_POINT('Ctrl Pts',(-0.225035279765036,-0.00157153834671639,
0.000387576973764386));
#31781=CARTESIAN_POINT('Ctrl Pts',(-0.225021714740738,-0.00157223455280892,
0.000346841231436762));
#31782=CARTESIAN_POINT('Ctrl Pts',(-0.225007189961945,-0.0015728802645566,
0.000303151418613095));
#31783=CARTESIAN_POINT('Ctrl Pts',(-0.224978140533459,-0.00157417168231261,
0.000215772181298103));
#31784=CARTESIAN_POINT('Ctrl Pts',(-0.22494525294181,-0.00157531381840194,
0.000116577087333678));
#31785=CARTESIAN_POINT('Ctrl Pts',(-0.224906594466267,-0.00157591540148865,
-2.25483220937621E-7));
#31786=CARTESIAN_POINT('',(-0.229393975477449,0.00581660464796595,-0.0107320544081557));
#31787=CARTESIAN_POINT('Ctrl Pts',(-0.224906594128032,-0.00157591540674423,
-2.27571033939348E-7));
#31788=CARTESIAN_POINT('Ctrl Pts',(-0.224946111868523,-0.00157529870331805,
-0.000118551128803213));
#31789=CARTESIAN_POINT('Ctrl Pts',(-0.224996629368199,-0.0015735663266729,
-0.000269517258642752));
#31790=CARTESIAN_POINT('Ctrl Pts',(-0.225052344323161,-0.00157067899600388,
-0.000435194557733859));
#31791=CARTESIAN_POINT('Ctrl Pts',(-0.225076556525918,-0.00156927633644708,
-0.000507075806777329));
#31792=CARTESIAN_POINT('Ctrl Pts',(-0.225130207366057,-0.0015656398299004,
-0.000664819935409192));
#31793=CARTESIAN_POINT('Ctrl Pts',(-0.225189841162327,-0.00156078991738676,
-0.000837533395631968));
#31794=CARTESIAN_POINT('Ctrl Pts',(-0.22525653713051,-0.00155462574186823,
-0.00102810784797744));
#31795=CARTESIAN_POINT('Ctrl Pts',(-0.225363879872858,-0.00154285643018889,
-0.00132367096100794));
#31796=CARTESIAN_POINT('Ctrl Pts',(-0.225495863486334,-0.0015265971055308,
-0.00166960190534258));
#31797=CARTESIAN_POINT('Ctrl Pts',(-0.225649782636847,-0.00150521381488585,
-0.00204850589559849));
#31798=CARTESIAN_POINT('Ctrl Pts',(-0.225872675355422,-0.00147720345367394,
-0.00254160361791802));
#31799=CARTESIAN_POINT('Ctrl Pts',(-0.226211629687716,-0.00140171665460475,
-0.00320349500780991));
#31800=CARTESIAN_POINT('Ctrl Pts',(-0.22667852249447,-0.00124920977011111,
-0.00397750653063482));
#31801=CARTESIAN_POINT('Ctrl Pts',(-0.227300714792837,-0.000994842482836054,
-0.00483218755095857));
#31802=CARTESIAN_POINT('Ctrl Pts',(-0.227912194052181,-0.000713115698522522,
-0.00552491953200038));
#31803=CARTESIAN_POINT('Ctrl Pts',(-0.228385701343969,-0.000485499178486317,
-0.00599498793797899));
#31804=CARTESIAN_POINT('Ctrl Pts',(-0.22878733542391,-0.000288437462414136,
-0.00636169114342147));
#31805=CARTESIAN_POINT('Ctrl Pts',(-0.229095506495693,-0.000134908177801581,
-0.00662084785225318));
#31806=CARTESIAN_POINT('Ctrl Pts',(-0.22936465511862,5.49838883985097E-7,
-0.00683645790999942));
#31807=CARTESIAN_POINT('Ctrl Pts',(-0.229591473222452,0.000115907254181684,
-0.00701093248054787));
#31808=CARTESIAN_POINT('Ctrl Pts',(-0.229758410587813,0.000201141186053844,
-0.00713536492284351));
#31809=CARTESIAN_POINT('Ctrl Pts',(-0.230084575118053,0.000369860873483232,
-0.00737136885461296));
#31810=CARTESIAN_POINT('Ctrl Pts',(-0.230320772955051,0.000494986606296006,
-0.00753599937709786));
#31811=CARTESIAN_POINT('Ctrl Pts',(-0.230655165569622,0.000682641774099848,
-0.00776837208130201));
#31812=CARTESIAN_POINT('Ctrl Pts',(-0.230862751346926,0.000807699941341247,
-0.00791571647726933));
#31813=CARTESIAN_POINT('Ctrl Pts',(-0.231060043316746,0.000935072905748187,
-0.00805946248585124));
#31814=CARTESIAN_POINT('Ctrl Pts',(-0.231207688046934,0.00103564097302385,
-0.00816957954198867));
#31815=CARTESIAN_POINT('Ctrl Pts',(-0.231430184389937,0.00120414395145074,
-0.00834535138518368));
#31816=CARTESIAN_POINT('Ctrl Pts',(-0.231579649993422,0.0013299767587557,
-0.00847062997824837));
#31817=CARTESIAN_POINT('Ctrl Pts',(-0.231768906738338,0.00152108066299523,
-0.00865138265776975));
#31818=CARTESIAN_POINT('Ctrl Pts',(-0.231885959839634,0.00167553057426468,
-0.0087894024681425));
#31819=CARTESIAN_POINT('Ctrl Pts',(-0.231994956950233,0.00188925368178171,
-0.00896980965249575));
#31820=CARTESIAN_POINT('Ctrl Pts',(-0.232067192729006,0.0021640031232806,
-0.00918668383711871));
#31821=CARTESIAN_POINT('Ctrl Pts',(-0.232024116308641,0.00249499966508092,
-0.00941975370458247));
#31822=CARTESIAN_POINT('Ctrl Pts',(-0.231920307934533,0.00274915188946458,
-0.00958185777628863));
#31823=CARTESIAN_POINT('Ctrl Pts',(-0.23178568627637,0.00300417566545555,
-0.00973340850727868));
#31824=CARTESIAN_POINT('Ctrl Pts',(-0.231668546496582,0.00319162004613365,
-0.00983699860767679));
#31825=CARTESIAN_POINT('Ctrl Pts',(-0.231502360598737,0.00343046561885037,
-0.00996031520102549));
#31826=CARTESIAN_POINT('Ctrl Pts',(-0.231381050326924,0.00358962237924073,
-0.0100368548962065));
#31827=CARTESIAN_POINT('Ctrl Pts',(-0.231220721639087,0.00379124967224796,
-0.0101287847241368));
#31828=CARTESIAN_POINT('Ctrl Pts',(-0.231053491019977,0.00399213949104106,
-0.010214286829562));
#31829=CARTESIAN_POINT('Ctrl Pts',(-0.230834786572646,0.00424485552231371,
-0.0103123580263811));
#31830=CARTESIAN_POINT('Ctrl Pts',(-0.230710779400135,0.00438412063471161,
-0.010362189532424));
#31831=CARTESIAN_POINT('Ctrl Pts',(-0.230536082718158,0.00457821904778256,
-0.0104284136644632));
#31832=CARTESIAN_POINT('Ctrl Pts',(-0.230376741888428,0.00475273926911148,
-0.0104825778295121));
#31833=CARTESIAN_POINT('Ctrl Pts',(-0.230245352068406,0.00489588458011249,
-0.0105243177957444));
#31834=CARTESIAN_POINT('Ctrl Pts',(-0.230120102425176,0.00503177140546183,
-0.0105614595581269));
#31835=CARTESIAN_POINT('Ctrl Pts',(-0.230072497203735,0.00508324860927118,
-0.010574824436958));
#31836=CARTESIAN_POINT('Ctrl Pts',(-0.229969032924836,0.00519505476708446,
-0.0106033757685201));
#31837=CARTESIAN_POINT('Ctrl Pts',(-0.229775084763404,0.00540432824391078,
-0.0106533278777229));
#31838=CARTESIAN_POINT('Ctrl Pts',(-0.229558050447209,0.00563880049780806,
-0.0107017175610709));
#31839=CARTESIAN_POINT('Ctrl Pts',(-0.229393975477449,0.00581660464796576,
-0.0107320544081557));
#31840=CARTESIAN_POINT('',(-0.228121493224293,0.00414974478032743,-0.0102148629362556));
#31841=CARTESIAN_POINT('Ctrl Pts',(-0.229393975477449,0.00581660464796602,
-0.0107320544081557));
#31842=CARTESIAN_POINT('Ctrl Pts',(-0.229260858960321,0.00565614753223228,
-0.01069838602159));
#31843=CARTESIAN_POINT('Ctrl Pts',(-0.229132855290044,0.00549873829411337,
-0.0106607741833732));
#31844=CARTESIAN_POINT('Ctrl Pts',(-0.229015768989325,0.00535237650556446,
-0.0106221138981469));
#31845=CARTESIAN_POINT('Ctrl Pts',(-0.228898682688606,0.00520601471701555,
-0.0105834536129206));
#31846=CARTESIAN_POINT('Ctrl Pts',(-0.228792501999893,0.00507058293729866,
-0.0105442720151909));
#31847=CARTESIAN_POINT('Ctrl Pts',(-0.228679848627723,0.00492249068197044,
-0.0104974436642677));
#31848=CARTESIAN_POINT('Ctrl Pts',(-0.228567195255553,0.00477439842664221,
-0.0104506153133446));
#31849=CARTESIAN_POINT('Ctrl Pts',(-0.228448084803687,0.00461386570734565,
-0.0103954316370884));
#31850=CARTESIAN_POINT('Ctrl Pts',(-0.228337596129134,0.0044593359696114,
-0.0103374414505981));
#31851=CARTESIAN_POINT('Ctrl Pts',(-0.228282351791858,0.00438207110074427,
-0.010308446357353));
#31852=CARTESIAN_POINT('Ctrl Pts',(-0.228229261601845,0.00430627978839228,
-0.0102788100670567));
#31853=CARTESIAN_POINT('Ctrl Pts',(-0.228179294360642,0.00423396073728532,
-0.0102494906607338));
#31854=CARTESIAN_POINT('Ctrl Pts',(-0.228159733383576,0.0042056495624831,
-0.0102380128160331));
#31855=CARTESIAN_POINT('Ctrl Pts',(-0.228140650513694,0.00417786961955901,
-0.0102265896495175));
#31856=CARTESIAN_POINT('Ctrl Pts',(-0.228121493224293,0.00414974478032743,
-0.0102148629362556));
#31857=CARTESIAN_POINT('',(-0.227485893353239,0.00309654395920274,-0.00969559727848083));
#31858=CARTESIAN_POINT('Ctrl Pts',(-0.228121493224293,0.00414974478032743,
-0.0102148629362556));
#31859=CARTESIAN_POINT('Ctrl Pts',(-0.228091714466324,0.00410602655052453,
-0.0101966345246728));
#31860=CARTESIAN_POINT('Ctrl Pts',(-0.228061755890881,0.00406146956532859,
-0.0101776840835163));
#31861=CARTESIAN_POINT('Ctrl Pts',(-0.228029542246017,0.00401285950391605,
-0.010156492775014));
#31862=CARTESIAN_POINT('Ctrl Pts',(-0.227976604898777,0.00393297758706865,
-0.0101216686605307));
#31863=CARTESIAN_POINT('Ctrl Pts',(-0.227917584474054,0.00384224359990983,
-0.0100805623915113));
#31864=CARTESIAN_POINT('Ctrl Pts',(-0.227864344213728,0.00375821752094305,
-0.0100408730610387));
#31865=CARTESIAN_POINT('Ctrl Pts',(-0.227811103953402,0.00367419144197628,
-0.0100011837305661));
#31866=CARTESIAN_POINT('Ctrl Pts',(-0.227763638776,0.00359676247856459,
-0.00996314948809607));
#31867=CARTESIAN_POINT('Ctrl Pts',(-0.227718266368965,0.00352005373481683,
-0.00992422989423481));
#31868=CARTESIAN_POINT('Ctrl Pts',(-0.227672893961929,0.00344334499106908,
-0.00988531030037355));
#31869=CARTESIAN_POINT('Ctrl Pts',(-0.227629616652783,0.00336741097886024,
-0.00984539544653163));
#31870=CARTESIAN_POINT('Ctrl Pts',(-0.227591308711727,0.00329798459064695,
-0.00980781213905574));
#31871=CARTESIAN_POINT('Ctrl Pts',(-0.227553856941985,0.00323010986196881,
-0.00977106880754444));
#31872=CARTESIAN_POINT('Ctrl Pts',(-0.227521150813476,0.00316835468101453,
-0.00973674788899397));
#31873=CARTESIAN_POINT('Ctrl Pts',(-0.227485893353239,0.00309654395920274,
-0.00969559727848083));
#31874=CARTESIAN_POINT('',(-0.227126281777643,0.00216860537756898,-0.00908887068682453));
#31875=CARTESIAN_POINT('Ctrl Pts',(-0.227485893353239,0.00309654395920274,
-0.00969559727848083));
#31876=CARTESIAN_POINT('Ctrl Pts',(-0.227485087345238,0.00309490218844343,
-0.00969465677495352));
#31877=CARTESIAN_POINT('Ctrl Pts',(-0.227484280003889,0.0030932552914689,
-0.00969371248168514));
#31878=CARTESIAN_POINT('Ctrl Pts',(-0.227483471242014,0.00309160294606555,
-0.00969276450874163));
#31879=CARTESIAN_POINT('Ctrl Pts',(-0.227447284556303,0.00301767153853937,
-0.00965034905863751));
#31880=CARTESIAN_POINT('Ctrl Pts',(-0.227408261758414,0.00293304001203312,
-0.00960019540130323));
#31881=CARTESIAN_POINT('Ctrl Pts',(-0.227376939924427,0.00285973054341183,
-0.0095553277649556));
#31882=CARTESIAN_POINT('Ctrl Pts',(-0.227361279007434,0.00282307580910118,
-0.00953289394678179));
#31883=CARTESIAN_POINT('Ctrl Pts',(-0.227347541293956,0.00278919165650028,
-0.00951188095760037));
#31884=CARTESIAN_POINT('Ctrl Pts',(-0.227331697400134,0.00274851693980081,
-0.00948621499946682));
#31885=CARTESIAN_POINT('Ctrl Pts',(-0.227315853506312,0.00270784222310134,
-0.00946054904133327));
#31886=CARTESIAN_POINT('Ctrl Pts',(-0.227297906689983,0.0026604761335986,
-0.00943007037660862));
#31887=CARTESIAN_POINT('Ctrl Pts',(-0.22728557185282,0.0026273161128947,
-0.00940842406727091));
#31888=CARTESIAN_POINT('Ctrl Pts',(-0.227273237015657,0.00259415609219081,
-0.00938677775793319));
#31889=CARTESIAN_POINT('Ctrl Pts',(-0.227266510364656,0.00257508000662186,
-0.00937415162267746));
#31890=CARTESIAN_POINT('Ctrl Pts',(-0.227256761271677,0.00254726774721839,
-0.0093555911838289));
#31891=CARTESIAN_POINT('Ctrl Pts',(-0.227247012178699,0.00251945548781492,
-0.00933703074498034));
#31892=CARTESIAN_POINT('Ctrl Pts',(-0.22723424257423,0.0024829710433869,
-0.00931243989623622));
#31893=CARTESIAN_POINT('Ctrl Pts',(-0.227220609376841,0.00244362879544726,
-0.00928540540934555));
#31894=CARTESIAN_POINT('Ctrl Pts',(-0.227193343013809,0.00236494439117793,
-0.00923133649851507));
#31895=CARTESIAN_POINT('Ctrl Pts',(-0.227162618503677,0.00227469484764093,
-0.00916768385327356));
#31896=CARTESIAN_POINT('Ctrl Pts',(-0.227126281773003,0.00216860010539621,
-0.00908887778676522));
#31897=CARTESIAN_POINT('',(-0.226399236752868,0.00218270468350247,-0.00908497199103554));
#31898=CARTESIAN_POINT('Ctrl Pts',(-0.226399237323331,0.00218270481409039,
-0.00908497209528306));
#31899=CARTESIAN_POINT('Ctrl Pts',(-0.226402015621168,0.00218242237783528,
-0.00908481942012229));
#31900=CARTESIAN_POINT('Ctrl Pts',(-0.226426871610067,0.0021791724381742,
-0.00908292829527202));
#31901=CARTESIAN_POINT('Ctrl Pts',(-0.226650682773869,0.00216138573969967,
-0.00907425334358046));
#31902=CARTESIAN_POINT('Ctrl Pts',(-0.226703737969127,0.0021601993779741,
-0.00907442059635822));
#31903=CARTESIAN_POINT('Ctrl Pts',(-0.2268930731039,0.00216094231513602,
-0.00907868413393107));
#31904=CARTESIAN_POINT('Ctrl Pts',(-0.226966948755117,0.00216362473656388,
-0.00908207388280154));
#31905=CARTESIAN_POINT('Ctrl Pts',(-0.22707003478252,0.00216671281664232,
-0.00908640974873301));
#31906=CARTESIAN_POINT('Ctrl Pts',(-0.227126282004474,0.00216861511471869,
-0.00908885732195361));
#31907=CARTESIAN_POINT('',(-0.22652065327516,0.00174024863118734,-0.00874177656924924));
#31908=CARTESIAN_POINT('Origin',(-0.228263370666261,0.00775028046455406,
-0.00208932932211252));
#31909=CARTESIAN_POINT('',(-0.225316604397604,0.00173833991161196,-0.00871757580529813));
#31910=CARTESIAN_POINT('',(-0.225316604396809,0.00173833991161069,-0.00871757580528216));
#31911=CARTESIAN_POINT('',(-0.225202513398594,0.00215390640396955,-0.00904067530421461));
#31912=CARTESIAN_POINT('Origin',(-0.226677373856487,0.00780210962717219,
-0.00184344636966992));
#31913=CARTESIAN_POINT('',(-0.224906358055501,0.00215779401747845,-0.00903767194051428));
#31914=CARTESIAN_POINT('Ctrl Pts',(-0.224906358055501,0.00215779401747845,
-0.00903767194051428));
#31915=CARTESIAN_POINT('Ctrl Pts',(-0.224965738450647,0.00215287276425,
-0.00903547806035347));
#31916=CARTESIAN_POINT('Ctrl Pts',(-0.225032844119037,0.00215141623484859,
-0.00903399244325265));
#31917=CARTESIAN_POINT('Ctrl Pts',(-0.225088313767917,0.00215087702492171,
-0.00903517782487992));
#31918=CARTESIAN_POINT('Ctrl Pts',(-0.225147134576941,0.00215030523900321,
-0.00903643482051134));
#31919=CARTESIAN_POINT('Ctrl Pts',(-0.225192860176731,0.0021516122887076,
-0.0090388265130241));
#31920=CARTESIAN_POINT('Ctrl Pts',(-0.225202513203785,0.00215390610473247,
-0.00904067508301585));
#31921=CARTESIAN_POINT('',(-0.224895681452505,0.00215874544783754,-0.00903810107358197));
#31922=CARTESIAN_POINT('Ctrl Pts',(-0.224895681757744,0.00215874503503595,
-0.00903810076696465));
#31923=CARTESIAN_POINT('Ctrl Pts',(-0.224899208684984,0.00215842069526572,
-0.00903796212742679));
#31924=CARTESIAN_POINT('Ctrl Pts',(-0.224902768068525,0.00215810962985243,
-0.00903782571768279));
#31925=CARTESIAN_POINT('Ctrl Pts',(-0.224906358055501,0.00215779401747845,
-0.00903767194051428));
#31926=CARTESIAN_POINT('',(-0.224918679572961,0.00225276421039843,-0.00910663697272384));
#31927=CARTESIAN_POINT('Ctrl Pts',(-0.224918679572961,0.00225276421039843,
-0.00910663697272384));
#31928=CARTESIAN_POINT('Ctrl Pts',(-0.224910263452399,0.00221796952208274,
-0.00908158964469767));
#31929=CARTESIAN_POINT('Ctrl Pts',(-0.224903043299005,0.00218876974680351,
-0.0090602399920936));
#31930=CARTESIAN_POINT('Ctrl Pts',(-0.224895680110049,0.00215877571930383,
-0.00903806209673358));
#31931=CARTESIAN_POINT('',(-0.22502122058335,0.00297339373605577,-0.00957419677215159));
#31932=CARTESIAN_POINT('Ctrl Pts',(-0.225021220587936,0.00297339370675859,
-0.00957419675522714));
#31933=CARTESIAN_POINT('Ctrl Pts',(-0.225018822681216,0.00292404131059288,
-0.00954547825756419));
#31934=CARTESIAN_POINT('Ctrl Pts',(-0.225015786101244,0.00284658987129514,
-0.00949966911370489));
#31935=CARTESIAN_POINT('Ctrl Pts',(-0.225008834761646,0.00276240820049218,
-0.00944752370527374));
#31936=CARTESIAN_POINT('Ctrl Pts',(-0.225005359091848,0.00272031736509071,
-0.00942145100105817));
#31937=CARTESIAN_POINT('Ctrl Pts',(-0.225000905055243,0.00267655359290298,
-0.00939377841014082));
#31938=CARTESIAN_POINT('Ctrl Pts',(-0.224996511017835,0.00264085188948549,
-0.00937084674685504));
#31939=CARTESIAN_POINT('Ctrl Pts',(-0.224992116980427,0.00260515018606799,
-0.00934791508356925));
#31940=CARTESIAN_POINT('Ctrl Pts',(-0.224987781650824,0.00257746907246234,
-0.00932978843303144));
#31941=CARTESIAN_POINT('Ctrl Pts',(-0.22498421438809,0.00255588184289646,
-0.00931556310125919));
#31942=CARTESIAN_POINT('Ctrl Pts',(-0.224982430756723,0.00254508822811351,
-0.00930845043537307));
#31943=CARTESIAN_POINT('Ctrl Pts',(-0.224980838910431,0.00253581068869719,
-0.00930232458184892));
#31944=CARTESIAN_POINT('Ctrl Pts',(-0.224977703366424,0.00251896760981262,
-0.00929110098797916));
#31945=CARTESIAN_POINT('Ctrl Pts',(-0.224974567822417,0.00250212453092805,
-0.00927987739410941));
#31946=CARTESIAN_POINT('Ctrl Pts',(-0.22496988938007,0.00247774239373384,
-0.00926351615899424));
#31947=CARTESIAN_POINT('Ctrl Pts',(-0.224965165668848,0.00245478699071914,
-0.00924792855998076));
#31948=CARTESIAN_POINT('Ctrl Pts',(-0.224960441957625,0.00243183158770443,
-0.00923234096096728));
#31949=CARTESIAN_POINT('Ctrl Pts',(-0.224955672693692,0.00241029291869914,
-0.00921754133956075));
#31950=CARTESIAN_POINT('Ctrl Pts',(-0.22495211515215,0.00239447540665665,
-0.0092066089723048));
#31951=CARTESIAN_POINT('Ctrl Pts',(-0.224948557610609,0.00237865789461416,
-0.00919567660504884));
#31952=CARTESIAN_POINT('Ctrl Pts',(-0.224946211283118,0.00236854422866547,
-0.00918863700259461));
#31953=CARTESIAN_POINT('Ctrl Pts',(-0.224943044205686,0.0023550400623941,
-0.00917919588349946));
#31954=CARTESIAN_POINT('Ctrl Pts',(-0.224936710050824,0.00232803172985139,
-0.00916031364530917));
#31955=CARTESIAN_POINT('Ctrl Pts',(-0.224927095693523,0.00228755889871412,
-0.00913168430075001));
#31956=CARTESIAN_POINT('Ctrl Pts',(-0.224918679572961,0.00225276421039843,
-0.00910663697272384));
#31957=CARTESIAN_POINT('',(-0.224873561887543,0.00458479712506902,-0.0103057155136081));
#31958=CARTESIAN_POINT('Ctrl Pts',(-0.22502122058335,0.00297339373605577,
-0.00957419677215159));
#31959=CARTESIAN_POINT('Ctrl Pts',(-0.224994800587243,0.00312706788500571,
-0.00966292275481428));
#31960=CARTESIAN_POINT('Ctrl Pts',(-0.224971751786512,0.00328898460622665,
-0.00975067902641553));
#31961=CARTESIAN_POINT('Ctrl Pts',(-0.224951688553439,0.00346762396572364,
-0.00983967477566947));
#31962=CARTESIAN_POINT('Ctrl Pts',(-0.224931625320365,0.00364626332522062,
-0.00992867052492342));
#31963=CARTESIAN_POINT('Ctrl Pts',(-0.22491456271264,0.00384201360972133,
-0.0100181849127952));
#31964=CARTESIAN_POINT('Ctrl Pts',(-0.22490161244035,0.00403033493817414,
-0.0100964406799755));
#31965=CARTESIAN_POINT('Ctrl Pts',(-0.22489853339978,0.00407510998209125,
-0.010115046673471));
#31966=CARTESIAN_POINT('Ctrl Pts',(-0.224895685788583,0.00411945175020758,
-0.0101330494887832));
#31967=CARTESIAN_POINT('Ctrl Pts',(-0.224893049692661,0.00416352534378688,
-0.0101505428737757));
#31968=CARTESIAN_POINT('Ctrl Pts',(-0.224884598516693,0.00430482281780293,
-0.0102066256868774));
#31969=CARTESIAN_POINT('Ctrl Pts',(-0.224878321311043,0.00444332778718251,
-0.0102575634943944));
#31970=CARTESIAN_POINT('Ctrl Pts',(-0.224873561887543,0.00458479712506902,
-0.0103057155136081));
#31971=CARTESIAN_POINT('',(-0.224989661033144,0.00750493775356048,-0.010792594548104));
#31972=CARTESIAN_POINT('Ctrl Pts',(-0.224873561887543,0.00458479712506902,
-0.0103057155136081));
#31973=CARTESIAN_POINT('Ctrl Pts',(-0.224867317901785,0.00477039366441729,
-0.0103688871397866));
#31974=CARTESIAN_POINT('Ctrl Pts',(-0.224863695490022,0.00496116495721837,
-0.0104269636390426));
#31975=CARTESIAN_POINT('Ctrl Pts',(-0.224863318658598,0.00515133401433211,
-0.0104781654954328));
#31976=CARTESIAN_POINT('Ctrl Pts',(-0.224862941827173,0.00534150307144586,
-0.010529367351823));
#31977=CARTESIAN_POINT('Ctrl Pts',(-0.224865806202762,0.00553104234508341,
-0.0105738883450165));
#31978=CARTESIAN_POINT('Ctrl Pts',(-0.224871561595658,0.00572270826827539,
-0.0106125334130875));
#31979=CARTESIAN_POINT('Ctrl Pts',(-0.224874439292107,0.00581854122987138,
-0.010631855947123));
#31980=CARTESIAN_POINT('Ctrl Pts',(-0.224878038558442,0.00591488770775002,
-0.010649763323073));
#31981=CARTESIAN_POINT('Ctrl Pts',(-0.224882845453478,0.00601827962750455,
-0.0106671096183221));
#31982=CARTESIAN_POINT('Ctrl Pts',(-0.224887652348514,0.00612167154725909,
-0.0106844559135711));
#31983=CARTESIAN_POINT('Ctrl Pts',(-0.224893675898609,0.00623218238819598,
-0.010700838010295));
#31984=CARTESIAN_POINT('Ctrl Pts',(-0.224898904237491,0.00632012556458434,
-0.0107125924563936));
#31985=CARTESIAN_POINT('Ctrl Pts',(-0.224904132576373,0.0064080687409727,
-0.0107243469024922));
#31986=CARTESIAN_POINT('Ctrl Pts',(-0.224908551189283,0.00647336006007754,
-0.0107321190251052));
#31987=CARTESIAN_POINT('Ctrl Pts',(-0.224914213769459,0.00655341180453011,
-0.0107407320671868));
#31988=CARTESIAN_POINT('Ctrl Pts',(-0.224919876349636,0.00663346354898268,
-0.0107493451092684));
#31989=CARTESIAN_POINT('Ctrl Pts',(-0.224926791877645,0.00672831496636562,
-0.0107584006712993));
#31990=CARTESIAN_POINT('Ctrl Pts',(-0.22493444307939,0.00682862505175741,
-0.0107661102157719));
#31991=CARTESIAN_POINT('Ctrl Pts',(-0.224949745482882,0.00702924522254099,
-0.010781529304717));
#31992=CARTESIAN_POINT('Ctrl Pts',(-0.224967975196583,0.00725167285755061,
-0.0107922449054418));
#31993=CARTESIAN_POINT('Ctrl Pts',(-0.224989661033144,0.00750493775356048,
-0.010792594548104));
#31994=CARTESIAN_POINT('',(-0.224861052242961,0.00980960902579858,-0.0104885393712655));
#31995=CARTESIAN_POINT('Ctrl Pts',(-0.224989619839449,0.00750541590997777,
-0.0107925933390392));
#31996=CARTESIAN_POINT('Ctrl Pts',(-0.224968308830846,0.00775278936281719,
-0.0107919616726235));
#31997=CARTESIAN_POINT('Ctrl Pts',(-0.224950341443786,0.00797012061575864,
-0.0107814799560685));
#31998=CARTESIAN_POINT('Ctrl Pts',(-0.224935172802778,0.00816640892122435,
-0.0107664984290652));
#31999=CARTESIAN_POINT('Ctrl Pts',(-0.224927583595994,0.00826461630437055,
-0.0107590028395596));
#32000=CARTESIAN_POINT('Ctrl Pts',(-0.224920698710054,0.00835754960891373,
-0.0107502157304149));
#32001=CARTESIAN_POINT('Ctrl Pts',(-0.224915052876814,0.00843590726060768,
-0.010741876735001));
#32002=CARTESIAN_POINT('Ctrl Pts',(-0.224909407043574,0.00851426491230164,
-0.0107335377395871));
#32003=CARTESIAN_POINT('Ctrl Pts',(-0.224904991495846,0.00857808469234472,
-0.0107260357632222));
#32004=CARTESIAN_POINT('Ctrl Pts',(-0.22489968241033,0.00866461685109938,
-0.0107146156992334));
#32005=CARTESIAN_POINT('Ctrl Pts',(-0.224894373324813,0.00875114900985405,
-0.0107031956352445));
#32006=CARTESIAN_POINT('Ctrl Pts',(-0.224888185038604,0.00886031180744275,
-0.0106872201606962));
#32007=CARTESIAN_POINT('Ctrl Pts',(-0.224883184114701,0.00896206883700661,
-0.0106703715492553));
#32008=CARTESIAN_POINT('Ctrl Pts',(-0.224878183190799,0.00906382586657046,
-0.0106535229378145));
#32009=CARTESIAN_POINT('Ctrl Pts',(-0.224874360588758,0.00915824882136895,
-0.0106362047479502));
#32010=CARTESIAN_POINT('Ctrl Pts',(-0.224871246701787,0.00925206036384027,
-0.0106175595945488));
#32011=CARTESIAN_POINT('Ctrl Pts',(-0.224865018927847,0.00943968344878292,
-0.010580269287746));
#32012=CARTESIAN_POINT('Ctrl Pts',(-0.224861631620231,0.00962479695162405,
-0.010537419086996));
#32013=CARTESIAN_POINT('Ctrl Pts',(-0.224861054524101,0.00980887667976263,
-0.0104887330969168));
#32014=CARTESIAN_POINT('',(-0.225003674467847,0.0119594514142438,-0.00961246062240638));
#32015=CARTESIAN_POINT('Ctrl Pts',(-0.224861052242961,0.00980960902579858,
-0.0104885393712655));
#32016=CARTESIAN_POINT('Ctrl Pts',(-0.224859994130178,0.0101515267552638,
-0.0103980785545349));
#32017=CARTESIAN_POINT('Ctrl Pts',(-0.22486861966081,0.0104899749483281,
-0.0102879912445166));
#32018=CARTESIAN_POINT('Ctrl Pts',(-0.224888950367126,0.0108364571580695,
-0.0101504612032825));
#32019=CARTESIAN_POINT('Ctrl Pts',(-0.224890495888814,0.0108627964185675,
-0.0101400062954098));
#32020=CARTESIAN_POINT('Ctrl Pts',(-0.224892109053557,0.0108891803588371,
-0.0101293892361149));
#32021=CARTESIAN_POINT('Ctrl Pts',(-0.224893790749427,0.01091561328614,
-0.0101186052814899));
#32022=CARTESIAN_POINT('Ctrl Pts',(-0.22490570050544,0.0111028110550533,
-0.0100422334055061));
#32023=CARTESIAN_POINT('Ctrl Pts',(-0.224921059623722,0.0112923339255128,
-0.00995711388322306));
#32024=CARTESIAN_POINT('Ctrl Pts',(-0.224939425953085,0.0114679404137457,
-0.0098713483279965));
#32025=CARTESIAN_POINT('Ctrl Pts',(-0.224957792282447,0.0116435469019786,
-0.00978558277276994));
#32026=CARTESIAN_POINT('Ctrl Pts',(-0.224979156068591,0.0118054886917652,
-0.00969963800962885));
#32027=CARTESIAN_POINT('Ctrl Pts',(-0.225003674449545,0.0119594518698436,
-0.00961246147151369));
#32028=CARTESIAN_POINT('',(-0.22485135503735,0.0128342630404597,-0.00904243198075601));
#32029=CARTESIAN_POINT('Ctrl Pts',(-0.224851353464631,0.0128342017223001,
-0.00904235060666903));
#32030=CARTESIAN_POINT('Ctrl Pts',(-0.22485925916006,0.0128021299727841,
-0.00906601576353804));
#32031=CARTESIAN_POINT('Ctrl Pts',(-0.224867008714604,0.0127708336008954,
-0.00908883359846289));
#32032=CARTESIAN_POINT('Ctrl Pts',(-0.224876088403718,0.0127334705285249,
-0.00911562313894002));
#32033=CARTESIAN_POINT('Ctrl Pts',(-0.224885168862013,0.0126961042909622,
-0.00914241494887834));
#32034=CARTESIAN_POINT('Ctrl Pts',(-0.224895582294414,0.0126525747563171,
-0.00917304599903577));
#32035=CARTESIAN_POINT('Ctrl Pts',(-0.224902470444808,0.0126234398800092,
-0.00919329013210234));
#32036=CARTESIAN_POINT('Ctrl Pts',(-0.224905914520005,0.0126088724418552,
-0.00920341219863562));
#32037=CARTESIAN_POINT('Ctrl Pts',(-0.224908476469182,0.0125979315046998,
-0.00921097808108285));
#32038=CARTESIAN_POINT('Ctrl Pts',(-0.224912358910093,0.0125809508958258,
-0.00922263290293978));
#32039=CARTESIAN_POINT('Ctrl Pts',(-0.224916241351003,0.0125639702869518,
-0.00923428772479671));
#32040=CARTESIAN_POINT('Ctrl Pts',(-0.22492144485436,0.0125409307741997,
-0.00925000290292928));
#32041=CARTESIAN_POINT('Ctrl Pts',(-0.22492671945306,0.0125162396970512,
-0.00926663390298052));
#32042=CARTESIAN_POINT('Ctrl Pts',(-0.224931994051759,0.0124915486199026,
-0.00928326490303176));
#32043=CARTESIAN_POINT('Ctrl Pts',(-0.224937340105205,0.0124651934712332,
-0.00930079361002119));
#32044=CARTESIAN_POINT('Ctrl Pts',(-0.224940932961824,0.0124470857933336,
-0.00931274715591608));
#32045=CARTESIAN_POINT('Ctrl Pts',(-0.224944525818442,0.012428978115434,
-0.00932470070181097));
#32046=CARTESIAN_POINT('Ctrl Pts',(-0.224946364530775,0.0124191489015504,
-0.00933112626801354));
#32047=CARTESIAN_POINT('Ctrl Pts',(-0.224948466183687,0.0124076180730514,
-0.0093386492942931));
#32048=CARTESIAN_POINT('Ctrl Pts',(-0.224952669489511,0.0123845564160533,
-0.00935369534685221));
#32049=CARTESIAN_POINT('Ctrl Pts',(-0.224957925683046,0.0123546528503569,
-0.00937307558661003));
#32050=CARTESIAN_POINT('Ctrl Pts',(-0.22496368028001,0.0123163102277348,
-0.00939742191162186));
#32051=CARTESIAN_POINT('Ctrl Pts',(-0.224969434876974,0.0122779676051128,
-0.0094217682366337));
#32052=CARTESIAN_POINT('Ctrl Pts',(-0.224975689291671,0.0122311411163537,
-0.0094510106343654));
#32053=CARTESIAN_POINT('Ctrl Pts',(-0.224981041882397,0.0121859897564173,
-0.00947859648540025));
#32054=CARTESIAN_POINT('Ctrl Pts',(-0.22499174706385,0.0120956870365444,
-0.00953376818746994));
#32055=CARTESIAN_POINT('Ctrl Pts',(-0.224998843833919,0.0120121173691427,
-0.00958236813765755));
#32056=CARTESIAN_POINT('Ctrl Pts',(-0.225003674451785,0.0119594518981984,
-0.00961246145541169));
#32057=CARTESIAN_POINT('',(-0.225189992040237,0.012835362403236,-0.00904829323284222));
#32058=CARTESIAN_POINT('Ctrl Pts',(-0.225189991984345,0.0128353624762501,
-0.00904829317995413));
#32059=CARTESIAN_POINT('Ctrl Pts',(-0.225177557949143,0.0128382138898305,
-0.00904599628478506));
#32060=CARTESIAN_POINT('Ctrl Pts',(-0.225123424484218,0.0128399799233524,
-0.00904304785851361));
#32061=CARTESIAN_POINT('Ctrl Pts',(-0.225057128079432,0.0128399711268489,
-0.00904126425642094));
#32062=CARTESIAN_POINT('Ctrl Pts',(-0.224990831901919,0.0128399623303756,
-0.00903948066044271));
#32063=CARTESIAN_POINT('Ctrl Pts',(-0.224912370630193,0.0128387738011947,
-0.00904015806168038));
#32064=CARTESIAN_POINT('Ctrl Pts',(-0.224851352869637,0.0128342685710829,
-0.00904242811423944));
#32065=CARTESIAN_POINT('',(-0.225309783756647,0.0132780506578484,-0.00870378498324709));
#32066=CARTESIAN_POINT('Ctrl Pts',(-0.225309747301439,0.0132780497391535,
-0.00870378504917953));
#32067=CARTESIAN_POINT('Ctrl Pts',(-0.225296300432129,0.0132302881562321,
-0.0087433986075426));
#32068=CARTESIAN_POINT('Ctrl Pts',(-0.225278030237819,0.0131658512022134,
-0.00879661521430529));
#32069=CARTESIAN_POINT('Ctrl Pts',(-0.225249280048583,0.0130594725678051,
-0.00887935672594214));
#32070=CARTESIAN_POINT('Ctrl Pts',(-0.225234904953965,0.013006283250601,
-0.00892072748176057));
#32071=CARTESIAN_POINT('Ctrl Pts',(-0.225217916472581,0.0129423241724453,
-0.00896912175258144));
#32072=CARTESIAN_POINT('Ctrl Pts',(-0.225207088659046,0.0129010582597847,
-0.00899977330256321));
#32073=CARTESIAN_POINT('Ctrl Pts',(-0.225196260845511,0.012859792347124,
-0.00903042485254499));
#32074=CARTESIAN_POINT('Ctrl Pts',(-0.225191586980628,0.012841462054515,
-0.00904366530876166));
#32075=CARTESIAN_POINT('Ctrl Pts',(-0.22518999470407,0.0128352773201681,
-0.00904817273968199));
#32076=CARTESIAN_POINT('',(-0.226513610415091,0.0132774514495838,-0.0087268701182885));
#32077=CARTESIAN_POINT('',(-0.226513587963189,0.0132774837566105,-0.00872685128052572));
#32078=CARTESIAN_POINT('',(-0.226387839413824,0.0128159440895836,-0.00908574126323817));
#32079=CARTESIAN_POINT('Origin',(-0.227813772544845,0.00720553420671457,
-0.00186973940970176));
#32080=CARTESIAN_POINT('',(-0.227080811026755,0.0128302386724515,-0.00908882599726657));
#32081=CARTESIAN_POINT('Ctrl Pts',(-0.227080576518632,0.0128308674881957,
-0.00908834620576183));
#32082=CARTESIAN_POINT('Ctrl Pts',(-0.226974397707285,0.012833937009542,
-0.00908410442899972));
#32083=CARTESIAN_POINT('Ctrl Pts',(-0.226856526383581,0.0128356891942227,
-0.00908035969467839));
#32084=CARTESIAN_POINT('Ctrl Pts',(-0.22673763939975,0.0128339634601437,
-0.00907931775934973));
#32085=CARTESIAN_POINT('Ctrl Pts',(-0.226618752415919,0.0128322377260647,
-0.00907827582402107));
#32086=CARTESIAN_POINT('Ctrl Pts',(-0.226498852018804,0.0128269680083964,
-0.00907983666977414));
#32087=CARTESIAN_POINT('Ctrl Pts',(-0.226388621137425,0.012815771215702,
-0.00908588121603269));
#32088=CARTESIAN_POINT('',(-0.229388968164796,0.00914967754123552,-0.0107383249628337));
#32089=CARTESIAN_POINT('Ctrl Pts',(-0.227080816141077,0.0128302296664822,
-0.00908884892398524));
#32090=CARTESIAN_POINT('Ctrl Pts',(-0.227118042045205,0.0127291087233939,
-0.0091639799482189));
#32091=CARTESIAN_POINT('Ctrl Pts',(-0.227166371368342,0.0125968433379446,
-0.009257729975268));
#32092=CARTESIAN_POINT('Ctrl Pts',(-0.227221508256631,0.0124478282471741,
-0.00935830862716436));
#32093=CARTESIAN_POINT('Ctrl Pts',(-0.227246597063904,0.01238023390187,
-0.00940311751157318));
#32094=CARTESIAN_POINT('Ctrl Pts',(-0.227301913293252,0.0122375017599441,
-0.00949488477515939));
#32095=CARTESIAN_POINT('Ctrl Pts',(-0.22736642320277,0.0120811836283352,
-0.00959127878264262));
#32096=CARTESIAN_POINT('Ctrl Pts',(-0.227484064229483,0.0118170422191122,
-0.00974673980499964));
#32097=CARTESIAN_POINT('Ctrl Pts',(-0.227636777896552,0.0115356572943751,
-0.00989754184678776));
#32098=CARTESIAN_POINT('Ctrl Pts',(-0.227828855086766,0.0112221796454634,
-0.0100508460071324));
#32099=CARTESIAN_POINT('Ctrl Pts',(-0.228009339223509,0.0109504965145836,
-0.0101726617716261));
#32100=CARTESIAN_POINT('Ctrl Pts',(-0.228139625684295,0.0107643904939703,
-0.0102501751694497));
#32101=CARTESIAN_POINT('Ctrl Pts',(-0.228304573361481,0.0105360288702207,
-0.0103394978935565));
#32102=CARTESIAN_POINT('Ctrl Pts',(-0.228472261507887,0.0103111456105014,
-0.0104209620829437));
#32103=CARTESIAN_POINT('Ctrl Pts',(-0.228685514219872,0.0100334503409072,
-0.0105116594987286));
#32104=CARTESIAN_POINT('Ctrl Pts',(-0.228804955859185,0.00988138379631196,
-0.010557077979536));
#32105=CARTESIAN_POINT('Ctrl Pts',(-0.229037084164035,0.0095881542493913,
-0.0106396138852661));
#32106=CARTESIAN_POINT('Ctrl Pts',(-0.22923748765341,0.0093381851229799,
-0.0106996220901668));
#32107=CARTESIAN_POINT('Ctrl Pts',(-0.229388968164794,0.00914967754123375,
-0.010738324962834));
#32108=CARTESIAN_POINT('',(-0.224906163263034,0.0165759221188024,-4.45014041372842E-7));
#32109=CARTESIAN_POINT('Ctrl Pts',(-0.229388968164796,0.00914967754123552,
-0.0107383249628337));
#32110=CARTESIAN_POINT('Ctrl Pts',(-0.229564104670247,0.00934079850670889,
-0.010706443305865));
#32111=CARTESIAN_POINT('Ctrl Pts',(-0.229713942021003,0.00950375582513596,
-0.0106729165575947));
#32112=CARTESIAN_POINT('Ctrl Pts',(-0.22983517785877,0.00963556162626185,
-0.0106432950332153));
#32113=CARTESIAN_POINT('Ctrl Pts',(-0.229895795777654,0.00970146452682479,
-0.0106284842710256));
#32114=CARTESIAN_POINT('Ctrl Pts',(-0.229949263009114,0.00975958209528396,
-0.0106146636081862));
#32115=CARTESIAN_POINT('Ctrl Pts',(-0.229998882838972,0.009813654019032,
-0.0106013255935172));
#32116=CARTESIAN_POINT('Ctrl Pts',(-0.230023692753901,0.00984068998090601,
-0.0105946565861827));
#32117=CARTESIAN_POINT('Ctrl Pts',(-0.230047541270744,0.00986670929317547,
-0.0105880878678036));
#32118=CARTESIAN_POINT('Ctrl Pts',(-0.230065885362377,0.00988671999043132,
-0.0105829693501056));
#32119=CARTESIAN_POINT('Ctrl Pts',(-0.23008422945401,0.00990673068768717,
-0.0105778508324077));
#32120=CARTESIAN_POINT('Ctrl Pts',(-0.23009706777556,0.0099207493068319,
-0.010574243222264));
#32121=CARTESIAN_POINT('Ctrl Pts',(-0.230122987907983,0.00994921599646166,
-0.0105667347448726));
#32122=CARTESIAN_POINT('Ctrl Pts',(-0.230148908040407,0.00997768268609141,
-0.0105592262674811));
#32123=CARTESIAN_POINT('Ctrl Pts',(-0.230187912816546,0.0100205614301913,
-0.0105476888864162));
#32124=CARTESIAN_POINT('Ctrl Pts',(-0.230222885609791,0.0100590946893514,
-0.0105369864609402));
#32125=CARTESIAN_POINT('Ctrl Pts',(-0.230257858403037,0.0100976279485115,
-0.0105262840354641));
#32126=CARTESIAN_POINT('Ctrl Pts',(-0.230288797031605,0.0101318456076922,
-0.0105165154836512));
#32127=CARTESIAN_POINT('Ctrl Pts',(-0.230319797319392,0.0101662100052759,
-0.0105064944662422));
#32128=CARTESIAN_POINT('Ctrl Pts',(-0.230381797894966,0.0102349388004433,
-0.010486452431424));
#32129=CARTESIAN_POINT('Ctrl Pts',(-0.2304440470754,0.0103042237496369,
-0.0104653107292336));
#32130=CARTESIAN_POINT('Ctrl Pts',(-0.230504662761974,0.0103721813001915,
-0.0104436457352738));
#32131=CARTESIAN_POINT('Ctrl Pts',(-0.230565278448548,0.0104401388507461,
-0.0104219807413139));
#32132=CARTESIAN_POINT('Ctrl Pts',(-0.230624261164103,0.0105067646109838,
-0.010399769209469));
#32133=CARTESIAN_POINT('Ctrl Pts',(-0.23067758423573,0.0105672084133487,
-0.0103788991236485));
#32134=CARTESIAN_POINT('Ctrl Pts',(-0.230730907307356,0.0106276522157137,
-0.0103580290378279));
#32135=CARTESIAN_POINT('Ctrl Pts',(-0.230778566444075,0.0106819821383055,
-0.0103386963744288));
#32136=CARTESIAN_POINT('Ctrl Pts',(-0.230838561740658,0.0107513942951081,
-0.0103129298682109));
#32137=CARTESIAN_POINT('Ctrl Pts',(-0.230868153891086,0.0107856312287117,
-0.010300220766474));
#32138=CARTESIAN_POINT('Ctrl Pts',(-0.230900749272715,0.0108235170458618,
-0.0102858937333083));
#32139=CARTESIAN_POINT('Ctrl Pts',(-0.230933926070351,0.0108622600474418,
-0.0102708948460321));
#32140=CARTESIAN_POINT('Ctrl Pts',(-0.230968012103738,0.0109020648308885,
-0.0102554849026716));
#32141=CARTESIAN_POINT('Ctrl Pts',(-0.231002711858128,0.0109427731882278,
-0.0102393637094851));
#32142=CARTESIAN_POINT('Ctrl Pts',(-0.231035398896431,0.0109814222351681,
-0.0102237263817688));
#32143=CARTESIAN_POINT('Ctrl Pts',(-0.231099901055102,0.0110576893761418,
-0.010192868847837));
#32144=CARTESIAN_POINT('Ctrl Pts',(-0.231156559478863,0.0111259983585293,
-0.0101640205438184));
#32145=CARTESIAN_POINT('Ctrl Pts',(-0.231211835149342,0.0111940704020128,
-0.0101342874093605));
#32146=CARTESIAN_POINT('Ctrl Pts',(-0.231267110819821,0.0112621424454963,
-0.0101045542749026));
#32147=CARTESIAN_POINT('Ctrl Pts',(-0.23132100653357,0.0113299180323245,
-0.010073805833687));
#32148=CARTESIAN_POINT('Ctrl Pts',(-0.23136787049939,0.011389691696947,
-0.0100458771804067));
#32149=CARTESIAN_POINT('Ctrl Pts',(-0.231414734465211,0.0114494653615695,
-0.0100179485271265));
#32150=CARTESIAN_POINT('Ctrl Pts',(-0.231454561628712,0.0115013491391876,
-0.00999307644786312));
#32151=CARTESIAN_POINT('Ctrl Pts',(-0.231503504946577,0.0115686589515727,
-0.00995964927974371));
#32152=CARTESIAN_POINT('Ctrl Pts',(-0.231552448264441,0.0116359687639579,
-0.0099262221116243));
#32153=CARTESIAN_POINT('Ctrl Pts',(-0.23161051693924,0.0117184863969086,
-0.00988380564676722));
#32154=CARTESIAN_POINT('Ctrl Pts',(-0.231658296470953,0.0117892053597625,
-0.00984606356092155));
#32155=CARTESIAN_POINT('Ctrl Pts',(-0.231706076002667,0.0118599243226163,
-0.00980832147507588));
#32156=CARTESIAN_POINT('Ctrl Pts',(-0.231743556658961,0.0119190988785855,
-0.00977571832815352));
#32157=CARTESIAN_POINT('Ctrl Pts',(-0.231784756299534,0.0119911418525335,
-0.00973463888789059));
#32158=CARTESIAN_POINT('Ctrl Pts',(-0.231825955940108,0.0120631848264815,
-0.00969355944762766));
#32159=CARTESIAN_POINT('Ctrl Pts',(-0.231870883582506,0.0121478440626175,
-0.00964356931092481));
#32160=CARTESIAN_POINT('Ctrl Pts',(-0.231906811484744,0.0122229265082499,
-0.00959750935911378));
#32161=CARTESIAN_POINT('Ctrl Pts',(-0.231942739386982,0.0122980089538823,
-0.00955144940730275));
#32162=CARTESIAN_POINT('Ctrl Pts',(-0.231969660030808,0.0123637434774996,
-0.00950968646531456));
#32163=CARTESIAN_POINT('Ctrl Pts',(-0.231991468015951,0.0124353497128256,
-0.00946264718223883));
#32164=CARTESIAN_POINT('Ctrl Pts',(-0.232035083986235,0.0125785621834778,
-0.00936856861608737));
#32165=CARTESIAN_POINT('Ctrl Pts',(-0.23205827808065,0.0127443218159472,
-0.0092519649420025));
#32166=CARTESIAN_POINT('Ctrl Pts',(-0.232043483449447,0.0128903437766426,
-0.0091412056146135));
#32167=CARTESIAN_POINT('Ctrl Pts',(-0.232036086133846,0.0129633547569904,
-0.009085825950919));
#32168=CARTESIAN_POINT('Ctrl Pts',(-0.232019186068209,0.0130316500789959,
-0.0090321924318841));
#32169=CARTESIAN_POINT('Ctrl Pts',(-0.231991634815625,0.0131027443802735,
-0.00897444119022315));
#32170=CARTESIAN_POINT('Ctrl Pts',(-0.23196408356304,0.0131738386815511,
-0.0089166899485622));
#32171=CARTESIAN_POINT('Ctrl Pts',(-0.231925885937843,0.0132475287214381,
-0.00885457037433584));
#32172=CARTESIAN_POINT('Ctrl Pts',(-0.231889750347582,0.013306209782967,
-0.00880373558487667));
#32173=CARTESIAN_POINT('Ctrl Pts',(-0.23185361475732,0.0133648908444959,
-0.00875290079541749));
#32174=CARTESIAN_POINT('Ctrl Pts',(-0.231819535158648,0.0134088405277549,
-0.00871367215862119));
#32175=CARTESIAN_POINT('Ctrl Pts',(-0.231777056882382,0.013458357573902,
-0.00866858901449053));
#32176=CARTESIAN_POINT('Ctrl Pts',(-0.231734578606116,0.0135078746200491,
-0.00862350587035986));
#32177=CARTESIAN_POINT('Ctrl Pts',(-0.231683705298113,0.0135627803727237,
-0.00857237091817839));
#32178=CARTESIAN_POINT('Ctrl Pts',(-0.231628986423714,0.0136163616562068,
-0.00852107800022125));
#32179=CARTESIAN_POINT('Ctrl Pts',(-0.231590792768567,0.013653761275373,
-0.00848527565520792));
#32180=CARTESIAN_POINT('Ctrl Pts',(-0.231550724619769,0.0136905495698959,
-0.00844943454284152));
#32181=CARTESIAN_POINT('Ctrl Pts',(-0.231506147015012,0.0137288292478143,
-0.00841142376562983));
#32182=CARTESIAN_POINT('Ctrl Pts',(-0.231486859657217,0.0137453916864714,
-0.00839497767203373));
#32183=CARTESIAN_POINT('Ctrl Pts',(-0.231466728117272,0.0137622314440902,
-0.00837812360215855));
#32184=CARTESIAN_POINT('Ctrl Pts',(-0.23144553897158,0.0137795097865656,
-0.00836068050978691));
#32185=CARTESIAN_POINT('Ctrl Pts',(-0.231375376743527,0.0138367224284889,
-0.00830292234234003));
#32186=CARTESIAN_POINT('Ctrl Pts',(-0.231293622555022,0.0138985813194139,
-0.00823853409137215));
#32187=CARTESIAN_POINT('Ctrl Pts',(-0.231226714525978,0.013947040708293,
-0.0081868881426923));
#32188=CARTESIAN_POINT('Ctrl Pts',(-0.231159806496934,0.0139955000971721,
-0.00813524219401245));
#32189=CARTESIAN_POINT('Ctrl Pts',(-0.231107739434246,0.0140308717053663,
-0.00809663782142736));
#32190=CARTESIAN_POINT('Ctrl Pts',(-0.231041587164618,0.0140742389559795,
-0.00804842920666416));
#32191=CARTESIAN_POINT('Ctrl Pts',(-0.23097543489499,0.0141176062065926,
-0.00800022059190097));
#32192=CARTESIAN_POINT('Ctrl Pts',(-0.230895202143996,0.0141686670137287,
-0.00794212927864545));
#32193=CARTESIAN_POINT('Ctrl Pts',(-0.230830248345273,0.0142088152135737,
-0.007895472402854));
#32194=CARTESIAN_POINT('Ctrl Pts',(-0.230765294546549,0.0142489634134188,
-0.00784881552706254));
#32195=CARTESIAN_POINT('Ctrl Pts',(-0.230715615487131,0.014278491958761,
-0.00781384935289027));
#32196=CARTESIAN_POINT('Ctrl Pts',(-0.2306479977017,0.0143177721079901,
-0.0077664766629716));
#32197=CARTESIAN_POINT('Ctrl Pts',(-0.230580379916268,0.0143570522572192,
-0.00771910397305294));
#32198=CARTESIAN_POINT('Ctrl Pts',(-0.230494827219163,0.0144058030335849,
-0.00765908731777351));
#32199=CARTESIAN_POINT('Ctrl Pts',(-0.230419563342902,0.0144478003300146,
-0.0076061272432004));
#32200=CARTESIAN_POINT('Ctrl Pts',(-0.23034429946664,0.0144897976264443,
-0.0075531671686273));
#32201=CARTESIAN_POINT('Ctrl Pts',(-0.23027932188938,0.0145252487348904,
-0.00750742818708478));
#32202=CARTESIAN_POINT('Ctrl Pts',(-0.230211958684545,0.0145614671965424,
-0.00745988023620919));
#32203=CARTESIAN_POINT('Ctrl Pts',(-0.230144595479711,0.0145976856581944,
-0.0074123322853336));
#32204=CARTESIAN_POINT('Ctrl Pts',(-0.23007484731461,0.0146346073714077,
-0.00736292855388468));
#32205=CARTESIAN_POINT('Ctrl Pts',(-0.23000379887155,0.0146717813647277,
-0.00731212793154391));
#32206=CARTESIAN_POINT('Ctrl Pts',(-0.229932750428491,0.0147089553580477,
-0.00726132730920313));
#32207=CARTESIAN_POINT('Ctrl Pts',(-0.22986040194103,0.014746365348263,
-0.00720911560519303));
#32208=CARTESIAN_POINT('Ctrl Pts',(-0.229791588342911,0.0147817912340649,
-0.00715866362205958));
#32209=CARTESIAN_POINT('Ctrl Pts',(-0.229722774744791,0.0148172171198668,
-0.00710821163892614));
#32210=CARTESIAN_POINT('Ctrl Pts',(-0.229657495501249,0.0148507081915223,
-0.00705955615765789));
#32211=CARTESIAN_POINT('Ctrl Pts',(-0.229589479953617,0.0148855070542966,
-0.00700795588366666));
#32212=CARTESIAN_POINT('Ctrl Pts',(-0.229453448858355,0.0149551047798453,
-0.0069047553356842));
#32213=CARTESIAN_POINT('Ctrl Pts',(-0.22930647593101,0.0150295874152323,
-0.00678953050805577));
#32214=CARTESIAN_POINT('Ctrl Pts',(-0.229171345764821,0.0150973553358833,
-0.00667973005196626));
#32215=CARTESIAN_POINT('Ctrl Pts',(-0.229036215598631,0.0151651232565343,
-0.00656992959587674));
#32216=CARTESIAN_POINT('Ctrl Pts',(-0.228912924944156,0.0152266020801001,
-0.00646582291419951));
#32217=CARTESIAN_POINT('Ctrl Pts',(-0.228784731269557,0.0152901893183376,
-0.00635310900734669));
#32218=CARTESIAN_POINT('Ctrl Pts',(-0.228656537594957,0.015353776556575,
-0.00624039510049387));
#32219=CARTESIAN_POINT('Ctrl Pts',(-0.228523442779258,0.0154191443299652,
-0.00611888796668704));
#32220=CARTESIAN_POINT('Ctrl Pts',(-0.228396736144486,0.0154805617283158,
-0.00599843481886273));
#32221=CARTESIAN_POINT('Ctrl Pts',(-0.228270029509714,0.0155419791266665,
-0.00587798167103842));
#32222=CARTESIAN_POINT('Ctrl Pts',(-0.228149709917567,0.0155997207953437,
-0.00575872349910771));
#32223=CARTESIAN_POINT('Ctrl Pts',(-0.228026646433393,0.0156579298630215,
-0.00563126705671706));
#32224=CARTESIAN_POINT('Ctrl Pts',(-0.228016605549242,0.015662679204461,
-0.00562086774630496));
#32225=CARTESIAN_POINT('Ctrl Pts',(-0.228006546404433,0.0156674307478862,
-0.00561041336623902));
#32226=CARTESIAN_POINT('Ctrl Pts',(-0.227996474915176,0.0156721811407406,
-0.00559990996590028));
#32227=CARTESIAN_POINT('Ctrl Pts',(-0.227883107816741,0.0157256527019563,
-0.00548168117274438));
#32228=CARTESIAN_POINT('Ctrl Pts',(-0.227768176640571,0.0157788534865566,
-0.00535719105107656));
#32229=CARTESIAN_POINT('Ctrl Pts',(-0.227660119078464,0.0158278578958162,
-0.00523542087007314));
#32230=CARTESIAN_POINT('Ctrl Pts',(-0.227542461724258,0.015881215837875,
-0.00510283267320184));
#32231=CARTESIAN_POINT('Ctrl Pts',(-0.227432953141424,0.0159299038159691,
-0.00497359566486382));
#32232=CARTESIAN_POINT('Ctrl Pts',(-0.227323539266157,0.0159777270605206,
-0.00483732653405633));
#32233=CARTESIAN_POINT('Ctrl Pts',(-0.227104711515624,0.0160733735496236,
-0.00456478827244135));
#32234=CARTESIAN_POINT('Ctrl Pts',(-0.226886262490342,0.0161640968769926,
-0.00426357577786167));
#32235=CARTESIAN_POINT('Ctrl Pts',(-0.226686889965372,0.016238216528244,
-0.00396147808314125));
#32236=CARTESIAN_POINT('Ctrl Pts',(-0.226487517440402,0.0163123361794955,
-0.00365938038842082));
#32237=CARTESIAN_POINT('Ctrl Pts',(-0.226307228819621,0.0163715748698451,
-0.00335681294423736));
#32238=CARTESIAN_POINT('Ctrl Pts',(-0.22613006964741,0.0164173393056575,
-0.00302983300065918));
#32239=CARTESIAN_POINT('Ctrl Pts',(-0.226041490061305,0.0164402215235637,
-0.00286634302887009));
#32240=CARTESIAN_POINT('Ctrl Pts',(-0.225953689054931,0.0164593064887217,
-0.00269670427482913));
#32241=CARTESIAN_POINT('Ctrl Pts',(-0.225873228778512,0.0164732474391017,
-0.00253266872281594));
#32242=CARTESIAN_POINT('Ctrl Pts',(-0.225839509654998,0.0164790897832831,
-0.00246392504848051));
#32243=CARTESIAN_POINT('Ctrl Pts',(-0.225807079371206,0.0164840666076802,
-0.00239619099430726));
#32244=CARTESIAN_POINT('Ctrl Pts',(-0.225775739961391,0.0164882613906457,
-0.00232903612135096));
#32245=CARTESIAN_POINT('Ctrl Pts',(-0.22573229754672,0.0164940761619552,
-0.00223594662619258));
#32246=CARTESIAN_POINT('Ctrl Pts',(-0.225690951274861,0.0164996201239921,
-0.00214463734262893));
#32247=CARTESIAN_POINT('Ctrl Pts',(-0.225651173843744,0.0165049400475781,
-0.00205378107599625));
#32248=CARTESIAN_POINT('Ctrl Pts',(-0.225582700926324,0.016514097770391,
-0.00189738099013219));
#32249=CARTESIAN_POINT('Ctrl Pts',(-0.2255188625694,0.0165225938264315,
-0.00174296906619653));
#32250=CARTESIAN_POINT('Ctrl Pts',(-0.22545387460209,0.0165308013835412,
-0.00157727287014463));
#32251=CARTESIAN_POINT('Ctrl Pts',(-0.225421380618434,0.0165349051620961,
-0.00149442477211867));
#32252=CARTESIAN_POINT('Ctrl Pts',(-0.225388599309305,0.0165389341830696,
-0.0014087549278449));
#32253=CARTESIAN_POINT('Ctrl Pts',(-0.225354400970614,0.0165429393029416,
-0.0013165744898758));
#32254=CARTESIAN_POINT('Ctrl Pts',(-0.225334634352807,0.0165452542596561,
-0.00126329425591231));
#32255=CARTESIAN_POINT('Ctrl Pts',(-0.225314394059584,0.016547552895731,
-0.0012078361574181));
#32256=CARTESIAN_POINT('Ctrl Pts',(-0.225294998104697,0.0165496652083673,
-0.00115407592783882));
#32257=CARTESIAN_POINT('Ctrl Pts',(-0.225280837006934,0.0165512074199223,
-0.00111482527628472));
#32258=CARTESIAN_POINT('Ctrl Pts',(-0.225267125987414,0.0165526516895471,
-0.00107647865586791));
#32259=CARTESIAN_POINT('Ctrl Pts',(-0.225254377998706,0.0165539545376519,
-0.00104054141329506));
#32260=CARTESIAN_POINT('Ctrl Pts',(-0.225224169540618,0.0165570418507387,
-0.000955382200266533));
#32261=CARTESIAN_POINT('Ctrl Pts',(-0.225199370447548,0.0165594075983991,
-0.000883760964632949));
#32262=CARTESIAN_POINT('Ctrl Pts',(-0.225169605988872,0.0165619809696788,
-0.000796234956166043));
#32263=CARTESIAN_POINT('Ctrl Pts',(-0.225139841530196,0.0165645543409585,
-0.000708708947699136));
#32264=CARTESIAN_POINT('Ctrl Pts',(-0.225105109287165,0.016567173521703,
-0.000605273992315721));
#32265=CARTESIAN_POINT('Ctrl Pts',(-0.225077485368256,0.0165689500200869,
-0.000522302514831214));
#32266=CARTESIAN_POINT('Ctrl Pts',(-0.225049861449347,0.0165707265184708,
-0.000439331037346707));
#32267=CARTESIAN_POINT('Ctrl Pts',(-0.225029348756218,0.0165718486883789,
-0.000376825865973877));
#32268=CARTESIAN_POINT('Ctrl Pts',(-0.225002310730227,0.0165730394231567,
-0.000294349705289951));
#32269=CARTESIAN_POINT('Ctrl Pts',(-0.224975272938767,0.0165742301476059,
-0.000211874260014666));
#32270=CARTESIAN_POINT('Ctrl Pts',(-0.224941708010107,0.0165753666276692,
-0.000109427566739171));
#32271=CARTESIAN_POINT('Ctrl Pts',(-0.224906163263034,0.0165759221188024,
-4.4501404137285E-7));
#32272=CARTESIAN_POINT('Ctrl Pts',(-0.224906162751896,0.016575922126827,
-4.40896898322947E-7));
#32273=CARTESIAN_POINT('Ctrl Pts',(-0.224941316351692,0.0165753758643503,
0.000108387621803853));
#32274=CARTESIAN_POINT('Ctrl Pts',(-0.225007616272799,0.0165730232478589,
0.00031277968645102));
#32275=CARTESIAN_POINT('Ctrl Pts',(-0.225067714507346,0.0165698105290274,
0.000497786035753373));
#32276=CARTESIAN_POINT('Ctrl Pts',(-0.225170449863763,0.0165620461258707,
0.00080734815416336));
#32277=CARTESIAN_POINT('Ctrl Pts',(-0.225244110283856,0.0165549138835177,
0.00102286209902418));
#32278=CARTESIAN_POINT('Ctrl Pts',(-0.225347914701633,0.0165433851135797,
0.00131538426692397));
#32279=CARTESIAN_POINT('Ctrl Pts',(-0.225461777579014,0.0165291028114222,
0.00162079186653887));
#32280=CARTESIAN_POINT('Ctrl Pts',(-0.225605867979303,0.0165102324611029,
0.00197868258918669));
#32281=CARTESIAN_POINT('Ctrl Pts',(-0.225719822319268,0.0164937064301101,
0.00223747884891758));
#32282=CARTESIAN_POINT('Ctrl Pts',(-0.225761332775488,0.0164871798990637,
0.00232893089033043));
#32283=CARTESIAN_POINT('',(-0.204292068243473,0.00260972885206963,-0.00893763826762711));
#32284=CARTESIAN_POINT('',(-0.203101435073175,0.00260940702415168,-0.00891395394943401));
#32285=CARTESIAN_POINT('',(-0.204292066964792,0.00260973006230206,-0.00893763333202277));
#32286=CARTESIAN_POINT('',(-0.203011006310301,0.00748198867741155,-0.0102941239933332));
#32287=CARTESIAN_POINT('Ctrl Pts',(-0.203013460631671,0.00748225597834897,
-0.01029589855914));
#32288=CARTESIAN_POINT('Ctrl Pts',(-0.202890737335905,0.00646872173921062,
-0.0102911781864089));
#32289=CARTESIAN_POINT('Ctrl Pts',(-0.202862048102838,0.00560185800414398,
-0.0101217239278096));
#32290=CARTESIAN_POINT('Ctrl Pts',(-0.202882559174494,0.00402897744691195,
-0.00967756834064981));
#32291=CARTESIAN_POINT('Ctrl Pts',(-0.20298717036797,0.00325117937997227,
-0.00930626342577085));
#32292=CARTESIAN_POINT('Ctrl Pts',(-0.203101405362522,0.00261009398323347,
-0.00891437067179455));
#32293=CARTESIAN_POINT('',(-0.203091797564858,0.0123956741229182,-0.00891063212388402));
#32294=CARTESIAN_POINT('Ctrl Pts',(-0.202996531950095,0.00750041510153064,
-0.0102955329893099));
#32295=CARTESIAN_POINT('Ctrl Pts',(-0.202973028026754,0.00777693274683738,
-0.0102949893546688));
#32296=CARTESIAN_POINT('Ctrl Pts',(-0.202943195461771,0.00814713734367451,
-0.0102756841645984));
#32297=CARTESIAN_POINT('Ctrl Pts',(-0.202918432522134,0.00848992946228484,
-0.0102417477030021));
#32298=CARTESIAN_POINT('Ctrl Pts',(-0.202906521722816,0.00867191060366439,
-0.0102195296512017));
#32299=CARTESIAN_POINT('Ctrl Pts',(-0.202900439779019,0.0087699904262681,
-0.0102066421178496));
#32300=CARTESIAN_POINT('Ctrl Pts',(-0.202890125869248,0.00895850416585149,
-0.0101787708011005));
#32301=CARTESIAN_POINT('Ctrl Pts',(-0.202880281088442,0.00917285871040499,
-0.0101425325315666));
#32302=CARTESIAN_POINT('Ctrl Pts',(-0.20286726104683,0.00955455309447455,
-0.0100679416187396));
#32303=CARTESIAN_POINT('Ctrl Pts',(-0.202863125830161,0.0100404412202094,
-0.00994714991380413));
#32304=CARTESIAN_POINT('Ctrl Pts',(-0.202883413807161,0.0106634592954592,
-0.00974969172924713));
#32305=CARTESIAN_POINT('Ctrl Pts',(-0.202926466180208,0.011176146849084,
-0.00954413107948249));
#32306=CARTESIAN_POINT('Ctrl Pts',(-0.202963217506325,0.0114893497038527,
-0.00940050398062725));
#32307=CARTESIAN_POINT('Ctrl Pts',(-0.202987606167699,0.0116811097923209,
-0.00930735232445663));
#32308=CARTESIAN_POINT('Ctrl Pts',(-0.203011098769037,0.0118529110797574,
-0.00921921645915818));
#32309=CARTESIAN_POINT('Ctrl Pts',(-0.203023596144259,0.0119401612959071,
-0.00917268091639791));
#32310=CARTESIAN_POINT('Ctrl Pts',(-0.20304984841018,0.0121205772363098,
-0.00907410908661622));
#32311=CARTESIAN_POINT('Ctrl Pts',(-0.203073505202074,0.0122772375631162,
-0.00898320363019314));
#32312=CARTESIAN_POINT('Ctrl Pts',(-0.203091797564858,0.0123956741229182,
-0.00891063212388402));
#32313=CARTESIAN_POINT('',(-0.204293520825211,0.0123942668896669,-0.00893520818590632));
#32314=CARTESIAN_POINT('',(-0.203091797686605,0.0123956703258418,-0.00891062595725835));
#32315=CARTESIAN_POINT('',(-0.20419682992175,0.00750016549753868,-0.0103226607303034));
#32316=CARTESIAN_POINT('Ctrl Pts',(-0.204293519302538,0.0123942655493259,
-0.00893520562090602));
#32317=CARTESIAN_POINT('Ctrl Pts',(-0.204275098485375,0.0122750823755585,
-0.0090084200287585));
#32318=CARTESIAN_POINT('Ctrl Pts',(-0.204259255211995,0.012170250463801,
-0.00906927480190584));
#32319=CARTESIAN_POINT('Ctrl Pts',(-0.20424519845668,0.0120752472755363,
-0.00912256605009863));
#32320=CARTESIAN_POINT('Ctrl Pts',(-0.204238170046716,0.0120277454630579,
-0.00914921179667441));
#32321=CARTESIAN_POINT('Ctrl Pts',(-0.204231589290253,0.0119826708213253,
-0.0091739156221354));
#32322=CARTESIAN_POINT('Ctrl Pts',(-0.20422624416428,0.0119458045626052,
-0.00919383477161695));
#32323=CARTESIAN_POINT('Ctrl Pts',(-0.204220899038308,0.0119089383038851,
-0.0092137539210985));
#32324=CARTESIAN_POINT('Ctrl Pts',(-0.204216787075737,0.0118803470916992,
-0.0092290098761559));
#32325=CARTESIAN_POINT('Ctrl Pts',(-0.20421076071024,0.0118372591327625,
-0.00925156467436655));
#32326=CARTESIAN_POINT('Ctrl Pts',(-0.204204734344742,0.0117941711738258,
-0.0092741194725772));
#32327=CARTESIAN_POINT('Ctrl Pts',(-0.204196798018096,0.0117364718292927,
-0.00930375609662389));
#32328=CARTESIAN_POINT('Ctrl Pts',(-0.204189753233104,0.0116835824953197,
-0.00933020964390826));
#32329=CARTESIAN_POINT('Ctrl Pts',(-0.204182708448112,0.0116306931613467,
-0.00935666319119263));
#32330=CARTESIAN_POINT('Ctrl Pts',(-0.204176552159317,0.0115826860432461,
-0.00938008049394186));
#32331=CARTESIAN_POINT('Ctrl Pts',(-0.204170681369622,0.0115357770237326,
-0.00940252102891353));
#32332=CARTESIAN_POINT('Ctrl Pts',(-0.204158939790232,0.0114419589847058,
-0.00944740209885687));
#32333=CARTESIAN_POINT('Ctrl Pts',(-0.204148340304367,0.0113525401346867,
-0.00948837408639008));
#32334=CARTESIAN_POINT('Ctrl Pts',(-0.20413834448362,0.011258693490137,
-0.00952957213746872));
#32335=CARTESIAN_POINT('Ctrl Pts',(-0.204121215724028,0.0110978786202386,
-0.00960016879285344));
#32336=CARTESIAN_POINT('Ctrl Pts',(-0.204105871698475,0.0109238361022606,
-0.00967093396616449));
#32337=CARTESIAN_POINT('Ctrl Pts',(-0.204094150246153,0.0107476948613483,
-0.00973616780463667));
#32338=CARTESIAN_POINT('Ctrl Pts',(-0.204092191135597,0.0107182548094752,
-0.00974707091613151));
#32339=CARTESIAN_POINT('Ctrl Pts',(-0.204090333223107,0.0106887587382086,
-0.00975782541208224));
#32340=CARTESIAN_POINT('Ctrl Pts',(-0.204088585089726,0.0106592618421083,
-0.00976841253402361));
#32341=CARTESIAN_POINT('Ctrl Pts',(-0.204076377790565,0.0104532836033615,
-0.00984234291379877));
#32342=CARTESIAN_POINT('Ctrl Pts',(-0.204069516229899,0.010247177684889,
-0.00990802601270076));
#32343=CARTESIAN_POINT('Ctrl Pts',(-0.204066818073886,0.0100469521393359,
-0.00996476619728215));
#32344=CARTESIAN_POINT('Ctrl Pts',(-0.204064119917873,0.00984672659378275,
-0.0100215063818635));
#32345=CARTESIAN_POINT('Ctrl Pts',(-0.204065571120084,0.00965260417818384,
-0.0100699507180676));
#32346=CARTESIAN_POINT('Ctrl Pts',(-0.204071293829835,0.00944014979634324,
-0.0101152576551124));
#32347=CARTESIAN_POINT('Ctrl Pts',(-0.204077016539586,0.00922769541450265,
-0.0101605645921573));
#32348=CARTESIAN_POINT('Ctrl Pts',(-0.204087041836827,0.00899660628102227,
-0.0102013362099875));
#32349=CARTESIAN_POINT('Ctrl Pts',(-0.204099347318883,0.00878303173230227,
-0.0102313445479147));
#32350=CARTESIAN_POINT('Ctrl Pts',(-0.204105500059911,0.00867624445794228,
-0.0102463487168783));
#32351=CARTESIAN_POINT('Ctrl Pts',(-0.204112216295476,0.00857387041820424,
-0.0102589531602456));
#32352=CARTESIAN_POINT('Ctrl Pts',(-0.204119551135905,0.00846894111221058,
-0.0102701237466303));
#32353=CARTESIAN_POINT('Ctrl Pts',(-0.204123218556119,0.00841647645921375,
-0.0102757090398227));
#32354=CARTESIAN_POINT('Ctrl Pts',(-0.20412704193822,0.00836336762879549,
-0.0102808777182749));
#32355=CARTESIAN_POINT('Ctrl Pts',(-0.204130486733839,0.00831673252746664,
-0.0102850758848288));
#32356=CARTESIAN_POINT('Ctrl Pts',(-0.204133931529458,0.0082700974261378,
-0.0102892740513827));
#32357=CARTESIAN_POINT('Ctrl Pts',(-0.204136995799708,0.00822994345958339,
-0.0102925877238228));
#32358=CARTESIAN_POINT('Ctrl Pts',(-0.204140419329825,0.00818593090051333,
-0.0102959302516981));
#32359=CARTESIAN_POINT('Ctrl Pts',(-0.204154113448717,0.0080098806844698,
-0.0103093003616625));
#32360=CARTESIAN_POINT('Ctrl Pts',(-0.204173578333277,0.00777202871891889,
-0.0103221303376117));
#32361=CARTESIAN_POINT('Ctrl Pts',(-0.204196829918995,0.00750016549729199,
-0.0103226607246193));
#32362=CARTESIAN_POINT('Ctrl Pts',(-0.204196829927013,0.00750016540354124,
-0.0103226607248022));
#32363=CARTESIAN_POINT('Ctrl Pts',(-0.204185296600283,0.00736627557242382,
-0.0103224024649696));
#32364=CARTESIAN_POINT('Ctrl Pts',(-0.204170173720485,0.00718828267231201,
-0.0103179549294819));
#32365=CARTESIAN_POINT('Ctrl Pts',(-0.204153088630003,0.00698026742655806,
-0.0103073072515267));
#32366=CARTESIAN_POINT('Ctrl Pts',(-0.204144365129465,0.00687195683859182,
-0.0103005485999431));
#32367=CARTESIAN_POINT('Ctrl Pts',(-0.204129528175449,0.00667906286088234,
-0.0102853466214339));
#32368=CARTESIAN_POINT('Ctrl Pts',(-0.204114088107036,0.00646341547837495,
-0.0102635347495406));
#32369=CARTESIAN_POINT('Ctrl Pts',(-0.204098618494934,0.00622876334523883,
-0.0102348069970239));
#32370=CARTESIAN_POINT('Ctrl Pts',(-0.204080493922748,0.00587940935304134,
-0.0101798881435763));
#32371=CARTESIAN_POINT('Ctrl Pts',(-0.204066164101744,0.0054538486912532,
-0.0100959729412001));
#32372=CARTESIAN_POINT('Ctrl Pts',(-0.204061500170532,0.00496565424176834,
-0.00997598165923886));
#32373=CARTESIAN_POINT('Ctrl Pts',(-0.204079665330309,0.00443189461430586,
-0.00980478175309179));
#32374=CARTESIAN_POINT('Ctrl Pts',(-0.204106657151681,0.00405435642971818,
-0.00966232705712367));
#32375=CARTESIAN_POINT('Ctrl Pts',(-0.204137703479563,0.00373318001710212,
-0.00952804466465791));
#32376=CARTESIAN_POINT('Ctrl Pts',(-0.204163349720393,0.00351683255250259,
-0.00942841282273942));
#32377=CARTESIAN_POINT('Ctrl Pts',(-0.204187933392733,0.00332430267970029,
-0.00933487767638302));
#32378=CARTESIAN_POINT('Ctrl Pts',(-0.204211586788645,0.00315180164980181,
-0.00924625546080158));
#32379=CARTESIAN_POINT('Ctrl Pts',(-0.204223864452251,0.00306614233221466,
-0.0092005126880041));
#32380=CARTESIAN_POINT('Ctrl Pts',(-0.204250056460208,0.00288600567993886,
-0.00910201089232994));
#32381=CARTESIAN_POINT('Ctrl Pts',(-0.204273721709538,0.00272888562244924,
-0.00901075832037522));
#32382=CARTESIAN_POINT('Ctrl Pts',(-0.204292066659032,0.00260972723221402,
-0.0089376405099374));
#32383=CARTESIAN_POINT('',(-0.206293207427109,0.00261116688226644,-0.00897808488880184));
#32384=CARTESIAN_POINT('',(-0.205091220874504,0.00261029994409268,-0.00895378396279216));
#32385=CARTESIAN_POINT('',(-0.206293206209515,0.00261116809564738,-0.00897808010478434));
#32386=CARTESIAN_POINT('',(-0.204995830964606,0.00750018061144568,-0.01034071880922));
#32387=CARTESIAN_POINT('Ctrl Pts',(-0.205091218737904,0.00261030113134024,
-0.00895378149630639));
#32388=CARTESIAN_POINT('Ctrl Pts',(-0.205073038446696,0.0027283973634415,
-0.00902637612295405));
#32389=CARTESIAN_POINT('Ctrl Pts',(-0.205049507187242,0.00288473012510694,
-0.00911738532094257));
#32390=CARTESIAN_POINT('Ctrl Pts',(-0.205023348755059,0.00306502113689564,
-0.00921619836789005));
#32391=CARTESIAN_POINT('Ctrl Pts',(-0.205010861943808,0.00315244889182092,
-0.00926296620515238));
#32392=CARTESIAN_POINT('Ctrl Pts',(-0.204987412224421,0.00332423590481222,
-0.00935136480094043));
#32393=CARTESIAN_POINT('Ctrl Pts',(-0.204962930879865,0.00351688601712408,
-0.00944514868659994));
#32394=CARTESIAN_POINT('Ctrl Pts',(-0.204937222363819,0.00373534002291959,
-0.00954583931029786));
#32395=CARTESIAN_POINT('Ctrl Pts',(-0.204906755137115,0.00405272141224298,
-0.00967875941234199));
#32396=CARTESIAN_POINT('Ctrl Pts',(-0.204879536268564,0.00443330123098864,
-0.00982262592539781));
#32397=CARTESIAN_POINT('Ctrl Pts',(-0.204861383847208,0.00496277755586631,
-0.00999271395898353));
#32398=CARTESIAN_POINT('Ctrl Pts',(-0.204865634488468,0.00545524074413209,
-0.0101140737523899));
#32399=CARTESIAN_POINT('Ctrl Pts',(-0.204879709034891,0.00588082021089614,
-0.0101979873791187));
#32400=CARTESIAN_POINT('Ctrl Pts',(-0.204897593596836,0.00622967416483981,
-0.0102528606149596));
#32401=CARTESIAN_POINT('Ctrl Pts',(-0.204912950260743,0.00646383985211491,
-0.0102815531993233));
#32402=CARTESIAN_POINT('Ctrl Pts',(-0.204928345204359,0.00667926356803342,
-0.0103033631066581));
#32403=CARTESIAN_POINT('Ctrl Pts',(-0.20494314048499,0.0068716218281429,
-0.0103185488470304));
#32404=CARTESIAN_POINT('Ctrl Pts',(-0.20495195108621,0.006980845097099,
-0.0103253770145249));
#32405=CARTESIAN_POINT('Ctrl Pts',(-0.204969098328994,0.00718899852828588,
-0.0103360288719754));
#32406=CARTESIAN_POINT('Ctrl Pts',(-0.204984270571741,0.00736672617235706,
-0.0103404601549147));
#32407=CARTESIAN_POINT('Ctrl Pts',(-0.204995830964606,0.00750018061144568,
-0.01034071880922));
#32408=CARTESIAN_POINT('',(-0.205092341371519,0.0123935602159587,-0.00895141703515626));
#32409=CARTESIAN_POINT('Ctrl Pts',(-0.204995831063211,0.00750018174974929,
-0.0103407188114261));
#32410=CARTESIAN_POINT('Ctrl Pts',(-0.204984334367631,0.00763376142047935,
-0.0103404563384653));
#32411=CARTESIAN_POINT('Ctrl Pts',(-0.204969242259353,0.00781169707145735,
-0.0103360126094618));
#32412=CARTESIAN_POINT('Ctrl Pts',(-0.204952175210056,0.00802021735232026,
-0.0103253230549911));
#32413=CARTESIAN_POINT('Ctrl Pts',(-0.204943403020839,0.00812966122370435,
-0.010318469780649));
#32414=CARTESIAN_POINT('Ctrl Pts',(-0.204928658061841,0.00832258199862167,
-0.0103032092465372));
#32415=CARTESIAN_POINT('Ctrl Pts',(-0.204913319337647,0.00853854827886881,
-0.0102812989237937));
#32416=CARTESIAN_POINT('Ctrl Pts',(-0.204898006317538,0.00877356793052689,
-0.0102524253354524));
#32417=CARTESIAN_POINT('Ctrl Pts',(-0.20488022415611,0.00912228369014853,
-0.0101974532003693));
#32418=CARTESIAN_POINT('Ctrl Pts',(-0.20486621057911,0.00954790324330249,
-0.0101133538141053));
#32419=CARTESIAN_POINT('Ctrl Pts',(-0.204861855720688,0.010037836615467,
-0.00999260025333758));
#32420=CARTESIAN_POINT('Ctrl Pts',(-0.204880098002849,0.0105711418094981,
-0.00982106567079185));
#32421=CARTESIAN_POINT('Ctrl Pts',(-0.204907090184449,0.0109495407743111,
-0.00967787507932532));
#32422=CARTESIAN_POINT('Ctrl Pts',(-0.204937963378322,0.0112700899770492,
-0.00954347334300635));
#32423=CARTESIAN_POINT('Ctrl Pts',(-0.204963627185177,0.0114873226245486,
-0.00944315781658447));
#32424=CARTESIAN_POINT('Ctrl Pts',(-0.20498816737331,0.0116797965093522,
-0.00934935193686226));
#32425=CARTESIAN_POINT('Ctrl Pts',(-0.205011652075311,0.0118512232809713,
-0.00926103771969262));
#32426=CARTESIAN_POINT('Ctrl Pts',(-0.205024193079732,0.0119387130080461,
-0.00921418941879961));
#32427=CARTESIAN_POINT('Ctrl Pts',(-0.205050448708611,0.0121189966104724,
-0.0091152741114829));
#32428=CARTESIAN_POINT('Ctrl Pts',(-0.205074081100572,0.0122754031260107,
-0.00902412724127784));
#32429=CARTESIAN_POINT('Ctrl Pts',(-0.205092341371519,0.0123935602159587,
-0.00895141703515626));
#32430=CARTESIAN_POINT('',(-0.20629401114421,0.0123924210579408,-0.00897588382629872));
#32431=CARTESIAN_POINT('',(-0.205092341489181,0.0123935565388823,-0.00895141108884611));
#32432=CARTESIAN_POINT('',(-0.206196247266385,0.00750007921659101,-0.0103678492122642));
#32433=CARTESIAN_POINT('Ctrl Pts',(-0.206294009778539,0.0123924197511446,
-0.00897588136592045));
#32434=CARTESIAN_POINT('Ctrl Pts',(-0.206275629933268,0.0122735287593914,
-0.00904923077174543));
#32435=CARTESIAN_POINT('Ctrl Pts',(-0.206251898274911,0.0121166099521123,
-0.00914086409857169));
#32436=CARTESIAN_POINT('Ctrl Pts',(-0.206225586245474,0.0119364025232917,
-0.00923992860321053));
#32437=CARTESIAN_POINT('Ctrl Pts',(-0.20621320957114,0.011850415602355,
-0.00928608543340328));
#32438=CARTESIAN_POINT('Ctrl Pts',(-0.206189421186814,0.0116777449991496,
-0.00937524164969374));
#32439=CARTESIAN_POINT('Ctrl Pts',(-0.206164666829607,0.0114849804098469,
-0.0094693586360107));
#32440=CARTESIAN_POINT('Ctrl Pts',(-0.206138729986972,0.0112675531340228,
-0.00956992324979396));
#32441=CARTESIAN_POINT('Ctrl Pts',(-0.206107574836102,0.0109483810244031,
-0.00970399210164722));
#32442=CARTESIAN_POINT('Ctrl Pts',(-0.206079918334012,0.0105696487151287,
-0.00984755873583954));
#32443=CARTESIAN_POINT('Ctrl Pts',(-0.206061320221384,0.0100390013969364,
-0.0100186198580634));
#32444=CARTESIAN_POINT('Ctrl Pts',(-0.206065538394757,0.00954660497520976,
-0.0101402971232334));
#32445=CARTESIAN_POINT('Ctrl Pts',(-0.206079659153249,0.00912064692309937,
-0.0102245493877391));
#32446=CARTESIAN_POINT('Ctrl Pts',(-0.206097649530151,0.00877166321992288,
-0.0102796197167479));
#32447=CARTESIAN_POINT('Ctrl Pts',(-0.206113124691997,0.00853683963756153,
-0.0103084791137337));
#32448=CARTESIAN_POINT('Ctrl Pts',(-0.206128578247856,0.00832144144316739,
-0.0103303502197896));
#32449=CARTESIAN_POINT('Ctrl Pts',(-0.206143442183771,0.0081289230195232,
-0.0103455919214823));
#32450=CARTESIAN_POINT('Ctrl Pts',(-0.206152196968296,0.0080207509803179,
-0.0103523791392198));
#32451=CARTESIAN_POINT('Ctrl Pts',(-0.20616937593705,0.00781267213620248,
-0.010363092481908));
#32452=CARTESIAN_POINT('Ctrl Pts',(-0.206184614854141,0.00763433161462997,
-0.0103675851511799));
#32453=CARTESIAN_POINT('Ctrl Pts',(-0.206196247269383,0.00750007928854104,
-0.0103678492126068));
#32454=CARTESIAN_POINT('Ctrl Pts',(-0.206196247263134,0.00750007921687407,
-0.0103678492124662));
#32455=CARTESIAN_POINT('Ctrl Pts',(-0.206184538016218,0.00736579215378392,
-0.0103675857323272));
#32456=CARTESIAN_POINT('Ctrl Pts',(-0.20616920962137,0.00718753481197185,
-0.0103630948863018));
#32457=CARTESIAN_POINT('Ctrl Pts',(-0.206151939567772,0.00697963270310972,
-0.0103523925616913));
#32458=CARTESIAN_POINT('Ctrl Pts',(-0.206143177224608,0.00687203383816881,
-0.010345652193588));
#32459=CARTESIAN_POINT('Ctrl Pts',(-0.206128179901813,0.00667889666688518,
-0.0103303743273525));
#32460=CARTESIAN_POINT('Ctrl Pts',(-0.206112637080238,0.00646336544810845,
-0.0103084932875251));
#32461=CARTESIAN_POINT('Ctrl Pts',(-0.206097083534865,0.00622820103627389,
-0.0102795775402357));
#32462=CARTESIAN_POINT('Ctrl Pts',(-0.206079166473915,0.00588103593041778,
-0.0102248175800093));
#32463=CARTESIAN_POINT('Ctrl Pts',(-0.206065099208172,0.0054560678829398,
-0.010140868723724));
#32464=CARTESIAN_POINT('Ctrl Pts',(-0.206060944985599,0.00496475893419326,
-0.0100196997915405));
#32465=CARTESIAN_POINT('Ctrl Pts',(-0.20607975759831,0.00443234740802005,
-0.00984824726940087));
#32466=CARTESIAN_POINT('Ctrl Pts',(-0.206107426047253,0.00405426418978633,
-0.00970505346746708));
#32467=CARTESIAN_POINT('Ctrl Pts',(-0.206138707262331,0.00373379004888558,
-0.00957052329097599));
#32468=CARTESIAN_POINT('Ctrl Pts',(-0.206164472409347,0.00351745989703588,
-0.00947050613876221));
#32469=CARTESIAN_POINT('Ctrl Pts',(-0.206189109621405,0.00332506288356478,
-0.00937664775095104));
#32470=CARTESIAN_POINT('Ctrl Pts',(-0.206212763871631,0.00315278593877367,
-0.00928777221922359));
#32471=CARTESIAN_POINT('Ctrl Pts',(-0.206225080280031,0.0030669007354627,
-0.00924171469636897));
#32472=CARTESIAN_POINT('Ctrl Pts',(-0.206251269492468,0.00288687783244609,
-0.0091428463681189));
#32473=CARTESIAN_POINT('Ctrl Pts',(-0.206274900907247,0.00273002804570731,
-0.00905134588017306));
#32474=CARTESIAN_POINT('Ctrl Pts',(-0.206293205915242,0.00261116529613781,
-0.00897808708453545));
#32475=CARTESIAN_POINT('',(-0.208294281955803,0.00261264102269791,-0.00901864434210674));
#32476=CARTESIAN_POINT('',(-0.20709233610443,0.00261177385669708,-0.00899428899190795));
#32477=CARTESIAN_POINT('',(-0.208294280799351,0.00261264227468941,-0.00901863964824329));
#32478=CARTESIAN_POINT('',(-0.206995159908711,0.00750002205440221,-0.0103859052997544));
#32479=CARTESIAN_POINT('Ctrl Pts',(-0.207092334177755,0.0026117750543677,
-0.00899428657135199));
#32480=CARTESIAN_POINT('Ctrl Pts',(-0.207074189408243,0.00272957361446454,
-0.00906701495139803));
#32481=CARTESIAN_POINT('Ctrl Pts',(-0.207050686386804,0.00288563070243773,
-0.00915826339207637));
#32482=CARTESIAN_POINT('Ctrl Pts',(-0.207024524692812,0.0030657969487444,
-0.00925743433152502));
#32483=CARTESIAN_POINT('Ctrl Pts',(-0.207011996627476,0.00315344113935562,
-0.00930451415959934));
#32484=CARTESIAN_POINT('Ctrl Pts',(-0.206988540251261,0.00332499174150683,
-0.00939315711270464));
#32485=CARTESIAN_POINT('Ctrl Pts',(-0.206963992767868,0.00351757661523681,
-0.00948728809442778));
#32486=CARTESIAN_POINT('Ctrl Pts',(-0.206938222613739,0.00373542462863214,
-0.00958812909678874));
#32487=CARTESIAN_POINT('Ctrl Pts',(-0.206907280012449,0.00405444268434713,
-0.00972222069990457));
#32488=CARTESIAN_POINT('Ctrl Pts',(-0.206879699677835,0.00443263550097346,
-0.00986566273753742));
#32489=CARTESIAN_POINT('Ctrl Pts',(-0.206860828660484,0.00496231258650676,
-0.0100365956434048));
#32490=CARTESIAN_POINT('Ctrl Pts',(-0.206864635917835,0.00545699157383567,
-0.0101588612972589));
#32491=CARTESIAN_POINT('Ctrl Pts',(-0.206878443249798,0.00588212796561463,
-0.0102428714297392));
#32492=CARTESIAN_POINT('Ctrl Pts',(-0.206896114734401,0.0062290841634208,
-0.0102976326277652));
#32493=CARTESIAN_POINT('Ctrl Pts',(-0.206911530121765,0.0064637966547499,
-0.0103265148036063));
#32494=CARTESIAN_POINT('Ctrl Pts',(-0.206927002746087,0.00667909031637067,
-0.010348390628485));
#32495=CARTESIAN_POINT('Ctrl Pts',(-0.206941927161123,0.00687158087442238,
-0.0103636439973363));
#32496=CARTESIAN_POINT('Ctrl Pts',(-0.206950771218564,0.0069801693552064,
-0.0103704600676468));
#32497=CARTESIAN_POINT('Ctrl Pts',(-0.206968081273249,0.00718821308792682,
-0.0103811664345483));
#32498=CARTESIAN_POINT('Ctrl Pts',(-0.206983439481071,0.00736619442711862,
-0.0103856407315178));
#32499=CARTESIAN_POINT('Ctrl Pts',(-0.206995159908711,0.00750002205440221,
-0.0103859052997544));
#32500=CARTESIAN_POINT('',(-0.207092865232531,0.0123914993286869,-0.00899226456837298));
#32501=CARTESIAN_POINT('Ctrl Pts',(-0.206995160031523,0.00750002345672208,
-0.0103859053025266));
#32502=CARTESIAN_POINT('Ctrl Pts',(-0.20698349311307,0.00763394443319968,
-0.0103856412779244));
#32503=CARTESIAN_POINT('Ctrl Pts',(-0.206968199965542,0.00781210259696279,
-0.0103811621280426));
#32504=CARTESIAN_POINT('Ctrl Pts',(-0.206950949156072,0.00802049676584612,
-0.0103704272461815));
#32505=CARTESIAN_POINT('Ctrl Pts',(-0.206942129888732,0.00812932220630246,
-0.0103635892330472));
#32506=CARTESIAN_POINT('Ctrl Pts',(-0.2069272342099,0.00832235552725582,
-0.0103482700117016));
#32507=CARTESIAN_POINT('Ctrl Pts',(-0.206911789920796,0.00853818425630776,
-0.010326302799079));
#32508=CARTESIAN_POINT('Ctrl Pts',(-0.206896386071748,0.00877369921132409,
-0.0102972571016713));
#32509=CARTESIAN_POINT('Ctrl Pts',(-0.206878751394063,0.00912063966793892,
-0.0102423901690412));
#32510=CARTESIAN_POINT('Ctrl Pts',(-0.206864923342377,0.00954576442995532,
-0.0101582262883187));
#32511=CARTESIAN_POINT('Ctrl Pts',(-0.20686095225699,0.0100380835322156,
-0.0100364882851224));
#32512=CARTESIAN_POINT('Ctrl Pts',(-0.206879694411204,0.0105701995383101,
-0.00986470231345221));
#32513=CARTESIAN_POINT('Ctrl Pts',(-0.206907300051337,0.0109490997977367,
-0.00972081160777631));
#32514=CARTESIAN_POINT('Ctrl Pts',(-0.206938373989643,0.0112689311788443,
-0.00958619717352718));
#32515=CARTESIAN_POINT('Ctrl Pts',(-0.20696414502829,0.0114861193909925,
-0.00948552661292593));
#32516=CARTESIAN_POINT('Ctrl Pts',(-0.206988732505316,0.0116784484693535,
-0.00939142218364685));
#32517=CARTESIAN_POINT('Ctrl Pts',(-0.207012217724842,0.0118496547665064,
-0.00930287261316598));
#32518=CARTESIAN_POINT('Ctrl Pts',(-0.207024793977032,0.0119373414710472,
-0.00925572972841337));
#32519=CARTESIAN_POINT('Ctrl Pts',(-0.2070510451993,0.0121174974653495,
-0.00915647501397999));
#32520=CARTESIAN_POINT('Ctrl Pts',(-0.207074643938323,0.0122736323678574,
-0.00906510156350076));
#32521=CARTESIAN_POINT('Ctrl Pts',(-0.207092865232531,0.0123914993286869,
-0.00899226456837298));
#32522=CARTESIAN_POINT('',(-0.208294510632333,0.0123904527314057,-0.00901672992862032));
#32523=CARTESIAN_POINT('',(-0.207092865348001,0.0123914957129992,-0.00899225874580488));
#32524=CARTESIAN_POINT('',(-0.208195607947799,0.00749997628122267,-0.0104130364120898));
#32525=CARTESIAN_POINT('Ctrl Pts',(-0.208294509417452,0.0123904514344384,
-0.00901672753192577));
#32526=CARTESIAN_POINT('Ctrl Pts',(-0.208276181164632,0.0122719181404718,
-0.00909016225797937));
#32527=CARTESIAN_POINT('Ctrl Pts',(-0.208252498633871,0.0121153542506921,
-0.00918197594062883));
#32528=CARTESIAN_POINT('Ctrl Pts',(-0.208226205748594,0.0119353502174475,
-0.00928134228950543));
#32529=CARTESIAN_POINT('Ctrl Pts',(-0.208213799926976,0.0118491943161256,
-0.00932777792712348));
#32530=CARTESIAN_POINT('Ctrl Pts',(-0.208190020192328,0.0116767848974124,
-0.00941715861423961));
#32531=CARTESIAN_POINT('Ctrl Pts',(-0.208165218664378,0.0114841186574925,
-0.00951159792424035));
#32532=CARTESIAN_POINT('Ctrl Pts',(-0.20813924384415,0.0112673281691524,
-0.00961228834450963));
#32533=CARTESIAN_POINT('Ctrl Pts',(-0.208107640684676,0.0109465229857111,
-0.00974752224379483));
#32534=CARTESIAN_POINT('Ctrl Pts',(-0.208079653839285,0.0105700841576997,
-0.00989068383234901));
#32535=CARTESIAN_POINT('Ctrl Pts',(-0.208060396592719,0.0100390834471602,
-0.0100626074030206));
#32536=CARTESIAN_POINT('Ctrl Pts',(-0.20806426493074,0.00954487186568535,
-0.0101850785676279));
#32537=CARTESIAN_POINT('Ctrl Pts',(-0.208078190088483,0.00911929227250148,
-0.0102694456505221));
#32538=CARTESIAN_POINT('Ctrl Pts',(-0.208096036535253,0.00877188338428215,
-0.0103244430295817));
#32539=CARTESIAN_POINT('Ctrl Pts',(-0.208111592493633,0.00853669280746013,
-0.0103534605517206));
#32540=CARTESIAN_POINT('Ctrl Pts',(-0.208127155320244,0.00832140634310011,
-0.0103753960639456));
#32541=CARTESIAN_POINT('Ctrl Pts',(-0.208142180512124,0.00812869235806478,
-0.0103907052740522));
#32542=CARTESIAN_POINT('Ctrl Pts',(-0.208150979455223,0.00802119205908008,
-0.010397474514162));
#32543=CARTESIAN_POINT('Ctrl Pts',(-0.208168348636477,0.00781321983289299,
-0.0104082377911213));
#32544=CARTESIAN_POINT('Ctrl Pts',(-0.208183797114821,0.00763461668549679,
-0.0104127698308575));
#32545=CARTESIAN_POINT('Ctrl Pts',(-0.208195607954992,0.007499976450901,
-0.0104130364190918));
#32546=CARTESIAN_POINT('Ctrl Pts',(-0.208195607940087,0.00749997628188942,
-0.0104130364187545));
#32547=CARTESIAN_POINT('Ctrl Pts',(-0.208183719664188,0.00736516411101924,
-0.0104127673845096));
#32548=CARTESIAN_POINT('Ctrl Pts',(-0.20817336389066,0.00724604273358998,
-0.0104096613586105));
#32549=CARTESIAN_POINT('Ctrl Pts',(-0.208164092614058,0.00713701838909442,
-0.0104051382902462));
#32550=CARTESIAN_POINT('Ctrl Pts',(-0.20815945697382,0.00708250619406622,
-0.010402876755119));
#32551=CARTESIAN_POINT('Ctrl Pts',(-0.208155093639217,0.00703051928157966,
-0.010400208702842));
#32552=CARTESIAN_POINT('Ctrl Pts',(-0.208151447072726,0.00698669776957684,
-0.0103976757432969));
#32553=CARTESIAN_POINT('Ctrl Pts',(-0.208147800506235,0.00694287625757402,
-0.0103951427837518));
#32554=CARTESIAN_POINT('Ctrl Pts',(-0.208144867772773,0.00690721346999065,
-0.0103928748950214));
#32555=CARTESIAN_POINT('Ctrl Pts',(-0.20814087628415,0.00685714754652952,
-0.0103892788868975));
#32556=CARTESIAN_POINT('Ctrl Pts',(-0.208136884795528,0.00680708162306839,
-0.0103856828787736));
#32557=CARTESIAN_POINT('Ctrl Pts',(-0.208131839666141,0.00674262825539959,
-0.010380532083281));
#32558=CARTESIAN_POINT('Ctrl Pts',(-0.20812736491757,0.00668347219054577,
-0.0103751684672179));
#32559=CARTESIAN_POINT('Ctrl Pts',(-0.208122890168998,0.00662431612569194,
-0.0103698048511548));
#32560=CARTESIAN_POINT('Ctrl Pts',(-0.208118982565773,0.00657044290211078,
-0.0103643720707445));
#32561=CARTESIAN_POINT('Ctrl Pts',(-0.208115338133192,0.00651881723080284,
-0.0103587675237056));
#32562=CARTESIAN_POINT('Ctrl Pts',(-0.20810804926803,0.00641556588818696,
-0.010347558429628));
#32563=CARTESIAN_POINT('Ctrl Pts',(-0.208101810000662,0.00632129812238758,
-0.0103357986961478));
#32564=CARTESIAN_POINT('Ctrl Pts',(-0.208095738311044,0.00621657821790559,
-0.0103209758955231));
#32565=CARTESIAN_POINT('Ctrl Pts',(-0.208089666621426,0.0061118583134236,
-0.0103061530948985));
#32566=CARTESIAN_POINT('Ctrl Pts',(-0.208083771217597,0.00599673817473072,
-0.0102878795171945));
#32567=CARTESIAN_POINT('Ctrl Pts',(-0.208079101993661,0.00588611975357556,
-0.0102681842171327));
#32568=CARTESIAN_POINT('Ctrl Pts',(-0.208074432769725,0.00577550133242041,
-0.0102484889170709));
#32569=CARTESIAN_POINT('Ctrl Pts',(-0.208070985265817,0.00566934369931672,
-0.0102275720520985));
#32570=CARTESIAN_POINT('Ctrl Pts',(-0.208068443190351,0.005565699150329,
-0.0102053859028492));
#32571=CARTESIAN_POINT('Ctrl Pts',(-0.208063359039417,0.00535841005235356,
-0.0101610136043507));
#32572=CARTESIAN_POINT('Ctrl Pts',(-0.208061889044625,0.00516113746489649,
-0.0101118982807474));
#32573=CARTESIAN_POINT('Ctrl Pts',(-0.208065058125948,0.00495584654660638,
-0.0100533710595396));
#32574=CARTESIAN_POINT('Ctrl Pts',(-0.208068227207272,0.00475055562831626,
-0.00999484383833177));
#32575=CARTESIAN_POINT('Ctrl Pts',(-0.208076057362027,0.00453750921082217,
-0.00992590844977681));
#32576=CARTESIAN_POINT('Ctrl Pts',(-0.208088021136334,0.00434138309898768,
-0.0098549933278441));
#32577=CARTESIAN_POINT('Ctrl Pts',(-0.208090202592185,0.00430562177121669,
-0.00984206277568236));
#32578=CARTESIAN_POINT('Ctrl Pts',(-0.208092520725194,0.00427041573162259,
-0.00982908721933613));
#32579=CARTESIAN_POINT('Ctrl Pts',(-0.208095012174201,0.00423522751845692,
-0.00981587670658352));
#32580=CARTESIAN_POINT('Ctrl Pts',(-0.208099352661212,0.00417392424401928,
-0.00979286196341021));
#32581=CARTESIAN_POINT('Ctrl Pts',(-0.208104219179505,0.00411266917946915,
-0.00976914801243592));
#32582=CARTESIAN_POINT('Ctrl Pts',(-0.208109805460969,0.00404869361284434,
-0.00974354225869674));
#32583=CARTESIAN_POINT('Ctrl Pts',(-0.208118598280172,0.00394799593151293,
-0.00970323874649185));
#32584=CARTESIAN_POINT('Ctrl Pts',(-0.208129181422691,0.00384066403524311,
-0.00965798872173971));
#32585=CARTESIAN_POINT('Ctrl Pts',(-0.20813963760985,0.00374392741908631,
-0.00961520867146894));
#32586=CARTESIAN_POINT('Ctrl Pts',(-0.208150093797009,0.00364719080292951,
-0.00957242862119817));
#32587=CARTESIAN_POINT('Ctrl Pts',(-0.208160414835794,0.0035608696244637,
-0.0095325080696441));
#32588=CARTESIAN_POINT('Ctrl Pts',(-0.208172085514657,0.00346802947437642,
-0.00948776714366573));
#32589=CARTESIAN_POINT('Ctrl Pts',(-0.208177920854088,0.00342160939933278,
-0.00946539668067656));
#32590=CARTESIAN_POINT('Ctrl Pts',(-0.208184094105983,0.00337357425884607,
-0.00944179621201782));
#32591=CARTESIAN_POINT('Ctrl Pts',(-0.208191119790713,0.00332085407877749,
-0.00941523251609465));
#32592=CARTESIAN_POINT('Ctrl Pts',(-0.208198145475443,0.00326813389870892,
-0.00938866882017148));
#32593=CARTESIAN_POINT('Ctrl Pts',(-0.208206026523807,0.0032107980187599,
-0.00935900113952639));
#32594=CARTESIAN_POINT('Ctrl Pts',(-0.208212027615872,0.00316783533406424,
-0.00933634570123583));
#32595=CARTESIAN_POINT('Ctrl Pts',(-0.208218028707937,0.00312487264936858,
-0.00931369026294528));
#32596=CARTESIAN_POINT('Ctrl Pts',(-0.208222145445723,0.00309616936839642,
-0.00929826115868092));
#32597=CARTESIAN_POINT('Ctrl Pts',(-0.208227474789829,0.00305931342216926,
-0.00927819758755507));
#32598=CARTESIAN_POINT('Ctrl Pts',(-0.208232804133935,0.0030224574759421,
-0.00925813401642922));
#32599=CARTESIAN_POINT('Ctrl Pts',(-0.208239348542458,0.00297751550620315,
-0.00923331539613978));
#32600=CARTESIAN_POINT('Ctrl Pts',(-0.208246332691185,0.00293017920813089,
-0.00920656032436194));
#32601=CARTESIAN_POINT('Ctrl Pts',(-0.208260300947443,0.00283550689119974,
-0.00915305033862115));
#32602=CARTESIAN_POINT('Ctrl Pts',(-0.208276024103448,0.00273113766315477,
-0.00909199637027481));
#32603=CARTESIAN_POINT('Ctrl Pts',(-0.208294280514564,0.00261263945190299,
-0.00901864652104168));
#32604=CARTESIAN_POINT('',(-0.210295596274888,0.0026140133424121,-0.00905923595863249));
#32605=CARTESIAN_POINT('',(-0.209093405037848,0.00261320592886496,-0.00903485853905873));
#32606=CARTESIAN_POINT('',(-0.210295595172847,0.00261401461120539,-0.00905923137572964));
#32607=CARTESIAN_POINT('',(-0.208994544730133,0.00749998715785556,-0.0104310930514343));
#32608=CARTESIAN_POINT('Ctrl Pts',(-0.209093403325743,0.00261320712931955,
-0.00903485617757382));
#32609=CARTESIAN_POINT('Ctrl Pts',(-0.209075287163041,0.00273078952585028,
-0.00910776338190552));
#32610=CARTESIAN_POINT('Ctrl Pts',(-0.209051803949458,0.00288667849406431,
-0.009199304375793));
#32611=CARTESIAN_POINT('Ctrl Pts',(-0.209025633252355,0.00306682577244403,
-0.00929887864898022));
#32612=CARTESIAN_POINT('Ctrl Pts',(-0.209013059146288,0.0031547547392515,
-0.00934630105910322));
#32613=CARTESIAN_POINT('Ctrl Pts',(-0.20898960376665,0.00332609194728352,
-0.00943518469474632));
#32614=CARTESIAN_POINT('Ctrl Pts',(-0.208964997943753,0.00351864509772977,
-0.00952966373552731));
#32615=CARTESIAN_POINT('Ctrl Pts',(-0.208939169709193,0.00373601100206904,
-0.00963068732037389));
#32616=CARTESIAN_POINT('Ctrl Pts',(-0.20890779757303,0.0040564040909896,
-0.00976582079672488));
#32617=CARTESIAN_POINT('Ctrl Pts',(-0.208879854701294,0.00443241802618406,
-0.00990888934421124));
#32618=CARTESIAN_POINT('Ctrl Pts',(-0.208860246398243,0.00496217141417863,
-0.0100805792723302));
#32619=CARTESIAN_POINT('Ctrl Pts',(-0.208863596164369,0.00545882350114872,
-0.0102036806673025));
#32620=CARTESIAN_POINT('Ctrl Pts',(-0.208877129956472,0.0058835563834354,
-0.0102877866011816));
#32621=CARTESIAN_POINT('Ctrl Pts',(-0.208894583868389,0.00622875777336524,
-0.0103424460616012));
#32622=CARTESIAN_POINT('Ctrl Pts',(-0.20891006127027,0.00646408490751225,
-0.0103715160371586));
#32623=CARTESIAN_POINT('Ctrl Pts',(-0.208925621038673,0.00667921457685546,
-0.0103934454631171));
#32624=CARTESIAN_POINT('Ctrl Pts',(-0.208940687029599,0.0068717606575439,
-0.0104087544437141));
#32625=CARTESIAN_POINT('Ctrl Pts',(-0.208949572232236,0.0069796541515509,
-0.0104155521292759));
#32626=CARTESIAN_POINT('Ctrl Pts',(-0.208967069010806,0.00718754014657644,
-0.0104263074860422));
#32627=CARTESIAN_POINT('Ctrl Pts',(-0.208982640861888,0.00736577272041199,
-0.0104308238271735));
#32628=CARTESIAN_POINT('Ctrl Pts',(-0.208994544730133,0.00749998715785556,
-0.0104310930514343));
#32629=CARTESIAN_POINT('',(-0.209093329064524,0.0123896542664875,-0.00903307101714839));
#32630=CARTESIAN_POINT('Ctrl Pts',(-0.208994544893321,0.00749998899777242,
-0.0104310930551249));
#32631=CARTESIAN_POINT('Ctrl Pts',(-0.208982705999951,0.00763413924716552,
-0.010430825647875));
#32632=CARTESIAN_POINT('Ctrl Pts',(-0.208967210984714,0.00781236163842383,
-0.0104263159156353));
#32633=CARTESIAN_POINT('Ctrl Pts',(-0.208949777667206,0.00802044089467235,
-0.0104155518224826));
#32634=CARTESIAN_POINT('Ctrl Pts',(-0.20894091592414,0.008128513175511,
-0.0104087429341645));
#32635=CARTESIAN_POINT('Ctrl Pts',(-0.208925867851496,0.00832154817731363,
-0.0103933857795959));
#32636=CARTESIAN_POINT('Ctrl Pts',(-0.2089103172045,0.00853716190381373,
-0.0103713854659244));
#32637=CARTESIAN_POINT('Ctrl Pts',(-0.208894824616601,0.00877315451964924,
-0.0103421906059869));
#32638=CARTESIAN_POINT('Ctrl Pts',(-0.208877320801299,0.00911860720596101,
-0.010287412183992));
#32639=CARTESIAN_POINT('Ctrl Pts',(-0.208863666216549,0.00954338077158189,
-0.0102031599596682));
#32640=CARTESIAN_POINT('Ctrl Pts',(-0.208860009499849,0.0100372452975142,
-0.0100807397059271));
#32641=CARTESIAN_POINT('Ctrl Pts',(-0.208879360438715,0.0105697164377529,
-0.00990816362194018));
#32642=CARTESIAN_POINT('Ctrl Pts',(-0.208907270581647,0.0109464746140233,
-0.00976466308937504));
#32643=CARTESIAN_POINT('Ctrl Pts',(-0.208938752514271,0.0112678251463805,
-0.00962896977344753));
#32644=CARTESIAN_POINT('Ctrl Pts',(-0.208964570384985,0.0114845683051079,
-0.00952811433689885));
#32645=CARTESIAN_POINT('Ctrl Pts',(-0.208989211407872,0.011676914863895,
-0.00943365116768143));
#32646=CARTESIAN_POINT('Ctrl Pts',(-0.209012698322003,0.0118479783561038,
-0.00934483474583016));
#32647=CARTESIAN_POINT('Ctrl Pts',(-0.209025311339803,0.0119359028386126,
-0.0092973790754351));
#32648=CARTESIAN_POINT('Ctrl Pts',(-0.209051564781441,0.0121160329579314,
-0.009197736640123));
#32649=CARTESIAN_POINT('Ctrl Pts',(-0.209075138847902,0.0122719973881306,
-0.00910608251841254));
#32650=CARTESIAN_POINT('Ctrl Pts',(-0.209093329064524,0.0123896542664875,
-0.00903307101714839));
#32651=CARTESIAN_POINT('',(-0.210295214238121,0.0123883927066978,-0.00905773115010187));
#32652=CARTESIAN_POINT('',(-0.209093329180995,0.012389650612435,-0.00903306515726067));
#32653=CARTESIAN_POINT('',(-0.210194950898403,0.00749992261723267,-0.0104582232103857));
#32654=CARTESIAN_POINT('Ctrl Pts',(-0.210295213170193,0.0123883913778837,
-0.00905772874839569));
#32655=CARTESIAN_POINT('Ctrl Pts',(-0.210276926508739,0.0122701560805008,
-0.00913127718769082));
#32656=CARTESIAN_POINT('Ctrl Pts',(-0.210253280898068,0.0121138705649328,
-0.0092233032752109));
#32657=CARTESIAN_POINT('Ctrl Pts',(-0.210226997140627,0.0119339996830231,
-0.00932299508710102));
#32658=CARTESIAN_POINT('Ctrl Pts',(-0.210214556449654,0.0118476323651082,
-0.00936972564086559));
#32659=CARTESIAN_POINT('Ctrl Pts',(-0.210190786792116,0.011675476606061,
-0.00945931840457171));
#32660=CARTESIAN_POINT('Ctrl Pts',(-0.210165940955667,0.0114828988779726,
-0.00955406939877045));
#32661=CARTESIAN_POINT('Ctrl Pts',(-0.210139924515179,0.0112666251945686,
-0.00965491597491719));
#32662=CARTESIAN_POINT('Ctrl Pts',(-0.210107923610646,0.0109445348858429,
-0.00979115138124437));
#32663=CARTESIAN_POINT('Ctrl Pts',(-0.210079602583789,0.010570125790686,
-0.00993398760550886));
#32664=CARTESIAN_POINT('Ctrl Pts',(-0.210059675792393,0.0100388881977446,
-0.0101066833814956));
#32665=CARTESIAN_POINT('Ctrl Pts',(-0.210063174055939,0.00954342433810476,
-0.0102298110037676));
#32666=CARTESIAN_POINT('Ctrl Pts',(-0.210076870548468,0.00911815800952164,
-0.0103143191211735));
#32667=CARTESIAN_POINT('Ctrl Pts',(-0.210094543901722,0.00877197614815612,
-0.0103692938412502));
#32668=CARTESIAN_POINT('Ctrl Pts',(-0.210110144111369,0.00853643895794477,
-0.0103984590221526));
#32669=CARTESIAN_POINT('Ctrl Pts',(-0.210125789774286,0.00832128382381539,
-0.0104204528663754));
#32670=CARTESIAN_POINT('Ctrl Pts',(-0.210140952603249,0.00812844154018853,
-0.0104358217663535));
#32671=CARTESIAN_POINT('Ctrl Pts',(-0.210149784035195,0.00802163519906834,
-0.0104425708482792));
#32672=CARTESIAN_POINT('Ctrl Pts',(-0.210167324477964,0.0078138027892246,
-0.0104533816768634));
#32673=CARTESIAN_POINT('Ctrl Pts',(-0.210182969923806,0.00763494796693094,
-0.0104579535863278));
#32674=CARTESIAN_POINT('Ctrl Pts',(-0.210194950908977,0.00749992286606277,
-0.0104582232242195));
#32675=CARTESIAN_POINT('Ctrl Pts',(-0.210194950886893,0.00749992261823137,
-0.0104582232237183));
#32676=CARTESIAN_POINT('Ctrl Pts',(-0.210182901046186,0.00736469672032039,
-0.0104579497398173));
#32677=CARTESIAN_POINT('Ctrl Pts',(-0.210172422497674,0.00724538734312025,
-0.0104548136618292));
#32678=CARTESIAN_POINT('Ctrl Pts',(-0.210163059345851,0.00713634177118728,
-0.0104502645999214));
#32679=CARTESIAN_POINT('Ctrl Pts',(-0.21015837776708,0.00708181895191274,
-0.010447990067578));
#32680=CARTESIAN_POINT('Ctrl Pts',(-0.21015397623712,0.00702986313799503,
-0.0104453092305155));
#32681=CARTESIAN_POINT('Ctrl Pts',(-0.210150307054415,0.00698617324694343,
-0.0104427721414516));
#32682=CARTESIAN_POINT('Ctrl Pts',(-0.210146637871711,0.00694248335589182,
-0.0104402350523877));
#32683=CARTESIAN_POINT('Ctrl Pts',(-0.210143698071857,0.00690705261103447,
-0.0104379729864375));
#32684=CARTESIAN_POINT('Ctrl Pts',(-0.210139683756397,0.00685708316826792,
-0.0104343707561762));
#32685=CARTESIAN_POINT('Ctrl Pts',(-0.210135669440937,0.00680711372550136,
-0.0104307685259148));
#32686=CARTESIAN_POINT('Ctrl Pts',(-0.210130585779747,0.0067426214917892,
-0.010425597011124));
#32687=CARTESIAN_POINT('Ctrl Pts',(-0.210126084760253,0.0066834609985755,
-0.0104202141619642));
#32688=CARTESIAN_POINT('Ctrl Pts',(-0.21012158374076,0.00662430050536181,
-0.0104148313128045));
#32689=CARTESIAN_POINT('Ctrl Pts',(-0.210117662082953,0.00657045706783954,
-0.0104093827532257));
#32690=CARTESIAN_POINT('Ctrl Pts',(-0.210114007159558,0.00651881912761199,
-0.010403757618497));
#32691=CARTESIAN_POINT('Ctrl Pts',(-0.210106697312767,0.0064155432471569,
-0.0103925073490395));
#32692=CARTESIAN_POINT('Ctrl Pts',(-0.21010045146602,0.00632108335076086,
-0.0103806806744025));
#32693=CARTESIAN_POINT('Ctrl Pts',(-0.21009441614451,0.0062164869318611,
-0.0103658243556338));
#32694=CARTESIAN_POINT('Ctrl Pts',(-0.210088380822999,0.00611189051296133,
-0.0103509680368652));
#32695=CARTESIAN_POINT('Ctrl Pts',(-0.21008256450481,0.00599720823621759,
-0.0103327046426888));
#32696=CARTESIAN_POINT('Ctrl Pts',(-0.210077972266854,0.00588684360592312,
-0.0103129973582448));
#32697=CARTESIAN_POINT('Ctrl Pts',(-0.210073380028898,0.00577647897562865,
-0.0102932900738008));
#32698=CARTESIAN_POINT('Ctrl Pts',(-0.210070007557372,0.0056703922517969,
-0.0102723324599391));
#32699=CARTESIAN_POINT('Ctrl Pts',(-0.210067545901141,0.00556669841361688,
-0.0102500722841563));
#32700=CARTESIAN_POINT('Ctrl Pts',(-0.210062622588677,0.00535931073725686,
-0.0102055519325907));
#32701=CARTESIAN_POINT('Ctrl Pts',(-0.210061335223825,0.0051614609530984,
-0.0101561444787735));
#32702=CARTESIAN_POINT('Ctrl Pts',(-0.210064745705541,0.00495583019273618,
-0.0100973149994839));
#32703=CARTESIAN_POINT('Ctrl Pts',(-0.210068156187256,0.00475019943237396,
-0.0100384855201942));
#32704=CARTESIAN_POINT('Ctrl Pts',(-0.210076286548203,0.00453705079573793,
-0.00996923671869086));
#32705=CARTESIAN_POINT('Ctrl Pts',(-0.210088476640698,0.00434154248511133,
-0.00989828957217904));
#32706=CARTESIAN_POINT('Ctrl Pts',(-0.210090891234621,0.00430281651325807,
-0.0098842364754586));
#32707=CARTESIAN_POINT('Ctrl Pts',(-0.210093464184377,0.00426477369336213,
-0.00987014248265051));
#32708=CARTESIAN_POINT('Ctrl Pts',(-0.210096245101527,0.00422668528530898,
-0.00985574713506132));
#32709=CARTESIAN_POINT('Ctrl Pts',(-0.210100483923172,0.00416862891046109,
-0.00983380498157101));
#32710=CARTESIAN_POINT('Ctrl Pts',(-0.210105205925359,0.00411046210709376,
-0.00981117299353445));
#32711=CARTESIAN_POINT('Ctrl Pts',(-0.210110586800972,0.00404967136736714,
-0.00978675728446723));
#32712=CARTESIAN_POINT('Ctrl Pts',(-0.210119497848536,0.00394899831486044,
-0.00974632342937738));
#32713=CARTESIAN_POINT('Ctrl Pts',(-0.210130223391488,0.00384123851543098,
-0.00970072961136996));
#32714=CARTESIAN_POINT('Ctrl Pts',(-0.210140763295786,0.00374438794995144,
-0.00965773465427805));
#32715=CARTESIAN_POINT('Ctrl Pts',(-0.210151303200083,0.00364753738447191,
-0.00961473969718614));
#32716=CARTESIAN_POINT('Ctrl Pts',(-0.210161648934644,0.0035614083089465,
-0.00957474870491259));
#32717=CARTESIAN_POINT('Ctrl Pts',(-0.21017334863502,0.00346865401672289,
-0.00952987258160654));
#32718=CARTESIAN_POINT('Ctrl Pts',(-0.210179198485208,0.00342227687061109,
-0.00950743451995351));
#32719=CARTESIAN_POINT('Ctrl Pts',(-0.210185387361134,0.00337425893918527,
-0.00948374876968531));
#32720=CARTESIAN_POINT('Ctrl Pts',(-0.210192421901137,0.00332158610454488,
-0.00945710265711653));
#32721=CARTESIAN_POINT('Ctrl Pts',(-0.21019945644114,0.00326891326990449,
-0.00943045654454775));
#32722=CARTESIAN_POINT('Ctrl Pts',(-0.210207339569676,0.00321165486863207,
-0.00940070981763388));
#32723=CARTESIAN_POINT('Ctrl Pts',(-0.210213348898254,0.00316869390487509,
-0.00937796337721139));
#32724=CARTESIAN_POINT('Ctrl Pts',(-0.210219358226833,0.00312573294111812,
-0.0093552169367889));
#32725=CARTESIAN_POINT('Ctrl Pts',(-0.210223489356426,0.00309695532981657,
-0.00933968458140724));
#32726=CARTESIAN_POINT('Ctrl Pts',(-0.210228826901985,0.00306007614923581,
-0.00931952500679846));
#32727=CARTESIAN_POINT('Ctrl Pts',(-0.210234164447545,0.00302319696865506,
-0.00929936543218968));
#32728=CARTESIAN_POINT('Ctrl Pts',(-0.210240710870133,0.00297828310429532,
-0.00927445811629131));
#32729=CARTESIAN_POINT('Ctrl Pts',(-0.21024769392878,0.00293099466147187,
-0.00924761742954498));
#32730=CARTESIAN_POINT('Ctrl Pts',(-0.210261660006699,0.00283641804245922,
-0.00919393620739263));
#32731=CARTESIAN_POINT('Ctrl Pts',(-0.210277368573352,0.00273222337063102,
-0.00913272268177796));
#32732=CARTESIAN_POINT('Ctrl Pts',(-0.210295594897407,0.00261401179386915,
-0.00905923810805346));
#32733=CARTESIAN_POINT('',(-0.194290184740893,0.00259891003340495,-0.00873469929757838));
#32734=CARTESIAN_POINT('',(-0.193089420205241,0.00259786897112515,-0.0087106653108531));
#32735=CARTESIAN_POINT('',(-0.194290183626354,0.00259891156440595,-0.0087346940896404));
#32736=CARTESIAN_POINT('',(-0.193001281131681,0.00750326240626864,-0.0100696314931372));
#32737=CARTESIAN_POINT('Ctrl Pts',(-0.193089417595358,0.00259787021585085,
-0.00871066257746708));
#32738=CARTESIAN_POINT('Ctrl Pts',(-0.193071520109316,0.00271737164203461,
-0.0087821698526072));
#32739=CARTESIAN_POINT('Ctrl Pts',(-0.193048393887614,0.00287523277332858,
-0.00887164272095586));
#32740=CARTESIAN_POINT('Ctrl Pts',(-0.193022765375995,0.003056792294895,
-0.00896856117898018));
#32741=CARTESIAN_POINT('Ctrl Pts',(-0.193010614506598,0.00314422540462343,
-0.00901413520726188));
#32742=CARTESIAN_POINT('Ctrl Pts',(-0.192987664968883,0.00331741658030568,
-0.00910097335122508));
#32743=CARTESIAN_POINT('Ctrl Pts',(-0.192963930400356,0.00351035925151311,
-0.00919259941855622));
#32744=CARTESIAN_POINT('Ctrl Pts',(-0.192928202941401,0.00382656270556843,
-0.00933427847044191));
#32745=CARTESIAN_POINT('Ctrl Pts',(-0.192887551610886,0.00433451593535043,
-0.00953365458093566));
#32746=CARTESIAN_POINT('Ctrl Pts',(-0.192868658917011,0.00496327969818103,
-0.0097289927725957));
#32747=CARTESIAN_POINT('Ctrl Pts',(-0.192873508297919,0.00544626414837375,
-0.00984654654740827));
#32748=CARTESIAN_POINT('Ctrl Pts',(-0.192886802235328,0.00582975166215757,
-0.00992002089963444));
#32749=CARTESIAN_POINT('Ctrl Pts',(-0.192896729854821,0.00604524879215619,
-0.00995568577848646));
#32750=CARTESIAN_POINT('Ctrl Pts',(-0.192907093637035,0.00623542839851351,
-0.00998317555330493));
#32751=CARTESIAN_POINT('Ctrl Pts',(-0.192913112747442,0.00633340690348751,
-0.00999574270740675));
#32752=CARTESIAN_POINT('Ctrl Pts',(-0.192924889956533,0.00651567014394898,
-0.0100174697902547));
#32753=CARTESIAN_POINT('Ctrl Pts',(-0.192949223880671,0.00685826224465497,
-0.0100505308306341));
#32754=CARTESIAN_POINT('Ctrl Pts',(-0.192978374135323,0.0072276364985116,
-0.0100692092264082));
#32755=CARTESIAN_POINT('Ctrl Pts',(-0.193001281131681,0.00750326240626864,
-0.0100696314931372));
#32756=CARTESIAN_POINT('',(-0.193087908899462,0.0124055063694067,-0.00870860190565759));
#32757=CARTESIAN_POINT('Ctrl Pts',(-0.193001281190772,0.00750326311727974,
-0.0100696314942265));
#32758=CARTESIAN_POINT('Ctrl Pts',(-0.192978210832965,0.00777866827952415,
-0.0100690146904097));
#32759=CARTESIAN_POINT('Ctrl Pts',(-0.192948830761218,0.008147788785168,
-0.0100501046519563));
#32760=CARTESIAN_POINT('Ctrl Pts',(-0.19292426502221,0.00849020464720827,
-0.0100168410848431));
#32761=CARTESIAN_POINT('Ctrl Pts',(-0.192912354662967,0.0086724362908473,
-0.00999500023200311));
#32762=CARTESIAN_POINT('Ctrl Pts',(-0.192906265760605,0.00877033231534428,
-0.00998238250180546));
#32763=CARTESIAN_POINT('Ctrl Pts',(-0.192895737826648,0.00896075376316357,
-0.00995473360888943));
#32764=CARTESIAN_POINT('Ctrl Pts',(-0.192885628503617,0.00917632356298331,
-0.00991891150020981));
#32765=CARTESIAN_POINT('Ctrl Pts',(-0.192872013216822,0.00955987628497917,
-0.00984514265529782));
#32766=CARTESIAN_POINT('Ctrl Pts',(-0.192866715571841,0.0100411414659507,
-0.00972773826890768));
#32767=CARTESIAN_POINT('Ctrl Pts',(-0.192885220267161,0.0106715812642055,
-0.0095314555019776));
#32768=CARTESIAN_POINT('Ctrl Pts',(-0.19292571236353,0.0111775914430577,
-0.00933246725911518));
#32769=CARTESIAN_POINT('Ctrl Pts',(-0.19296159843528,0.011493722472007,
-0.00919066330427862));
#32770=CARTESIAN_POINT('Ctrl Pts',(-0.192985458260683,0.0116864938887278,
-0.00909901104930757));
#32771=CARTESIAN_POINT('Ctrl Pts',(-0.193008563102243,0.0118596393209108,
-0.00901210051369803));
#32772=CARTESIAN_POINT('Ctrl Pts',(-0.193020768112869,0.0119467998890343,
-0.00896662056560247));
#32773=CARTESIAN_POINT('Ctrl Pts',(-0.19304656776878,0.0121281882483118,
-0.00886970079861718));
#32774=CARTESIAN_POINT('Ctrl Pts',(-0.193069867896834,0.0122859955607241,
-0.00878017895815907));
#32775=CARTESIAN_POINT('Ctrl Pts',(-0.193087908899462,0.0124055063694067,
-0.00870860190565759));
#32776=CARTESIAN_POINT('',(-0.194289761930591,0.0124043673425885,-0.00873272050667267));
#32777=CARTESIAN_POINT('',(-0.193087909024505,0.0124055025124637,-0.00870859549681853));
#32778=CARTESIAN_POINT('',(-0.194201350807346,0.00750361794929087,-0.0100967539450016));
#32779=CARTESIAN_POINT('Ctrl Pts',(-0.194289760087428,0.0124043660030698,
-0.00873271781171757));
#32780=CARTESIAN_POINT('Ctrl Pts',(-0.194271557560553,0.0122841918170491,
-0.00880489926922499));
#32781=CARTESIAN_POINT('Ctrl Pts',(-0.194255924507852,0.0121786813739423,
-0.00886479899873608));
#32782=CARTESIAN_POINT('Ctrl Pts',(-0.194242077346723,0.0120832044547145,
-0.00891719261876354));
#32783=CARTESIAN_POINT('Ctrl Pts',(-0.194235153737023,0.0120354657942032,
-0.00894338953902113));
#32784=CARTESIAN_POINT('Ctrl Pts',(-0.19422867761032,0.0119902062506205,
-0.00896765903205084));
#32785=CARTESIAN_POINT('Ctrl Pts',(-0.194223429540068,0.0119532774812538,
-0.00898718409458635));
#32786=CARTESIAN_POINT('Ctrl Pts',(-0.194218181469815,0.0119163487118872,
-0.00900670915712187));
#32787=CARTESIAN_POINT('Ctrl Pts',(-0.194214159033718,0.0118878153593697,
-0.00902161018266591));
#32788=CARTESIAN_POINT('Ctrl Pts',(-0.194208244185811,0.0118446120395155,
-0.00904374737452372));
#32789=CARTESIAN_POINT('Ctrl Pts',(-0.194202329337904,0.0118014087196613,
-0.00906588456638152));
#32790=CARTESIAN_POINT('Ctrl Pts',(-0.194194526447476,0.011743424062956,
-0.00909504257821868));
#32791=CARTESIAN_POINT('Ctrl Pts',(-0.194187615787879,0.0116903232532915,
-0.00912104827855453));
#32792=CARTESIAN_POINT('Ctrl Pts',(-0.194180705128282,0.011637222443627,
-0.00914705397889038));
#32793=CARTESIAN_POINT('Ctrl Pts',(-0.194174683690572,0.0115890759491422,
-0.00917005356254145));
#32794=CARTESIAN_POINT('Ctrl Pts',(-0.19416894561689,0.0115419790292713,
-0.00919212077082414));
#32795=CARTESIAN_POINT('Ctrl Pts',(-0.194157469469527,0.0114477851895296,
-0.00923625518738952));
#32796=CARTESIAN_POINT('Ctrl Pts',(-0.194147127099538,0.0113577901971368,
-0.00927664711652409));
#32797=CARTESIAN_POINT('Ctrl Pts',(-0.194137479955741,0.0112640004553303,
-0.00931699556663056));
#32798=CARTESIAN_POINT('Ctrl Pts',(-0.194119369196314,0.0110879272582998,
-0.00939274244969722));
#32799=CARTESIAN_POINT('Ctrl Pts',(-0.194103719839443,0.0108982588085448,
-0.00946782936055712));
#32800=CARTESIAN_POINT('Ctrl Pts',(-0.194092456058785,0.0107050027776539,
-0.00953690472670395));
#32801=CARTESIAN_POINT('Ctrl Pts',(-0.194091719976914,0.0106923736023294,
-0.00954141876388897));
#32802=CARTESIAN_POINT('Ctrl Pts',(-0.194091002623868,0.0106797294941558,
-0.00954590800925234));
#32803=CARTESIAN_POINT('Ctrl Pts',(-0.194090304536643,0.010667073418177,
-0.00955037138673742));
#32804=CARTESIAN_POINT('Ctrl Pts',(-0.194078924076026,0.0104607496681452,
-0.00962313491803084));
#32805=CARTESIAN_POINT('Ctrl Pts',(-0.194072662679182,0.0102511157066591,
-0.00968879287497787));
#32806=CARTESIAN_POINT('Ctrl Pts',(-0.194070598391485,0.0100500588759178,
-0.00974474285896947));
#32807=CARTESIAN_POINT('Ctrl Pts',(-0.194068534103787,0.00984900204517659,
-0.00980069284296108));
#32808=CARTESIAN_POINT('Ctrl Pts',(-0.194070648874117,0.00965676744371061,
-0.00984776204665912));
#32809=CARTESIAN_POINT('Ctrl Pts',(-0.194076567237035,0.00944655516440553,
-0.00989189619201452));
#32810=CARTESIAN_POINT('Ctrl Pts',(-0.194079526418495,0.009341449024753,
-0.00991396326469222));
#32811=CARTESIAN_POINT('Ctrl Pts',(-0.19408344128464,0.00923180464711715,
-0.0099350813053663));
#32812=CARTESIAN_POINT('Ctrl Pts',(-0.194088139064564,0.00912335820941506,
-0.00995400868302609));
#32813=CARTESIAN_POINT('Ctrl Pts',(-0.194090487954526,0.00906913499056402,
-0.00996347237185598));
#32814=CARTESIAN_POINT('Ctrl Pts',(-0.194093031522886,0.0090152195964702,
-0.00997243543958158));
#32815=CARTESIAN_POINT('Ctrl Pts',(-0.194096071829517,0.00895644906944938,
-0.00998163393309338));
#32816=CARTESIAN_POINT('Ctrl Pts',(-0.194099112136148,0.00889767854242856,
-0.00999083242660519));
#32817=CARTESIAN_POINT('Ctrl Pts',(-0.19410265263027,0.00883402824504551,
-0.0100001121226521));
#32818=CARTESIAN_POINT('Ctrl Pts',(-0.194105435828594,0.00878603171415256,
-0.0100067460210346));
#32819=CARTESIAN_POINT('Ctrl Pts',(-0.194108219026918,0.0087380351832596,
-0.010013379919417));
#32820=CARTESIAN_POINT('Ctrl Pts',(-0.194110240099272,0.00870572131166556,
-0.0100175833341403));
#32821=CARTESIAN_POINT('Ctrl Pts',(-0.194112740675617,0.00866684824967951,
-0.0100224633622123));
#32822=CARTESIAN_POINT('Ctrl Pts',(-0.194115241251962,0.00862797518769346,
-0.0100273433902844));
#32823=CARTESIAN_POINT('Ctrl Pts',(-0.194118223924051,0.00858252925364297,
-0.0100327846897015));
#32824=CARTESIAN_POINT('Ctrl Pts',(-0.194121383971891,0.00853594848017848,
-0.0100379828379812));
#32825=CARTESIAN_POINT('Ctrl Pts',(-0.194127704067573,0.0084427869332495,
-0.0100483791345406));
#32826=CARTESIAN_POINT('Ctrl Pts',(-0.194134730458665,0.00834509945083744,
-0.0100579452337754));
#32827=CARTESIAN_POINT('Ctrl Pts',(-0.194142685912192,0.00823888424106794,
-0.0100664533359255));
#32828=CARTESIAN_POINT('Ctrl Pts',(-0.194158596817806,0.00802645384076312,
-0.010083469538685));
#32829=CARTESIAN_POINT('Ctrl Pts',(-0.194178226891711,0.00777991114448582,
-0.0100961249381803));
#32830=CARTESIAN_POINT('Ctrl Pts',(-0.194201351177526,0.00750361798025657,
-0.0100967539377924));
#32831=CARTESIAN_POINT('Ctrl Pts',(-0.194201351183807,0.00750361790520686,
-0.0100967539379632));
#32832=CARTESIAN_POINT('Ctrl Pts',(-0.1941784036171,0.00722720869209292,
-0.0100963417181278));
#32833=CARTESIAN_POINT('Ctrl Pts',(-0.19415892327886,0.00698052577256948,
-0.0100838676069228));
#32834=CARTESIAN_POINT('Ctrl Pts',(-0.194143133295327,0.00676793924744402,
-0.0100669960050715));
#32835=CARTESIAN_POINT('Ctrl Pts',(-0.194135238303561,0.00666164598488129,
-0.0100585602041459));
#32836=CARTESIAN_POINT('Ctrl Pts',(-0.194128265168655,0.0065638764940593,
-0.0100490573230068));
#32837=CARTESIAN_POINT('Ctrl Pts',(-0.194121992959818,0.00647062775368298,
-0.010038718058705));
#32838=CARTESIAN_POINT('Ctrl Pts',(-0.194118856855399,0.00642400338349483,
-0.0100335484265541));
#32839=CARTESIAN_POINT('Ctrl Pts',(-0.194115896785519,0.00637851253535828,
-0.0100281340490187));
#32840=CARTESIAN_POINT('Ctrl Pts',(-0.194113414944245,0.00633959584073668,
-0.0100232759418804));
#32841=CARTESIAN_POINT('Ctrl Pts',(-0.194110933102972,0.00630067914611507,
-0.0100184178347421));
#32842=CARTESIAN_POINT('Ctrl Pts',(-0.194108926894298,0.00626832298245323,
-0.0100142315214387));
#32843=CARTESIAN_POINT('Ctrl Pts',(-0.194106165030128,0.00622027508395902,
-0.0100076237304598));
#32844=CARTESIAN_POINT('Ctrl Pts',(-0.194103403165958,0.0061722271854648,
-0.010001015939481));
#32845=CARTESIAN_POINT('Ctrl Pts',(-0.194099890484652,0.00610851634466332,
-0.00999177100812512));
#32846=CARTESIAN_POINT('Ctrl Pts',(-0.194096874427416,0.00604969047262855,
-0.00998260367179467));
#32847=CARTESIAN_POINT('Ctrl Pts',(-0.194093858370181,0.00599086460059379,
-0.00997343633546422));
#32848=CARTESIAN_POINT('Ctrl Pts',(-0.194091335481784,0.00593689912204222,
-0.00996450107264417));
#32849=CARTESIAN_POINT('Ctrl Pts',(-0.194089006191789,0.00588262685159719,
-0.00995506487481372));
#32850=CARTESIAN_POINT('Ctrl Pts',(-0.194084347611799,0.00577408231070712,
-0.00993619247915282));
#32851=CARTESIAN_POINT('Ctrl Pts',(-0.194080467634741,0.00566434390043965,
-0.00991512777454408));
#32852=CARTESIAN_POINT('Ctrl Pts',(-0.194077536821785,0.00555915963491658,
-0.00989311214193168));
#32853=CARTESIAN_POINT('Ctrl Pts',(-0.194071675195875,0.00534879110387044,
-0.00984908087670686));
#32854=CARTESIAN_POINT('Ctrl Pts',(-0.194069591003107,0.00515646375103136,
-0.00980211034402297));
#32855=CARTESIAN_POINT('Ctrl Pts',(-0.194071666486789,0.00495527116389036,
-0.00974624901355076));
#32856=CARTESIAN_POINT('Ctrl Pts',(-0.19407374197047,0.00475407857674936,
-0.00969038768307855));
#32857=CARTESIAN_POINT('Ctrl Pts',(-0.194079995256821,0.00454426636275194,
-0.00962480503332397));
#32858=CARTESIAN_POINT('Ctrl Pts',(-0.19409134999362,0.00433775402585064,
-0.00955210057146974));
#32859=CARTESIAN_POINT('Ctrl Pts',(-0.194092134644621,0.00432348331974186,
-0.00954707644543695));
#32860=CARTESIAN_POINT('Ctrl Pts',(-0.194092943662198,0.00430922775133401,
-0.00954201941471674));
#32861=CARTESIAN_POINT('Ctrl Pts',(-0.194093776278021,0.0042949915867727,
-0.0095369310292579));
#32862=CARTESIAN_POINT('Ctrl Pts',(-0.194104992501138,0.00410321526746275,
-0.00946838505043592));
#32863=CARTESIAN_POINT('Ctrl Pts',(-0.194120491089499,0.00391504859850539,
-0.00939394859554914));
#32864=CARTESIAN_POINT('Ctrl Pts',(-0.194138393795351,0.00374031506574058,
-0.00931887929995244));
#32865=CARTESIAN_POINT('Ctrl Pts',(-0.194148009635601,0.00364646278713287,
-0.00927855833617551));
#32866=CARTESIAN_POINT('Ctrl Pts',(-0.194158315848446,0.0035564231592988,
-0.00923819860106988));
#32867=CARTESIAN_POINT('Ctrl Pts',(-0.194169754463968,0.0034621532928448,
-0.00919408287663085));
#32868=CARTESIAN_POINT('Ctrl Pts',(-0.194175473771729,0.0034150183596178,
-0.00917202501441133));
#32869=CARTESIAN_POINT('Ctrl Pts',(-0.194181476100521,0.0033668260329514,
-0.00914903136473678));
#32870=CARTESIAN_POINT('Ctrl Pts',(-0.194188366540259,0.00331365880698595,
-0.0091230233186226));
#32871=CARTESIAN_POINT('Ctrl Pts',(-0.194195256979996,0.0032604915810205,
-0.00909701527250842));
#32872=CARTESIAN_POINT('Ctrl Pts',(-0.194203038554286,0.00320242016548369,
-0.00906784595621892));
#32873=CARTESIAN_POINT('Ctrl Pts',(-0.194208933111204,0.00315918193490789,
-0.00904571485433129));
#32874=CARTESIAN_POINT('Ctrl Pts',(-0.194214827668121,0.00311594370433209,
-0.00902358375244366));
#32875=CARTESIAN_POINT('Ctrl Pts',(-0.194218830819376,0.00308742695170646,
-0.00900870709690693));
#32876=CARTESIAN_POINT('Ctrl Pts',(-0.194224058435703,0.0030504868152752,
-0.00898919675401521));
#32877=CARTESIAN_POINT('Ctrl Pts',(-0.19422928605203,0.00301354667884394,
-0.00896968641112348));
#32878=CARTESIAN_POINT('Ctrl Pts',(-0.194235740564667,0.00296824795435302,
-0.00894542157318903));
#32879=CARTESIAN_POINT('Ctrl Pts',(-0.194242641940655,0.00292046237651401,
-0.00891922568503443));
#32880=CARTESIAN_POINT('Ctrl Pts',(-0.194256444653212,0.00282489149378098,
-0.00886683405835275));
#32881=CARTESIAN_POINT('Ctrl Pts',(-0.194272030765503,0.00271925573908181,
-0.0088069226691576));
#32882=CARTESIAN_POINT('Ctrl Pts',(-0.194290183336391,0.00259890843439175,
-0.00873470160911481));
#32883=CARTESIAN_POINT('',(-0.214298629851053,0.00261569271051004,-0.00914002418897946));
#32884=CARTESIAN_POINT('',(-0.213096481634368,0.00261552650153193,-0.00911594495457058));
#32885=CARTESIAN_POINT('',(-0.214298628831032,0.00261569386335166,-0.00914002001605525));
#32886=CARTESIAN_POINT('',(-0.212993232294335,0.0075001970402567,-0.0105214666975835));
#32887=CARTESIAN_POINT('Ctrl Pts',(-0.21309648029403,0.00261552762645514,
-0.00911594282477631));
#32888=CARTESIAN_POINT('Ctrl Pts',(-0.213078430112302,0.00273245414128495,
-0.00918906108432047));
#32889=CARTESIAN_POINT('Ctrl Pts',(-0.213054995693056,0.00288771851498538,
-0.0092810210476475));
#32890=CARTESIAN_POINT('Ctrl Pts',(-0.21302880695443,0.00306756366400709,
-0.00938127103149015));
#32891=CARTESIAN_POINT('Ctrl Pts',(-0.213016143252952,0.00315590799634756,
-0.00942930968362297));
#32892=CARTESIAN_POINT('Ctrl Pts',(-0.212992660269334,0.003326786139957,
-0.00951867735662309));
#32893=CARTESIAN_POINT('Ctrl Pts',(-0.21296791706596,0.0035191922936703,
-0.00961383729171739));
#32894=CARTESIAN_POINT('Ctrl Pts',(-0.212941949550837,0.00373557892325479,
-0.00971524319924369));
#32895=CARTESIAN_POINT('Ctrl Pts',(-0.212909725136388,0.00405845154500544,
-0.0098524131824994));
#32896=CARTESIAN_POINT('Ctrl Pts',(-0.212881015567256,0.00443089820167271,
-0.00999509170778643));
#32897=CARTESIAN_POINT('Ctrl Pts',(-0.212859850566388,0.00496168574833953,
-0.0101685244860136));
#32898=CARTESIAN_POINT('Ctrl Pts',(-0.212862265028007,0.00545958577045319,
-0.0102927065215424));
#32899=CARTESIAN_POINT('Ctrl Pts',(-0.212875146008631,0.0058842422052161,
-0.0103772957691917));
#32900=CARTESIAN_POINT('Ctrl Pts',(-0.212892085155633,0.00622799509361403,
-0.0104320981575625));
#32901=CARTESIAN_POINT('Ctrl Pts',(-0.212907529886643,0.00646460503686682,
-0.0104615313468541));
#32902=CARTESIAN_POINT('Ctrl Pts',(-0.212923143490097,0.00667948099614421,
-0.0104835687423165));
#32903=CARTESIAN_POINT('Ctrl Pts',(-0.212938368518025,0.00687187013964289,
-0.010498964812566));
#32904=CARTESIAN_POINT('Ctrl Pts',(-0.212947295699535,0.00697855992041427,
-0.010505738088064));
#32905=CARTESIAN_POINT('Ctrl Pts',(-0.212965076377683,0.00718624194132101,
-0.0105165930048715));
#32906=CARTESIAN_POINT('Ctrl Pts',(-0.212981009572996,0.00736511552634172,
-0.0105211933895291));
#32907=CARTESIAN_POINT('Ctrl Pts',(-0.212993232294335,0.0075001970402567,
-0.0105214666975835));
#32908=CARTESIAN_POINT('',(-0.21309504262537,0.0123853440218161,-0.00911536634304113));
#32909=CARTESIAN_POINT('Ctrl Pts',(-0.212993232518998,0.00750019952315436,
-0.0105214667026068));
#32910=CARTESIAN_POINT('Ctrl Pts',(-0.212981061653907,0.00763520971852247,
-0.0105211886623164));
#32911=CARTESIAN_POINT('Ctrl Pts',(-0.212965184756485,0.00781408229962534,
-0.0105165863100814));
#32912=CARTESIAN_POINT('Ctrl Pts',(-0.212947437584023,0.00802198453578981,
-0.0105057108565127));
#32913=CARTESIAN_POINT('Ctrl Pts',(-0.212938511769387,0.00812893139569496,
-0.0104989147874754));
#32914=CARTESIAN_POINT('Ctrl Pts',(-0.212923276308821,0.00832174278934911,
-0.010483464014518));
#32915=CARTESIAN_POINT('Ctrl Pts',(-0.212907629501198,0.00853704573621329,
-0.0104613497492999));
#32916=CARTESIAN_POINT('Ctrl Pts',(-0.21289211318811,0.00877418254637154,
-0.0104317971122061));
#32917=CARTESIAN_POINT('Ctrl Pts',(-0.212875016315916,0.00911806924975992,
-0.0103768834350925));
#32918=CARTESIAN_POINT('Ctrl Pts',(-0.212861881278273,0.0095425186563387,
-0.0102921897492956));
#32919=CARTESIAN_POINT('Ctrl Pts',(-0.212858990654386,0.0100372170775486,
-0.0101688017016576));
#32920=CARTESIAN_POINT('Ctrl Pts',(-0.212879702219452,0.0105702101667965,
-0.00999470542822341));
#32921=CARTESIAN_POINT('Ctrl Pts',(-0.212908308029409,0.0109434177167843,
-0.00985163308745656));
#32922=CARTESIAN_POINT('Ctrl Pts',(-0.212940513214306,0.011266746511133,
-0.00971416489421704));
#32923=CARTESIAN_POINT('Ctrl Pts',(-0.212966407470973,0.0114824337087737,
-0.00961301708601186));
#32924=CARTESIAN_POINT('Ctrl Pts',(-0.212991121561868,0.0116744958348988,
-0.00951798776478114));
#32925=CARTESIAN_POINT('Ctrl Pts',(-0.213014577453931,0.0118449807481599,
-0.00942879779089917));
#32926=CARTESIAN_POINT('Ctrl Pts',(-0.213027252935726,0.0119332823145633,
-0.00938077251897972));
#32927=CARTESIAN_POINT('Ctrl Pts',(-0.213053470144755,0.012113045655154,
-0.00928054494139649));
#32928=CARTESIAN_POINT('Ctrl Pts',(-0.213076951250776,0.0122683567168384,
-0.00918853996606421));
#32929=CARTESIAN_POINT('Ctrl Pts',(-0.21309504262537,0.0123853440218161,
-0.00911536634304113));
#32930=CARTESIAN_POINT('',(-0.214296931244579,0.0123846052054983,-0.00913980847830293));
#32931=CARTESIAN_POINT('',(-0.213095042734061,0.0123853405995523,-0.00911536089812739));
#32932=CARTESIAN_POINT('',(-0.214193730601714,0.00750035257190656,-0.0105485989207064));
#32933=CARTESIAN_POINT('Ctrl Pts',(-0.214296930448721,0.0123846039446203,
-0.0091398062710915));
#32934=CARTESIAN_POINT('Ctrl Pts',(-0.214278721771776,0.0122668959833074,
-0.00921361292919597));
#32935=CARTESIAN_POINT('Ctrl Pts',(-0.214263005072048,0.0121629773635556,
-0.00927519657157546));
#32936=CARTESIAN_POINT('Ctrl Pts',(-0.21424900854385,0.0120685001738844,
-0.00932927853847729));
#32937=CARTESIAN_POINT('Ctrl Pts',(-0.214242010247462,0.0120212613610989,
-0.00935631964669018));
#32938=CARTESIAN_POINT('Ctrl Pts',(-0.214235443009659,0.0119763528144547,
-0.00938143520479044));
#32939=CARTESIAN_POINT('Ctrl Pts',(-0.214230075611608,0.0119393872627358,
-0.00940181100398319));
#32940=CARTESIAN_POINT('Ctrl Pts',(-0.214224708213557,0.0119024217110168,
-0.00942218680317593));
#32941=CARTESIAN_POINT('Ctrl Pts',(-0.214220538178746,0.011873466807046,
-0.00943794372517518));
#32942=CARTESIAN_POINT('Ctrl Pts',(-0.214214494776839,0.0118304283104676,
-0.00946091659507249));
#32943=CARTESIAN_POINT('Ctrl Pts',(-0.214208451374932,0.0117873898138891,
-0.00948388946496979));
#32944=CARTESIAN_POINT('Ctrl Pts',(-0.214200539028783,0.0117301524518821,
-0.00951386398846413));
#32945=CARTESIAN_POINT('Ctrl Pts',(-0.214193469042124,0.0116774632250146,
-0.00954073002665238));
#32946=CARTESIAN_POINT('Ctrl Pts',(-0.214186399055465,0.011624773998147,
-0.00956759606484063));
#32947=CARTESIAN_POINT('Ctrl Pts',(-0.214180168492324,0.0115767028581632,
-0.00959149404375981));
#32948=CARTESIAN_POINT('Ctrl Pts',(-0.21417427591499,0.0115302697149787,
-0.00961413300801649));
#32949=CARTESIAN_POINT('Ctrl Pts',(-0.214162490760321,0.0114374034286095,
-0.00965941093652985));
#32950=CARTESIAN_POINT('Ctrl Pts',(-0.214152055361112,0.0113511529333559,
-0.00969976052723715));
#32951=CARTESIAN_POINT('Ctrl Pts',(-0.214141387483464,0.0112541405327512,
-0.00974314176318902));
#32952=CARTESIAN_POINT('Ctrl Pts',(-0.214130719605816,0.0111571281321464,
-0.00978652299914088));
#32953=CARTESIAN_POINT('Ctrl Pts',(-0.214119828009397,0.0110491600093937,
-0.00983252088936748));
#32954=CARTESIAN_POINT('Ctrl Pts',(-0.214110763409328,0.0109487202024644,
-0.00987313923237703));
#32955=CARTESIAN_POINT('Ctrl Pts',(-0.214105855700514,0.010894340602476,
-0.00989513060524584));
#32956=CARTESIAN_POINT('Ctrl Pts',(-0.21410148123821,0.0108422001052795,
-0.00991562376018389));
#32957=CARTESIAN_POINT('Ctrl Pts',(-0.214097508592728,0.0107903940484817,
-0.00993546403750088));
#32958=CARTESIAN_POINT('Ctrl Pts',(-0.214094143711908,0.0107465136650769,
-0.00995226900258296));
#32959=CARTESIAN_POINT('Ctrl Pts',(-0.214091067106676,0.0107028718786788,
-0.00996860292194799));
#32960=CARTESIAN_POINT('Ctrl Pts',(-0.214088198910818,0.01065827961437,
-0.00998489994682812));
#32961=CARTESIAN_POINT('Ctrl Pts',(-0.214075690020502,0.0104638020505384,
-0.0100559751825337));
#32962=CARTESIAN_POINT('Ctrl Pts',(-0.21406716976087,0.0102510002344298,
-0.0101256466000661));
#32963=CARTESIAN_POINT('Ctrl Pts',(-0.214063472264175,0.0100454113775732,
-0.0101848993120509));
#32964=CARTESIAN_POINT('Ctrl Pts',(-0.214059774767479,0.00983982252071662,
-0.0102441520240357));
#32965=CARTESIAN_POINT('Ctrl Pts',(-0.214060877726939,0.00964171398316327,
-0.0102939948760628));
#32966=CARTESIAN_POINT('Ctrl Pts',(-0.214065644163786,0.00943396330360745,
-0.0103389073683293));
#32967=CARTESIAN_POINT('Ctrl Pts',(-0.21406802738221,0.00933008796382954,
-0.0103613636144626));
#32968=CARTESIAN_POINT('Ctrl Pts',(-0.214071328264685,0.00922379415886723,
-0.0103825080238672));
#32969=CARTESIAN_POINT('Ctrl Pts',(-0.21407585910803,0.00911310620040166,
-0.0104024031717887));
#32970=CARTESIAN_POINT('Ctrl Pts',(-0.214080389951375,0.00900241824193609,
-0.0104222983197102));
#32971=CARTESIAN_POINT('Ctrl Pts',(-0.214086155225572,0.00888729480678718,
-0.0104407437416028));
#32972=CARTESIAN_POINT('Ctrl Pts',(-0.214092160048566,0.0087824703095477,
-0.0104557182416041));
#32973=CARTESIAN_POINT('Ctrl Pts',(-0.21409816487156,0.00867764581230821,
-0.0104706927416053));
#32974=CARTESIAN_POINT('Ctrl Pts',(-0.21410440059583,0.00858317218749535,
-0.0104825812100531));
#32975=CARTESIAN_POINT('Ctrl Pts',(-0.214111730246791,0.00848006693797604,
-0.0104938751473267));
#32976=CARTESIAN_POINT('Ctrl Pts',(-0.214115395072272,0.00842851431321638,
-0.0104995221159635));
#32977=CARTESIAN_POINT('Ctrl Pts',(-0.214119334123338,0.00837480225013233,
-0.0105049875567496));
#32978=CARTESIAN_POINT('Ctrl Pts',(-0.214123864686976,0.00831582647206328,
-0.0105103853131636));
#32979=CARTESIAN_POINT('Ctrl Pts',(-0.214128395250614,0.00825685069399423,
-0.0105157830695775));
#32980=CARTESIAN_POINT('Ctrl Pts',(-0.21413352061064,0.00819259641006701,
-0.0105209673652426));
#32981=CARTESIAN_POINT('Ctrl Pts',(-0.214137565354542,0.00814289901357351,
-0.0105245745801381));
#32982=CARTESIAN_POINT('Ctrl Pts',(-0.214141610098444,0.00809320161708002,
-0.0105281817950336));
#32983=CARTESIAN_POINT('Ctrl Pts',(-0.214144569038739,0.00805807717990574,
-0.0105304418179341));
#32984=CARTESIAN_POINT('Ctrl Pts',(-0.214148279134351,0.00801458612955796,
-0.0105329887781426));
#32985=CARTESIAN_POINT('Ctrl Pts',(-0.214151989229963,0.00797109507921019,
-0.0105355357383511));
#32986=CARTESIAN_POINT('Ctrl Pts',(-0.214156453463961,0.00791923052684874,
-0.0105382375369189));
#32987=CARTESIAN_POINT('Ctrl Pts',(-0.214161211273031,0.00786472646875704,
-0.0105405341258496));
#32988=CARTESIAN_POINT('Ctrl Pts',(-0.214170726891171,0.00775571835257365,
-0.0105451273037108));
#32989=CARTESIAN_POINT('Ctrl Pts',(-0.214181411936434,0.00763615658959353,
-0.0105483152401436));
#32990=CARTESIAN_POINT('Ctrl Pts',(-0.214193730627006,0.00750035314621932,
-0.0105485989486921));
#32991=CARTESIAN_POINT('Ctrl Pts',(-0.214193730574935,0.00750035257429044,
-0.0105485989475376));
#32992=CARTESIAN_POINT('Ctrl Pts',(-0.214181345616963,0.00736432013461061,
-0.0105483243338446));
#32993=CARTESIAN_POINT('Ctrl Pts',(-0.214170615447453,0.00724467154441374,
-0.0105451359586704));
#32994=CARTESIAN_POINT('Ctrl Pts',(-0.214161069591025,0.0071356472345695,
-0.0105405459272893));
#32995=CARTESIAN_POINT('Ctrl Pts',(-0.214156296656122,0.00708113500325122,
-0.0105382509083823));
#32996=CARTESIAN_POINT('Ctrl Pts',(-0.214151821033651,0.00702927995572575,
-0.0105355509097294));
#32997=CARTESIAN_POINT('Ctrl Pts',(-0.214148109500974,0.00698588746795613,
-0.0105330117591464));
#32998=CARTESIAN_POINT('Ctrl Pts',(-0.214144397968298,0.00694249498018651,
-0.0105304726085634));
#32999=CARTESIAN_POINT('Ctrl Pts',(-0.214141447512222,0.00690755810329318,
-0.0105282277386009));
#33000=CARTESIAN_POINT('Ctrl Pts',(-0.214137396362883,0.0068578514447973,
-0.0105246238289852));
#33001=CARTESIAN_POINT('Ctrl Pts',(-0.214133345213544,0.00680814478630143,
-0.0105210199193695));
#33002=CARTESIAN_POINT('Ctrl Pts',(-0.214128198626389,0.00674368458937078,
-0.0105158240713284));
#33003=CARTESIAN_POINT('Ctrl Pts',(-0.214123657729659,0.00668457551066981,
-0.0105104167347357));
#33004=CARTESIAN_POINT('Ctrl Pts',(-0.214119116832928,0.00662546643196883,
-0.0105050093981429));
#33005=CARTESIAN_POINT('Ctrl Pts',(-0.214115178280762,0.00657169344874913,
-0.0104995391005902));
#33006=CARTESIAN_POINT('Ctrl Pts',(-0.214111515099688,0.00652003053578507,
-0.0104938808240976));
#33007=CARTESIAN_POINT('Ctrl Pts',(-0.214104188737539,0.00641670470985695,
-0.0104825642711124));
#33008=CARTESIAN_POINT('Ctrl Pts',(-0.214097961137331,0.00632181412899653,
-0.0104706161469304));
#33009=CARTESIAN_POINT('Ctrl Pts',(-0.214092017849508,0.00621714983984993,
-0.0104556612666314));
#33010=CARTESIAN_POINT('Ctrl Pts',(-0.214086074561685,0.00611248555070334,
-0.0104407063863325));
#33011=CARTESIAN_POINT('Ctrl Pts',(-0.214080423805992,0.00599809690955629,
-0.010422378897594));
#33012=CARTESIAN_POINT('Ctrl Pts',(-0.214075994597286,0.00588787166133225,
-0.0104025810141776));
#33013=CARTESIAN_POINT('Ctrl Pts',(-0.214071565388579,0.0057776464131082,
-0.0103827831307611));
#33014=CARTESIAN_POINT('Ctrl Pts',(-0.214068353557564,0.0056715458111831,
-0.0103617018577092));
#33015=CARTESIAN_POINT('Ctrl Pts',(-0.214066060271609,0.00556779765735659,
-0.0103392962444784));
#33016=CARTESIAN_POINT('Ctrl Pts',(-0.2140614736997,0.00536030134970358,
-0.0102944850180168));
#33017=CARTESIAN_POINT('Ctrl Pts',(-0.214060553859486,0.00516218037746964,
-0.0102447055306988));
#33018=CARTESIAN_POINT('Ctrl Pts',(-0.214064458399895,0.00495623279761624,
-0.0101853953614391));
#33019=CARTESIAN_POINT('Ctrl Pts',(-0.214068362940304,0.00475028521776285,
-0.0101260851921794));
#33020=CARTESIAN_POINT('Ctrl Pts',(-0.214077114659975,0.00453678428426086,
-0.0100562132639311));
#33021=CARTESIAN_POINT('Ctrl Pts',(-0.214089782012679,0.004342031475676,
-0.00998504834678421));
#33022=CARTESIAN_POINT('Ctrl Pts',(-0.214092690231091,0.00429731939438625,
-0.00996871003780899));
#33023=CARTESIAN_POINT('Ctrl Pts',(-0.214095803503907,0.00425358214047101,
-0.00995234173959868));
#33024=CARTESIAN_POINT('Ctrl Pts',(-0.214099204596534,0.00420959871191655,
-0.00993549782678036));
#33025=CARTESIAN_POINT('Ctrl Pts',(-0.21410321058855,0.00415779263576576,
-0.00991565814945591));
#33026=CARTESIAN_POINT('Ctrl Pts',(-0.214107615884805,0.00410564313783565,
-0.00989516236796775));
#33027=CARTESIAN_POINT('Ctrl Pts',(-0.214112555731078,0.00405120821435422,
-0.00987314859199749));
#33028=CARTESIAN_POINT('Ctrl Pts',(-0.214121689513501,0.00395055796738748,
-0.00983244509052506));
#33029=CARTESIAN_POINT('Ctrl Pts',(-0.214132658894906,0.00384220786214466,
-0.00978627536711066));
#33030=CARTESIAN_POINT('Ctrl Pts',(-0.214143350697998,0.00374517508066676,
-0.00974287572751151));
#33031=CARTESIAN_POINT('Ctrl Pts',(-0.214154042501091,0.00364814229918887,
-0.00969947608791235));
#33032=CARTESIAN_POINT('Ctrl Pts',(-0.21416444770987,0.00356222737904924,
-0.00965927365907892));
#33033=CARTESIAN_POINT('Ctrl Pts',(-0.21417620969836,0.00346954930648967,
-0.00961408480996121));
#33034=CARTESIAN_POINT('Ctrl Pts',(-0.214182090692604,0.0034232102702099,
-0.00959149038540235));
#33035=CARTESIAN_POINT('Ctrl Pts',(-0.214188311461854,0.00337519720913805,
-0.00956762083501447));
#33036=CARTESIAN_POINT('Ctrl Pts',(-0.21419536566459,0.00332258178985352,
-0.00954079257226103));
#33037=CARTESIAN_POINT('Ctrl Pts',(-0.214202419867326,0.00326996637056899,
-0.0095139643095076));
#33038=CARTESIAN_POINT('Ctrl Pts',(-0.214210310421654,0.00321281808848199,
-0.00948403777143926));
#33039=CARTESIAN_POINT('Ctrl Pts',(-0.214216339274854,0.00316982536706485,
-0.00946109081517068));
#33040=CARTESIAN_POINT('Ctrl Pts',(-0.214222368128053,0.00312683264564772,
-0.00943814385890211));
#33041=CARTESIAN_POINT('Ctrl Pts',(-0.214226530873441,0.00309788065642511,
-0.0094223899883824));
#33042=CARTESIAN_POINT('Ctrl Pts',(-0.214231888387702,0.00306092283807243,
-0.00940202005736926));
#33043=CARTESIAN_POINT('Ctrl Pts',(-0.214237245901962,0.00302396501971975,
-0.00938165012635613));
#33044=CARTESIAN_POINT('Ctrl Pts',(-0.214243800654996,0.00297906883286363,
-0.00935654357939838));
#33045=CARTESIAN_POINT('Ctrl Pts',(-0.214250786332799,0.00293183529864835,
-0.00932950779425316));
#33046=CARTESIAN_POINT('Ctrl Pts',(-0.214264757651952,0.00283736847668207,
-0.00927543636503528));
#33047=CARTESIAN_POINT('Ctrl Pts',(-0.214280448620716,0.00273343208000158,
-0.00921384815061718));
#33048=CARTESIAN_POINT('Ctrl Pts',(-0.214298628577443,0.00261569126736467,
-0.0091400261770453));
#33049=CARTESIAN_POINT('',(-0.224520431112711,0.00173717640815345,-0.00870165576114943));
#33050=CARTESIAN_POINT('',(-0.223316843015392,0.00173498433150003,-0.00867730364596437));
#33051=CARTESIAN_POINT('',(-0.223316842847435,0.00173497690009322,-0.00867731262527063));
#33052=CARTESIAN_POINT('',(-0.222880624396322,0.00442263472015358,-0.0102052666341114));
#33053=CARTESIAN_POINT('Ctrl Pts',(-0.223316843015392,0.00173498433150003,
-0.00867730364596437));
#33054=CARTESIAN_POINT('Ctrl Pts',(-0.223279812530346,0.00186517669334324,
-0.00878435058928567));
#33055=CARTESIAN_POINT('Ctrl Pts',(-0.223232277207935,0.00203819990847103,
-0.00891798594929538));
#33056=CARTESIAN_POINT('Ctrl Pts',(-0.223180379664801,0.00223735359889598,
-0.00906189282015912));
#33057=CARTESIAN_POINT('Ctrl Pts',(-0.223156273797957,0.00233181413205371,
-0.00912841520280122));
#33058=CARTESIAN_POINT('Ctrl Pts',(-0.223110681833087,0.00252272373509083,
-0.00925731540364347));
#33059=CARTESIAN_POINT('Ctrl Pts',(-0.223064310367951,0.00273688688368519,
-0.00939387105231042));
#33060=CARTESIAN_POINT('Ctrl Pts',(-0.223014089616156,0.00300235697175274,
-0.00955231904645436));
#33061=CARTESIAN_POINT('Ctrl Pts',(-0.22296962319346,0.00330683358017323,
-0.00971821280969721));
#33062=CARTESIAN_POINT('Ctrl Pts',(-0.222918488070061,0.00375942200152719,
-0.00994375002725347));
#33063=CARTESIAN_POINT('Ctrl Pts',(-0.222892083013316,0.00416376038165397,
-0.010111187965774));
#33064=CARTESIAN_POINT('Ctrl Pts',(-0.222880624396322,0.00442263472015358,
-0.0102052666341114));
#33065=CARTESIAN_POINT('',(-0.222990249020465,0.00750413602119545,-0.0107474065933957));
#33066=CARTESIAN_POINT('Ctrl Pts',(-0.222880624396322,0.00442263472015358,
-0.0102052666341114));
#33067=CARTESIAN_POINT('Ctrl Pts',(-0.222869165779329,0.0046815090586532,
-0.0102993453024488));
#33068=CARTESIAN_POINT('Ctrl Pts',(-0.222858538053683,0.00517788857248262,
-0.0104524093911042));
#33069=CARTESIAN_POINT('Ctrl Pts',(-0.222872218454889,0.005825756390809,
-0.0105939424252743));
#33070=CARTESIAN_POINT('Ctrl Pts',(-0.222894283711276,0.00623987313934977,
-0.0106579681688692));
#33071=CARTESIAN_POINT('Ctrl Pts',(-0.222910771496852,0.00650106062914115,
-0.0106909307204901));
#33072=CARTESIAN_POINT('Ctrl Pts',(-0.222927661448382,0.00673784986174582,
-0.0107142151130225));
#33073=CARTESIAN_POINT('Ctrl Pts',(-0.222937668479361,0.00686760687829407,
-0.0107242714777256));
#33074=CARTESIAN_POINT('Ctrl Pts',(-0.222957834975291,0.00712122554238282,
-0.010740444183054));
#33075=CARTESIAN_POINT('Ctrl Pts',(-0.222976136323122,0.00733939368582136,
-0.0107471639425212));
#33076=CARTESIAN_POINT('Ctrl Pts',(-0.222990249020465,0.00750413602119545,
-0.0107474065933957));
#33077=CARTESIAN_POINT('',(-0.222877378469082,0.0105855117421594,-0.0102022589418487));
#33078=CARTESIAN_POINT('Ctrl Pts',(-0.222990244138736,0.00750419266379995,
-0.0107474064566597));
#33079=CARTESIAN_POINT('Ctrl Pts',(-0.222976039113982,0.00766901363741887,
-0.0107470080875829));
#33080=CARTESIAN_POINT('Ctrl Pts',(-0.222957602873573,0.0078873936039232,
-0.0107400749543394));
#33081=CARTESIAN_POINT('Ctrl Pts',(-0.222937255048052,0.00814141129479029,
-0.0107236237028279));
#33082=CARTESIAN_POINT('Ctrl Pts',(-0.222927131990394,0.00827164133562222,
-0.0107133928644021));
#33083=CARTESIAN_POINT('Ctrl Pts',(-0.222910062603263,0.00850863202679079,
-0.0106898315254736));
#33084=CARTESIAN_POINT('Ctrl Pts',(-0.222893339477359,0.00877024695059987,
-0.0106565146658551));
#33085=CARTESIAN_POINT('Ctrl Pts',(-0.222870855927369,0.00918444368936968,
-0.0105920366667686));
#33086=CARTESIAN_POINT('Ctrl Pts',(-0.222856249020398,0.00983626402533809,
-0.0104486341552913));
#33087=CARTESIAN_POINT('Ctrl Pts',(-0.222866269191294,0.0103293456390423,
-0.0102956441034219));
#33088=CARTESIAN_POINT('Ctrl Pts',(-0.222877378469082,0.0105855117421594,
-0.0102022589418487));
#33089=CARTESIAN_POINT('',(-0.22331062247459,0.0132796121775377,-0.0086650768419741));
#33090=CARTESIAN_POINT('Ctrl Pts',(-0.222877378469082,0.0105855117421594,
-0.0102022589418487));
#33091=CARTESIAN_POINT('Ctrl Pts',(-0.222877439347042,0.010586915512061,
-0.0102017471985795));
#33092=CARTESIAN_POINT('Ctrl Pts',(-0.222888704245993,0.0108459462110236,
-0.0101072438214903));
#33093=CARTESIAN_POINT('Ctrl Pts',(-0.222914931562689,0.0112496955499137,
-0.0099395147505797));
#33094=CARTESIAN_POINT('Ctrl Pts',(-0.222966043253251,0.0117035833443654,
-0.00971273963873267));
#33095=CARTESIAN_POINT('Ctrl Pts',(-0.223011019189053,0.0120122134010204,
-0.00954390981295897));
#33096=CARTESIAN_POINT('Ctrl Pts',(-0.223060691065504,0.0122764008889023,
-0.00938554157135033));
#33097=CARTESIAN_POINT('Ctrl Pts',(-0.223106708820329,0.0124909981044285,
-0.0092481825342308));
#33098=CARTESIAN_POINT('Ctrl Pts',(-0.223151918814857,0.0126824022555419,
-0.00911841361702317));
#33099=CARTESIAN_POINT('Ctrl Pts',(-0.223175770367161,0.0127770012983113,
-0.00905151203694784));
#33100=CARTESIAN_POINT('Ctrl Pts',(-0.223227096344508,0.0129763708623679,
-0.00890683647480226));
#33101=CARTESIAN_POINT('Ctrl Pts',(-0.223274054708729,0.0131494382524228,
-0.00877258438081807));
#33102=CARTESIAN_POINT('Ctrl Pts',(-0.223310622067065,0.0132796145543947,
-0.00866508035255934));
#33103=CARTESIAN_POINT('',(-0.224514160940373,0.0132784691364097,-0.00868853601036365));
#33104=CARTESIAN_POINT('',(-0.224514160785051,0.0132784760514594,-0.00868854430898473));
#33105=CARTESIAN_POINT('',(-0.224077522253103,0.0105904549332816,-0.010226572185957));
#33106=CARTESIAN_POINT('Ctrl Pts',(-0.224514160940373,0.0132784691364097,
-0.00868853601036365));
#33107=CARTESIAN_POINT('Ctrl Pts',(-0.224477211330273,0.0131470369833515,
-0.00879735581073573));
#33108=CARTESIAN_POINT('Ctrl Pts',(-0.224429947924994,0.0129731504511415,
-0.00893246460129079));
#33109=CARTESIAN_POINT('Ctrl Pts',(-0.224378503318962,0.0127742662803209,
-0.00907701980843753));
#33110=CARTESIAN_POINT('Ctrl Pts',(-0.224355204002411,0.012682587246764,
-0.00914202253367616));
#33111=CARTESIAN_POINT('Ctrl Pts',(-0.224309198807288,0.012489784381346,
-0.00927305835532011));
#33112=CARTESIAN_POINT('Ctrl Pts',(-0.224262698143804,0.0122754037092251,
-0.0094105335025692));
#33113=CARTESIAN_POINT('Ctrl Pts',(-0.224212453791538,0.012012311248366,
-0.00956858000955867));
#33114=CARTESIAN_POINT('Ctrl Pts',(-0.224166966590675,0.0117051190396636,
-0.0097370321999535));
#33115=CARTESIAN_POINT('Ctrl Pts',(-0.224115284552749,0.0112520802508404,
-0.00996403935026655));
#33116=CARTESIAN_POINT('Ctrl Pts',(-0.224088864698508,0.010848572764703,
-0.010132103654354));
#33117=CARTESIAN_POINT('Ctrl Pts',(-0.224077522253103,0.0105904549332816,
-0.010226572185957));
#33118=CARTESIAN_POINT('',(-0.224190652839191,0.00750467962157126,-0.0107745363515886));
#33119=CARTESIAN_POINT('Ctrl Pts',(-0.224077522253103,0.0105904549332816,
-0.010226572185957));
#33120=CARTESIAN_POINT('Ctrl Pts',(-0.224066179807698,0.0103323371018601,
-0.0103210407175601));
#33121=CARTESIAN_POINT('Ctrl Pts',(-0.224056036498401,0.00983787575769098,
-0.010474829105189));
#33122=CARTESIAN_POINT('Ctrl Pts',(-0.224070822277838,0.00918506719538518,
-0.0106187627126106));
#33123=CARTESIAN_POINT('Ctrl Pts',(-0.224093495468947,0.00877092269132658,
-0.0106833806781232));
#33124=CARTESIAN_POINT('Ctrl Pts',(-0.224110305171158,0.00850937751485411,
-0.0107167762264158));
#33125=CARTESIAN_POINT('Ctrl Pts',(-0.224127483217192,0.0082719805659879,
-0.0107404318766813));
#33126=CARTESIAN_POINT('Ctrl Pts',(-0.224137553020629,0.00814288141660961,
-0.0107506002887076));
#33127=CARTESIAN_POINT('Ctrl Pts',(-0.224157926592086,0.00788901316584556,
-0.010767122229214));
#33128=CARTESIAN_POINT('Ctrl Pts',(-0.224176402851754,0.00767017484618538,
-0.0107741274603846));
#33129=CARTESIAN_POINT('Ctrl Pts',(-0.224190654114418,0.00750468128569608,
-0.0107745364705206));
#33130=CARTESIAN_POINT('',(-0.224080543674127,0.00442370045670947,-0.0102317785325732));
#33131=CARTESIAN_POINT('Ctrl Pts',(-0.224190653963733,0.00750467952515814,
-0.0107745364680395));
#33132=CARTESIAN_POINT('Ctrl Pts',(-0.224176492634204,0.00733922436874332,
-0.0107743032793675));
#33133=CARTESIAN_POINT('Ctrl Pts',(-0.224158150009196,0.0071205751719775,
-0.0107675345622608));
#33134=CARTESIAN_POINT('Ctrl Pts',(-0.224137959599138,0.00686713230331976,
-0.0107513204960082));
#33135=CARTESIAN_POINT('Ctrl Pts',(-0.22412801473866,0.00673863242070432,
-0.0107413514946879));
#33136=CARTESIAN_POINT('Ctrl Pts',(-0.224111008867221,0.00650134479792787,
-0.0107179940224818));
#33137=CARTESIAN_POINT('Ctrl Pts',(-0.224094430592809,0.0062402098664611,
-0.0106849790050444));
#33138=CARTESIAN_POINT('Ctrl Pts',(-0.224072172068249,0.00582632754687287,
-0.0106209007979213));
#33139=CARTESIAN_POINT('Ctrl Pts',(-0.224058310898166,0.00517837148533668,
-0.0104791024854185));
#33140=CARTESIAN_POINT('Ctrl Pts',(-0.224068978285216,0.00468250947702801,
-0.0103259955728961));
#33141=CARTESIAN_POINT('Ctrl Pts',(-0.224080543674127,0.00442370045670947,
-0.0102317785325732));
#33142=CARTESIAN_POINT('Ctrl Pts',(-0.224080576473508,0.00442296681989542,
-0.0102315114221622));
#33143=CARTESIAN_POINT('Ctrl Pts',(-0.224092164582625,0.00416389245189672,
-0.01013717187508));
#33144=CARTESIAN_POINT('Ctrl Pts',(-0.224118916883511,0.0037587335085994,
-0.00996905170028294));
#33145=CARTESIAN_POINT('Ctrl Pts',(-0.22417075519572,0.00330687307078908,
-0.00974336361782637));
#33146=CARTESIAN_POINT('Ctrl Pts',(-0.224215944808682,0.00300301955498354,
-0.00957745415886877));
#33147=CARTESIAN_POINT('Ctrl Pts',(-0.224266694586266,0.00273933256641242,
-0.0094197813232676));
#33148=CARTESIAN_POINT('Ctrl Pts',(-0.224313605043636,0.00252528923250781,
-0.00928311801791386));
#33149=CARTESIAN_POINT('Ctrl Pts',(-0.224360139565172,0.00233246415434654,
-0.00915264520743171));
#33150=CARTESIAN_POINT('Ctrl Pts',(-0.224383537818016,0.00224151895518211,
-0.00908844952425034));
#33151=CARTESIAN_POINT('Ctrl Pts',(-0.224435538741471,0.00204291078658062,
-0.00894477273158201));
#33152=CARTESIAN_POINT('Ctrl Pts',(-0.224483417379835,0.00186891392296787,
-0.00881022807967479));
#33153=CARTESIAN_POINT('Ctrl Pts',(-0.224520891120564,0.00173723890051058,
-0.00870172018785915));
#33154=CARTESIAN_POINT('',(-0.212297190745867,0.00261509365239396,-0.00909973957363974));
#33155=CARTESIAN_POINT('',(-0.211094978475873,0.0026144378598994,-0.00907540326291864));
#33156=CARTESIAN_POINT('',(-0.212297189692149,0.00261509491117278,-0.00909973513226721));
#33157=CARTESIAN_POINT('',(-0.210993897433281,0.00750003962408243,-0.0104762800771199));
#33158=CARTESIAN_POINT('Ctrl Pts',(-0.211094976956083,0.00261443904769588,
-0.00907540097906681));
#33159=CARTESIAN_POINT('Ctrl Pts',(-0.211076902605002,0.00273164864698635,
-0.00914838755433385));
#33160=CARTESIAN_POINT('Ctrl Pts',(-0.211053454528153,0.00288716843060544,
-0.00924010842643544));
#33161=CARTESIAN_POINT('Ctrl Pts',(-0.211027284102128,0.00306711239604655,
-0.00933999693310741));
#33162=CARTESIAN_POINT('Ctrl Pts',(-0.21101466974253,0.00315522153342331,
-0.00938771508920937));
#33163=CARTESIAN_POINT('Ctrl Pts',(-0.210991202323522,0.00332631582695644,
-0.00947684014530071));
#33164=CARTESIAN_POINT('Ctrl Pts',(-0.210966529056182,0.00351877420073698,
-0.00957165595315125));
#33165=CARTESIAN_POINT('Ctrl Pts',(-0.210940630339799,0.00373561938964548,
-0.00967286496974557));
#33166=CARTESIAN_POINT('Ctrl Pts',(-0.21090882306288,0.00405724803395585,
-0.00980902641083227));
#33167=CARTESIAN_POINT('Ctrl Pts',(-0.210880468868142,0.00443154685424827,
-0.00995193760637929));
#33168=CARTESIAN_POINT('Ctrl Pts',(-0.210860080553832,0.00496167972118646,
-0.0101244790534111));
#33169=CARTESIAN_POINT('Ctrl Pts',(-0.210862937430638,0.00545949645723989,
-0.0102482570737715));
#33170=CARTESIAN_POINT('Ctrl Pts',(-0.210876138533289,0.00588408926952714,
-0.0103325668728133));
#33171=CARTESIAN_POINT('Ctrl Pts',(-0.210893327512164,0.0062282183878831,
-0.010387245267968));
#33172=CARTESIAN_POINT('Ctrl Pts',(-0.210908799693423,0.00646418655898334,
-0.010416504326486));
#33173=CARTESIAN_POINT('Ctrl Pts',(-0.210924391642302,0.00667919920548634,
-0.0104384931741096));
#33174=CARTESIAN_POINT('Ctrl Pts',(-0.210939543408632,0.00687173172318124,
-0.0104538539003637));
#33175=CARTESIAN_POINT('Ctrl Pts',(-0.210948449678075,0.00697902885001758,
-0.0104606407092845));
#33176=CARTESIAN_POINT('Ctrl Pts',(-0.210966087921597,0.00718683343980474,
-0.010471448835588));
#33177=CARTESIAN_POINT('Ctrl Pts',(-0.210981837268104,0.00736539084021717,
-0.0104760080954136));
#33178=CARTESIAN_POINT('Ctrl Pts',(-0.210993897433281,0.00750003962408243,
-0.0104762800771199));
#33179=CARTESIAN_POINT('',(-0.211094250162357,0.0123877779842441,-0.00907399873728111));
#33180=CARTESIAN_POINT('Ctrl Pts',(-0.210993897632963,0.00750004185348807,
-0.0104762800816229));
#33181=CARTESIAN_POINT('Ctrl Pts',(-0.210981890216983,0.00763468789296296,
-0.0104760080851524));
#33182=CARTESIAN_POINT('Ctrl Pts',(-0.210966199980559,0.00781332793409896,
-0.0104714488088166));
#33183=CARTESIAN_POINT('Ctrl Pts',(-0.210948602845398,0.00802143287698861,
-0.0104606187649496));
#33184=CARTESIAN_POINT('Ctrl Pts',(-0.210939703774113,0.00812901655090803,
-0.0104538083326638));
#33185=CARTESIAN_POINT('Ctrl Pts',(-0.210924554722707,0.00832203008104696,
-0.0104383893943833));
#33186=CARTESIAN_POINT('Ctrl Pts',(-0.210908948238448,0.00853754616492999,
-0.0104163157338736));
#33187=CARTESIAN_POINT('Ctrl Pts',(-0.210893432115795,0.00877414459232575,
-0.0103869227932625));
#33188=CARTESIAN_POINT('Ctrl Pts',(-0.210876133572762,0.00911857566127197,
-0.0103320979866237));
#33189=CARTESIAN_POINT('Ctrl Pts',(-0.210862740048901,0.00954314440249559,
-0.0102476263108843));
#33190=CARTESIAN_POINT('Ctrl Pts',(-0.210859479042776,0.0100378417967945,
-0.0101245951266467));
#33191=CARTESIAN_POINT('Ctrl Pts',(-0.210879522352077,0.010570553837214,
-0.0099512065487221));
#33192=CARTESIAN_POINT('Ctrl Pts',(-0.210907788954054,0.0109453488756747,
-0.0098079652419107));
#33193=CARTESIAN_POINT('Ctrl Pts',(-0.210939669417399,0.011267837985318,
-0.00967129752156446));
#33194=CARTESIAN_POINT('Ctrl Pts',(-0.210965530369932,0.0114839680748931,
-0.00957031370016262));
#33195=CARTESIAN_POINT('Ctrl Pts',(-0.210990215655556,0.0116761440659366,
-0.0094755657339967));
#33196=CARTESIAN_POINT('Ctrl Pts',(-0.211013692363919,0.0118468850488585,
-0.00938656527404313));
#33197=CARTESIAN_POINT('Ctrl Pts',(-0.211026338937093,0.0119349808819548,
-0.00933882751891443));
#33198=CARTESIAN_POINT('Ctrl Pts',(-0.211052578045645,0.0121148872431664,
-0.00923890045957065));
#33199=CARTESIAN_POINT('Ctrl Pts',(-0.211076107929383,0.0122704862945661,
-0.00914708137410498));
#33200=CARTESIAN_POINT('Ctrl Pts',(-0.211094250162357,0.0123877779842441,
-0.00907399873728111));
#33201=CARTESIAN_POINT('',(-0.212296026124715,0.0123861564107362,-0.00909893835561097));
#33202=CARTESIAN_POINT('',(-0.21109425028115,0.0123877742504626,-0.00907399277386768));
#33203=CARTESIAN_POINT('',(-0.212194328822827,0.00750004200959953,-0.0105034107997523));
#33204=CARTESIAN_POINT('Ctrl Pts',(-0.212296025195952,0.012386155034837,
-0.00909893592235296));
#33205=CARTESIAN_POINT('Ctrl Pts',(-0.212277771181288,0.0122681537068886,
-0.00917262789174738));
#33206=CARTESIAN_POINT('Ctrl Pts',(-0.212262026617893,0.0121640536793492,
-0.00923406794799332));
#33207=CARTESIAN_POINT('Ctrl Pts',(-0.212248015826452,0.012069474226596,
-0.00928799208719917));
#33208=CARTESIAN_POINT('Ctrl Pts',(-0.212241010396515,0.0120221842692378,
-0.00931495428849542));
#33209=CARTESIAN_POINT('Ctrl Pts',(-0.212234439427194,0.0119772443834241,
-0.00933998720033867));
#33210=CARTESIAN_POINT('Ctrl Pts',(-0.212229075568991,0.0119402994511595,
-0.00936027144983805));
#33211=CARTESIAN_POINT('Ctrl Pts',(-0.212223711710787,0.0119033545188948,
-0.00938055569933742));
#33212=CARTESIAN_POINT('Ctrl Pts',(-0.212219552489172,0.0118744719849607,
-0.00939621227379056));
#33213=CARTESIAN_POINT('Ctrl Pts',(-0.212213511685548,0.0118314285085296,
-0.00941909943121386));
#33214=CARTESIAN_POINT('Ctrl Pts',(-0.212207470881924,0.0117883850320986,
-0.00944198658863716));
#33215=CARTESIAN_POINT('Ctrl Pts',(-0.212199552919732,0.0117310655767387,
-0.0094718896685894));
#33216=CARTESIAN_POINT('Ctrl Pts',(-0.212192484407939,0.0116783235343651,
-0.00949868046344015));
#33217=CARTESIAN_POINT('Ctrl Pts',(-0.212185415896147,0.0116255814919915,
-0.00952547125829089));
#33218=CARTESIAN_POINT('Ctrl Pts',(-0.212179193892156,0.0115774868294401,
-0.00954929070656413));
#33219=CARTESIAN_POINT('Ctrl Pts',(-0.212173309502402,0.0115310109034,-0.00957186554182796));
#33220=CARTESIAN_POINT('Ctrl Pts',(-0.212161540722894,0.0114380590513197,
-0.00961701521235564));
#33221=CARTESIAN_POINT('Ctrl Pts',(-0.212151120316311,0.0113516431713247,
-0.00965728933529618));
#33222=CARTESIAN_POINT('Ctrl Pts',(-0.212140516807543,0.0112547003042211,
-0.00970048125207246));
#33223=CARTESIAN_POINT('Ctrl Pts',(-0.212129913298776,0.0111577574371174,
-0.00974367316884873));
#33224=CARTESIAN_POINT('Ctrl Pts',(-0.212119135175636,0.0110501002630214,
-0.00978938029664853));
#33225=CARTESIAN_POINT('Ctrl Pts',(-0.212110169288513,0.0109496173505987,
-0.00982987977422684));
#33226=CARTESIAN_POINT('Ctrl Pts',(-0.212105030416407,0.0108920247411125,
-0.0098530923836181));
#33227=CARTESIAN_POINT('Ctrl Pts',(-0.212100484409045,0.0108368243355517,
-0.00987468061069946));
#33228=CARTESIAN_POINT('Ctrl Pts',(-0.212096381915708,0.0107818522688614,
-0.00989559572584027));
#33229=CARTESIAN_POINT('Ctrl Pts',(-0.212093326711515,0.0107409135335892,
-0.00991117160671009));
#33230=CARTESIAN_POINT('Ctrl Pts',(-0.212090517482946,0.0107000997302077,
-0.00992637045413619));
#33231=CARTESIAN_POINT('Ctrl Pts',(-0.212087892544318,0.010658492958655,
-0.00994152400292711));
#33232=CARTESIAN_POINT('Ctrl Pts',(-0.212075593191774,0.0104635412191762,
-0.0100125271253955));
#33233=CARTESIAN_POINT('Ctrl Pts',(-0.212067363419537,0.0102509499324125,
-0.0100818754945736));
#33234=CARTESIAN_POINT('Ctrl Pts',(-0.212063884862461,0.0100453926460674,
-0.0101409198863523));
#33235=CARTESIAN_POINT('Ctrl Pts',(-0.212060406305386,0.00983983535972219,
-0.0101999642781311));
#33236=CARTESIAN_POINT('Ctrl Pts',(-0.212061657359005,0.00964157027834746,
-0.0102496821449324));
#33237=CARTESIAN_POINT('Ctrl Pts',(-0.212066560809478,0.00943377986916841,
-0.0102944520101106));
#33238=CARTESIAN_POINT('Ctrl Pts',(-0.212069012534715,0.00932988466457889,
-0.0103168369426997));
#33239=CARTESIAN_POINT('Ctrl Pts',(-0.2120723790939,0.00922360061547029,
-0.0103379082944401));
#33240=CARTESIAN_POINT('Ctrl Pts',(-0.212076974896308,0.00911290057028226,
-0.0103577387941635));
#33241=CARTESIAN_POINT('Ctrl Pts',(-0.212081570698716,0.00900220052509422,
-0.010377569293887));
#33242=CARTESIAN_POINT('Ctrl Pts',(-0.212087400244757,0.00888704309246514,
-0.0103959570783915));
#33243=CARTESIAN_POINT('Ctrl Pts',(-0.212093439725352,0.00878228104010102,
-0.0104108722877212));
#33244=CARTESIAN_POINT('Ctrl Pts',(-0.212099479205947,0.00867751898773691,
-0.0104257874970509));
#33245=CARTESIAN_POINT('Ctrl Pts',(-0.212105719912849,0.00858320444963351,
-0.0104376177616694));
#33246=CARTESIAN_POINT('Ctrl Pts',(-0.212113035079603,0.00848009932947122,
-0.0104488749494349));
#33247=CARTESIAN_POINT('Ctrl Pts',(-0.21211669266298,0.00842854676939008,
-0.0104545035433176));
#33248=CARTESIAN_POINT('Ctrl Pts',(-0.212120619623256,0.00837479494961345,
-0.0104599551726937));
#33249=CARTESIAN_POINT('Ctrl Pts',(-0.212125126833372,0.00831578408466029,
-0.0104653377458155));
#33250=CARTESIAN_POINT('Ctrl Pts',(-0.212129634043488,0.00825677321970713,
-0.0104707203189373));
#33251=CARTESIAN_POINT('Ctrl Pts',(-0.212134724759161,0.00819248868025532,
-0.0104758892980401));
#33252=CARTESIAN_POINT('Ctrl Pts',(-0.21213874797157,0.00814265720978303,
-0.0104794924998593));
#33253=CARTESIAN_POINT('Ctrl Pts',(-0.212142771183979,0.00809282573931075,
-0.0104830957016785));
#33254=CARTESIAN_POINT('Ctrl Pts',(-0.212145721744291,0.00805746323684213,
-0.0104853613080341));
#33255=CARTESIAN_POINT('Ctrl Pts',(-0.212149407167978,0.00801383089916331,
-0.0104879038888235));
#33256=CARTESIAN_POINT('Ctrl Pts',(-0.212153092591665,0.00797019856148449,
-0.0104904464696128));
#33257=CARTESIAN_POINT('Ctrl Pts',(-0.212157515838839,0.00791828959182719,
-0.0104931349412913));
#33258=CARTESIAN_POINT('Ctrl Pts',(-0.212162223711799,0.00786378802432783,
-0.0104954173976478));
#33259=CARTESIAN_POINT('Ctrl Pts',(-0.212171639457718,0.00775478488932911,
-0.0104999823103607));
#33260=CARTESIAN_POINT('Ctrl Pts',(-0.212182188900109,0.00763541561494652,
-0.010503135815364));
#33261=CARTESIAN_POINT('Ctrl Pts',(-0.212194328841677,0.00750004244211601,
-0.0105034108204182));
#33262=CARTESIAN_POINT('Ctrl Pts',(-0.212194328802889,0.00750004201135476,
-0.0105034108195435));
#33263=CARTESIAN_POINT('Ctrl Pts',(-0.212182123539449,0.00736450040649182,
-0.0105031355974154));
#33264=CARTESIAN_POINT('Ctrl Pts',(-0.212171528626418,0.00724509368721271,
-0.0104999761795604));
#33265=CARTESIAN_POINT('Ctrl Pts',(-0.212162080336148,0.00713610960086918,
-0.0104954100708588));
#33266=CARTESIAN_POINT('Ctrl Pts',(-0.212157356186009,0.00708161749997084,
-0.0104931270140894));
#33267=CARTESIAN_POINT('Ctrl Pts',(-0.21215291990874,0.00702973214041256,
-0.010490438460955));
#33268=CARTESIAN_POINT('Ctrl Pts',(-0.212149231583743,0.00698621172109704,
-0.010487902327003));
#33269=CARTESIAN_POINT('Ctrl Pts',(-0.212145543258746,0.00694269130178152,
-0.010485366193051));
#33270=CARTESIAN_POINT('Ctrl Pts',(-0.212142599894812,0.0069075289581561,
-0.0104831149386858));
#33271=CARTESIAN_POINT('Ctrl Pts',(-0.212138566498245,0.00685768893969642,
-0.0104795127975055));
#33272=CARTESIAN_POINT('Ctrl Pts',(-0.212134533101678,0.00680784892123675,
-0.0104759106563253));
#33273=CARTESIAN_POINT('Ctrl Pts',(-0.212129414893486,0.00674334732119604,
-0.0104707262493208));
#33274=CARTESIAN_POINT('Ctrl Pts',(-0.212124891557789,0.00668420290603628,
-0.010465331278609));
#33275=CARTESIAN_POINT('Ctrl Pts',(-0.212120368222091,0.00662505849087652,
-0.0104599363078971));
#33276=CARTESIAN_POINT('Ctrl Pts',(-0.212116436438123,0.00657125637734932,
-0.0104544781964647));
#33277=CARTESIAN_POINT('Ctrl Pts',(-0.212112775599472,0.00651961866839045,
-0.0104488387645201));
#33278=CARTESIAN_POINT('Ctrl Pts',(-0.21210545392217,0.00641634325047269,
-0.0104375599006309));
#33279=CARTESIAN_POINT('Ctrl Pts',(-0.212099213203322,0.00632171996357587,
-0.010425680554823));
#33280=CARTESIAN_POINT('Ctrl Pts',(-0.212093220629257,0.00621716805955512,
-0.0104107896322911));
#33281=CARTESIAN_POINT('Ctrl Pts',(-0.212087228055191,0.00611261615553437,
-0.0103958987097591));
#33282=CARTESIAN_POINT('Ctrl Pts',(-0.212081491953092,0.00599818549761978,
-0.0103776255386813));
#33283=CARTESIAN_POINT('Ctrl Pts',(-0.212076978793602,0.00588796000678455,
-0.0103578922018477));
#33284=CARTESIAN_POINT('Ctrl Pts',(-0.212072465634112,0.00577773451594932,
-0.0103381588650141));
#33285=CARTESIAN_POINT('Ctrl Pts',(-0.212069171194045,0.00567167514409762,
-0.0103171548169983));
#33286=CARTESIAN_POINT('Ctrl Pts',(-0.212066792035586,0.00556794849651943,
-0.0102948284638349));
#33287=CARTESIAN_POINT('Ctrl Pts',(-0.212062033718667,0.00536049520136305,
-0.0102501757575081));
#33288=CARTESIAN_POINT('Ctrl Pts',(-0.212060929276825,0.00516233987027589,
-0.0102005541469401));
#33289=CARTESIAN_POINT('Ctrl Pts',(-0.212064583752465,0.00495647680610926,
-0.0101414727213551));
#33290=CARTESIAN_POINT('Ctrl Pts',(-0.212068238228106,0.00475061374194264,
-0.0100823912957701));
#33291=CARTESIAN_POINT('Ctrl Pts',(-0.212076673891627,0.00453730905366078,
-0.0100128424971044));
#33292=CARTESIAN_POINT('Ctrl Pts',(-0.212089098860114,0.00434224089645113,
-0.00994181834806706));
#33293=CARTESIAN_POINT('Ctrl Pts',(-0.212091765988984,0.00430036779920021,
-0.0099265723892066));
#33294=CARTESIAN_POINT('Ctrl Pts',(-0.212094615809571,0.00425932394153444,
-0.00991129019538823));
#33295=CARTESIAN_POINT('Ctrl Pts',(-0.212097714097661,0.00421814204450483,
-0.00989562226672202));
#33296=CARTESIAN_POINT('Ctrl Pts',(-0.21210183258344,0.00416339986030607,
-0.00987479523594094));
#33297=CARTESIAN_POINT('Ctrl Pts',(-0.212106390106241,0.00410841068640518,
-0.00985329330232126));
#33298=CARTESIAN_POINT('Ctrl Pts',(-0.212111541160687,0.00405096246581216,
-0.00983014395607332));
#33299=CARTESIAN_POINT('Ctrl Pts',(-0.212120567292405,0.00395029662904939,
-0.00978957963072948));
#33300=CARTESIAN_POINT('Ctrl Pts',(-0.212131423698469,0.00384219210363941,
-0.00974368374009559));
#33301=CARTESIAN_POINT('Ctrl Pts',(-0.212142046213562,0.00374522463100718,
-0.0097004800320845));
#33302=CARTESIAN_POINT('Ctrl Pts',(-0.212152668728655,0.00364825715837495,
-0.0096572763240734));
#33303=CARTESIAN_POINT('Ctrl Pts',(-0.212163048553079,0.00356223260132983,
-0.00961718215571804));
#33304=CARTESIAN_POINT('Ctrl Pts',(-0.21217478537429,0.00346950464697697,
-0.00957214819609432));
#33305=CARTESIAN_POINT('Ctrl Pts',(-0.212180653784895,0.00342314066980054,
-0.00954963121628245));
#33306=CARTESIAN_POINT('Ctrl Pts',(-0.212186862003761,0.00337511703119302,
-0.00952585173312588));
#33307=CARTESIAN_POINT('Ctrl Pts',(-0.212193910295831,0.00332246376500242,
-0.00949911215485694));
#33308=CARTESIAN_POINT('Ctrl Pts',(-0.2122009585879,0.00326981049881182,
-0.00947237257658799));
#33309=CARTESIAN_POINT('Ctrl Pts',(-0.212208849875716,0.0032125970416991,
-0.00944253293996776));
#33310=CARTESIAN_POINT('Ctrl Pts',(-0.21221487211149,0.00316961435383794,
-0.00941968492124474));
#33311=CARTESIAN_POINT('Ctrl Pts',(-0.212220894347265,0.00312663166597678,
-0.00939683690252173));
#33312=CARTESIAN_POINT('Ctrl Pts',(-0.212225043125917,0.00309776524461444,
-0.00938119425465462));
#33313=CARTESIAN_POINT('Ctrl Pts',(-0.212230393485056,0.00306084166967678,
-0.00936092826695534));
#33314=CARTESIAN_POINT('Ctrl Pts',(-0.212235743844195,0.00302391809473912,
-0.00934066227925607));
#33315=CARTESIAN_POINT('Ctrl Pts',(-0.212242298250575,0.00297900456721415,
-0.00931565235421951));
#33316=CARTESIAN_POINT('Ctrl Pts',(-0.212249286853305,0.00293173364208715,
-0.00928871011573586));
#33317=CARTESIAN_POINT('Ctrl Pts',(-0.212263264021031,0.00283719204706346,
-0.00923482578423803));
#33318=CARTESIAN_POINT('Ctrl Pts',(-0.212278973919057,0.00273310083018332,
-0.0091734129978045));
#33319=CARTESIAN_POINT('Ctrl Pts',(-0.212297189426323,0.00261509213602985,
-0.00909974167633009));
#33320=CARTESIAN_POINT('',(-0.20229073069173,0.00260802819594702,-0.00889711922744007));
#33321=CARTESIAN_POINT('',(-0.201088519916106,0.00260697650863716,-0.00887281289522955));
#33322=CARTESIAN_POINT('',(-0.202290729582105,0.00260802964547657,-0.0088971142446013));
#33323=CARTESIAN_POINT('',(-0.200997253167062,0.00750071976884877,-0.0102503476155925));
#33324=CARTESIAN_POINT('Ctrl Pts',(-0.201088517234415,0.00260697768703412,
-0.00887281028342328));
#33325=CARTESIAN_POINT('Ctrl Pts',(-0.201070231378405,0.00272574422538841,
-0.00894517065855103));
#33326=CARTESIAN_POINT('Ctrl Pts',(-0.20104660700157,0.00288268449617453,
-0.00903571755969753));
#33327=CARTESIAN_POINT('Ctrl Pts',(-0.201020428886199,0.00306324011348402,
-0.00913380586456596));
#33328=CARTESIAN_POINT('Ctrl Pts',(-0.201008031521991,0.00315009960764293,
-0.00917988033017122));
#33329=CARTESIAN_POINT('Ctrl Pts',(-0.200984567569492,0.00332254158062,
-0.00926785663333399));
#33330=CARTESIAN_POINT('Ctrl Pts',(-0.200960305513351,0.00351465179944262,
-0.00936066460635266));
#33331=CARTESIAN_POINT('Ctrl Pts',(-0.200923777451925,0.00382954798428417,
-0.00950417474699339));
#33332=CARTESIAN_POINT('Ctrl Pts',(-0.200882155475116,0.00433605979405848,
-0.00970630389687771));
#33333=CARTESIAN_POINT('Ctrl Pts',(-0.200862761315044,0.00496362486152777,
-0.00990440070219615));
#33334=CARTESIAN_POINT('Ctrl Pts',(-0.200867614140204,0.00544563190383476,
-0.0100236066604576));
#33335=CARTESIAN_POINT('Ctrl Pts',(-0.200881077294953,0.005828723981634,
-0.0100982028485135));
#33336=CARTESIAN_POINT('Ctrl Pts',(-0.200891145223225,0.00604404165042094,
-0.010134424351333));
#33337=CARTESIAN_POINT('Ctrl Pts',(-0.200901663721965,0.00623413010597689,
-0.0101623574414713));
#33338=CARTESIAN_POINT('Ctrl Pts',(-0.200907769791474,0.00633199116033011,
-0.0101751201838898));
#33339=CARTESIAN_POINT('Ctrl Pts',(-0.200919720793469,0.00651408529372874,
-0.010197196127569));
#33340=CARTESIAN_POINT('Ctrl Pts',(-0.200944415623066,0.00685633873757801,
-0.0102308035714179));
#33341=CARTESIAN_POINT('Ctrl Pts',(-0.200974002174022,0.00722536468550294,
-0.0102498434994338));
#33342=CARTESIAN_POINT('Ctrl Pts',(-0.200997253167062,0.00750071976884877,
-0.0102503476155925));
#33343=CARTESIAN_POINT('',(-0.201091338207746,0.0123976804872637,-0.00887001172820126));
#33344=CARTESIAN_POINT('Ctrl Pts',(-0.200997253189733,0.00750072003734376,
-0.0102503476160841));
#33345=CARTESIAN_POINT('Ctrl Pts',(-0.200974226058333,0.00777622966032588,
-0.0102498057883578));
#33346=CARTESIAN_POINT('Ctrl Pts',(-0.200944926608782,0.00814550668245003,
-0.0102306939411073));
#33347=CARTESIAN_POINT('Ctrl Pts',(-0.200920475693722,0.00848807026377426,
-0.0101969861106214));
#33348=CARTESIAN_POINT('Ctrl Pts',(-0.200908644715003,0.00867036462369381,
-0.0101748434138683));
#33349=CARTESIAN_POINT('Ctrl Pts',(-0.200902600687783,0.00876833805227905,
-0.010162042409973));
#33350=CARTESIAN_POINT('Ctrl Pts',(-0.200892191101917,0.00895870315128538,
-0.0101340170690275));
#33351=CARTESIAN_POINT('Ctrl Pts',(-0.200882239017754,0.00917425974551143,
-0.010097690760335));
#33352=CARTESIAN_POINT('Ctrl Pts',(-0.200868964749715,0.00955773818742233,
-0.0100228808043527));
#33353=CARTESIAN_POINT('Ctrl Pts',(-0.200864271521825,0.0100393106820076,
-0.00990363217018893));
#33354=CARTESIAN_POINT('Ctrl Pts',(-0.200883875554183,0.0106684281424501,
-0.00970474543934178));
#33355=CARTESIAN_POINT('Ctrl Pts',(-0.200925612659579,0.0111740766689703,
-0.00950266590494921));
#33356=CARTESIAN_POINT('Ctrl Pts',(-0.200962341330629,0.0114892663409321,
-0.00935886602107145));
#33357=CARTESIAN_POINT('Ctrl Pts',(-0.200986739504071,0.0116814829294643,
-0.00926589566588928));
#33358=CARTESIAN_POINT('Ctrl Pts',(-0.201010344072047,0.0118540654419843,
-0.00917774291603716));
#33359=CARTESIAN_POINT('Ctrl Pts',(-0.201022808712449,0.0119409346873194,
-0.00913160785205659));
#33360=CARTESIAN_POINT('Ctrl Pts',(-0.201049148976313,0.0121216430743756,
-0.00903331926895959));
#33361=CARTESIAN_POINT('Ctrl Pts',(-0.201072928578555,0.0122787618858155,
-0.00894255830868901));
#33362=CARTESIAN_POINT('Ctrl Pts',(-0.201091338207746,0.0123976804872637,
-0.00887001172820126));
#33363=CARTESIAN_POINT('',(-0.202293074116991,0.0123964300494642,-0.00889443311216738));
#33364=CARTESIAN_POINT('',(-0.201091338329048,0.0123976767118359,-0.00887000556980743));
#33365=CARTESIAN_POINT('',(-0.202197548254198,0.00750045600863564,-0.0102774753127245));
#33366=CARTESIAN_POINT('Ctrl Pts',(-0.202293072280915,0.0123964287538336,
-0.00889443052768938));
#33367=CARTESIAN_POINT('Ctrl Pts',(-0.202274494498572,0.0122768166966399,
-0.00896759163493234));
#33368=CARTESIAN_POINT('Ctrl Pts',(-0.202258537883566,0.012171743084332,
-0.00902831707970255));
#33369=CARTESIAN_POINT('Ctrl Pts',(-0.202244401605263,0.0120766332932925,
-0.00908143808158457));
#33370=CARTESIAN_POINT('Ctrl Pts',(-0.202237333434346,0.0120290781840582,
-0.00910799870189006));
#33371=CARTESIAN_POINT('Ctrl Pts',(-0.20223072137725,0.0119839839266795,
-0.00913260678336198));
#33372=CARTESIAN_POINT('Ctrl Pts',(-0.202225363198743,0.0119471877968328,
-0.00915240392969132));
#33373=CARTESIAN_POINT('Ctrl Pts',(-0.202220005020236,0.0119103916669861,
-0.00917220107602065));
#33374=CARTESIAN_POINT('Ctrl Pts',(-0.202215898250785,0.0118819602340639,
-0.0091873091097473));
#33375=CARTESIAN_POINT('Ctrl Pts',(-0.202209856163251,0.0118388980500071,
-0.00920975838000546));
#33376=CARTESIAN_POINT('Ctrl Pts',(-0.202203814075716,0.0117958358659502,
-0.00923220765026362));
#33377=CARTESIAN_POINT('Ctrl Pts',(-0.202195841123907,0.0117380282236051,
-0.00926178017206805));
#33378=CARTESIAN_POINT('Ctrl Pts',(-0.202188777096842,0.0116850814160394,
-0.00928815591228989));
#33379=CARTESIAN_POINT('Ctrl Pts',(-0.202181713069777,0.0116321346084737,
-0.00931453165251173));
#33380=CARTESIAN_POINT('Ctrl Pts',(-0.202175554902053,0.0115841212056271,
-0.00933785864569768));
#33381=CARTESIAN_POINT('Ctrl Pts',(-0.202169685062092,0.0115371577243816,
-0.00936023633717544));
#33382=CARTESIAN_POINT('Ctrl Pts',(-0.202157945382171,0.0114432307618907,
-0.00940499172013097));
#33383=CARTESIAN_POINT('Ctrl Pts',(-0.202147359312351,0.011353504796092,
-0.0094459379756937));
#33384=CARTESIAN_POINT('Ctrl Pts',(-0.202137462087568,0.011259896757467,
-0.00948687411303633));
#33385=CARTESIAN_POINT('Ctrl Pts',(-0.202120092033886,0.0110956106377205,
-0.00955871878856009));
#33386=CARTESIAN_POINT('Ctrl Pts',(-0.202104854053046,0.0109191718891678,
-0.00963009428879758));
#33387=CARTESIAN_POINT('Ctrl Pts',(-0.202093387924333,0.0107391546369728,
-0.00969630675200009));
#33388=CARTESIAN_POINT('Ctrl Pts',(-0.202091787558797,0.0107140290332449,
-0.00970554824464586));
#33389=CARTESIAN_POINT('Ctrl Pts',(-0.202090260671614,0.0106888351820918,
-0.00971469236466777));
#33390=CARTESIAN_POINT('Ctrl Pts',(-0.202088811721322,0.0106635979043288,
-0.00972372989803367));
#33391=CARTESIAN_POINT('Ctrl Pts',(-0.202076981486153,0.0104575432641258,
-0.00979751858885518));
#33392=CARTESIAN_POINT('Ctrl Pts',(-0.20207034465538,0.0102484667046851,
-0.00986398925107306));
#33393=CARTESIAN_POINT('Ctrl Pts',(-0.202067972793861,0.0100475507252513,
-0.00992073131987059));
#33394=CARTESIAN_POINT('Ctrl Pts',(-0.202065600932341,0.00984663474581746,
-0.00997747338866811));
#33395=CARTESIAN_POINT('Ctrl Pts',(-0.202067476359534,0.00965412391713009,
-0.0100252955433957));
#33396=CARTESIAN_POINT('Ctrl Pts',(-0.202073202188225,0.00944386085916814,
-0.0100700604354503));
#33397=CARTESIAN_POINT('Ctrl Pts',(-0.20207606510257,0.00933872933018716,
-0.0100924428814776));
#33398=CARTESIAN_POINT('Ctrl Pts',(-0.202079895387504,0.00922911533405485,
-0.0101138466780218));
#33399=CARTESIAN_POINT('Ctrl Pts',(-0.202084523624796,0.00912069371656406,
-0.010133028299003));
#33400=CARTESIAN_POINT('Ctrl Pts',(-0.202086837743442,0.00906648290781867,
-0.0101426191094935));
#33401=CARTESIAN_POINT('Ctrl Pts',(-0.202089350290228,0.00901257874257112,
-0.0101517018283888));
#33402=CARTESIAN_POINT('Ctrl Pts',(-0.202092361027929,0.00895383404463594,
-0.0101610201059614));
#33403=CARTESIAN_POINT('Ctrl Pts',(-0.20209537176563,0.00889508934670077,
-0.010170338383534));
#33404=CARTESIAN_POINT('Ctrl Pts',(-0.202098884187202,0.00883147883691273,
-0.0101797361479915));
#33405=CARTESIAN_POINT('Ctrl Pts',(-0.202101649554293,0.00878349099574898,
-0.0101864567721823));
#33406=CARTESIAN_POINT('Ctrl Pts',(-0.202104414921384,0.00873550315458523,
-0.0101931773963731));
#33407=CARTESIAN_POINT('Ctrl Pts',(-0.202106428339549,0.00870316764003492,
-0.0101974389521304));
#33408=CARTESIAN_POINT('Ctrl Pts',(-0.202108920491588,0.00866427834590321,
-0.0102023845624647));
#33409=CARTESIAN_POINT('Ctrl Pts',(-0.202111412643626,0.00862538905177151,
-0.0102073301727989));
#33410=CARTESIAN_POINT('Ctrl Pts',(-0.20211438615768,0.00857993192696311,
-0.0102128429215111));
#33411=CARTESIAN_POINT('Ctrl Pts',(-0.20211753897259,0.00853333627651013,
-0.0102181086866933));
#33412=CARTESIAN_POINT('Ctrl Pts',(-0.20212384460241,0.00844014497560417,
-0.0102286402170578));
#33413=CARTESIAN_POINT('Ctrl Pts',(-0.202130864181834,0.00834241335367361,
-0.0102383282389047));
#33414=CARTESIAN_POINT('Ctrl Pts',(-0.202138818565719,0.00823614458621563,
-0.0102469384026684));
#33415=CARTESIAN_POINT('Ctrl Pts',(-0.20215472733349,0.00802360705129966,
-0.0102641587301959));
#33416=CARTESIAN_POINT('Ctrl Pts',(-0.202174378256334,0.00777691961388399,
-0.0102769379987594));
#33417=CARTESIAN_POINT('Ctrl Pts',(-0.202197548276474,0.00750045623478144,
-0.010277475295121));
#33418=CARTESIAN_POINT('Ctrl Pts',(-0.202197548257345,0.00750045600840331,
-0.0102774752946998));
#33419=CARTESIAN_POINT('Ctrl Pts',(-0.202174203175516,0.00722418787536874,
-0.0102769612949105));
#33420=CARTESIAN_POINT('Ctrl Pts',(-0.202154402182172,0.00697769519644182,
-0.0102642204595934));
#33421=CARTESIAN_POINT('Ctrl Pts',(-0.202138370075718,0.0067653447285158,
-0.010247046325628));
#33422=CARTESIAN_POINT('Ctrl Pts',(-0.202130354020302,0.0066591694655523,
-0.0102384592562998));
#33423=CARTESIAN_POINT('Ctrl Pts',(-0.202123279456543,0.00656152943931938,
-0.0102287961037126));
#33424=CARTESIAN_POINT('Ctrl Pts',(-0.202116923777592,0.0064684343667805,
-0.0102182920830441));
#33425=CARTESIAN_POINT('Ctrl Pts',(-0.202113745938117,0.00642188683051106,
-0.0102130400727099));
#33426=CARTESIAN_POINT('Ctrl Pts',(-0.202110748631194,0.00637647896299386,
-0.0102075418327333));
#33427=CARTESIAN_POINT('Ctrl Pts',(-0.202108236329092,0.00633763121108928,
-0.010202609085463));
#33428=CARTESIAN_POINT('Ctrl Pts',(-0.202105724026989,0.0062987834591847,
-0.0101976763381926));
#33429=CARTESIAN_POINT('Ctrl Pts',(-0.202103694108944,0.00626648183425165,
-0.010193425669544));
#33430=CARTESIAN_POINT('Ctrl Pts',(-0.2021009060143,0.00621855639123403,
-0.010186723946201));
#33431=CARTESIAN_POINT('Ctrl Pts',(-0.202098117919657,0.00617063094821641,
-0.010180022222858));
#33432=CARTESIAN_POINT('Ctrl Pts',(-0.202094576527078,0.00610711120290014,
-0.0101706520808344));
#33433=CARTESIAN_POINT('Ctrl Pts',(-0.202091539695686,0.00604844186568722,
-0.0101613598309362));
#33434=CARTESIAN_POINT('Ctrl Pts',(-0.202088502864294,0.0059897725284743,
-0.0101520675810381));
#33435=CARTESIAN_POINT('Ctrl Pts',(-0.202085967113789,0.00593592844766217,
-0.0101430087253429));
#33436=CARTESIAN_POINT('Ctrl Pts',(-0.202083630277739,0.00588177702189636,
-0.0101334427620972));
#33437=CARTESIAN_POINT('Ctrl Pts',(-0.202078956605641,0.00577347417036475,
-0.0101143108356057));
#33438=CARTESIAN_POINT('Ctrl Pts',(-0.202075082802893,0.00566397593382631,
-0.0100929619309007));
#33439=CARTESIAN_POINT('Ctrl Pts',(-0.202072182143848,0.00555889914283848,
-0.0100706232669665));
#33440=CARTESIAN_POINT('Ctrl Pts',(-0.202066380825758,0.00534874556086281,
-0.0100259459390981));
#33441=CARTESIAN_POINT('Ctrl Pts',(-0.202064453366962,0.00515610306662607,
-0.00997815057565958));
#33442=CARTESIAN_POINT('Ctrl Pts',(-0.202066768684074,0.00495539428595943,
-0.00992153686344134));
#33443=CARTESIAN_POINT('Ctrl Pts',(-0.202069084001186,0.00475468550529279,
-0.0098649231512231));
#33444=CARTESIAN_POINT('Ctrl Pts',(-0.202075659074073,0.00454614650373027,
-0.00979871421367979));
#33445=CARTESIAN_POINT('Ctrl Pts',(-0.202087442152237,0.00434017468158449,
-0.00972505509448496));
#33446=CARTESIAN_POINT('Ctrl Pts',(-0.202088957696926,0.00431368249535475,
-0.00971558102622213));
#33447=CARTESIAN_POINT('Ctrl Pts',(-0.202090559446696,0.00428723079419437,
-0.00970598690689844));
#33448=CARTESIAN_POINT('Ctrl Pts',(-0.202092242088241,0.00426085025377553,
-0.00969628392349822));
#33449=CARTESIAN_POINT('Ctrl Pts',(-0.202103641671852,0.00408212699746957,
-0.00963054801507335));
#33450=CARTESIAN_POINT('Ctrl Pts',(-0.202118754034746,0.00390674732751332,
-0.00955964449039378));
#33451=CARTESIAN_POINT('Ctrl Pts',(-0.20213592699882,0.00374367671188409,
-0.00948841157134542));
#33452=CARTESIAN_POINT('Ctrl Pts',(-0.202145780893062,0.0036501063419974,
-0.00944753792554636));
#33453=CARTESIAN_POINT('Ctrl Pts',(-0.202156309756316,0.00356052315313633,
-0.00940670249336416));
#33454=CARTESIAN_POINT('Ctrl Pts',(-0.20216799037999,0.00346667879554435,
-0.00936203806939491));
#33455=CARTESIAN_POINT('Ctrl Pts',(-0.202173830691827,0.00341975661674836,
-0.00933970585741029));
#33456=CARTESIAN_POINT('Ctrl Pts',(-0.202179958877149,0.00337176970234555,
-0.00931641897443527));
#33457=CARTESIAN_POINT('Ctrl Pts',(-0.202186990410553,0.00331883357972307,
-0.00929007896089968));
#33458=CARTESIAN_POINT('Ctrl Pts',(-0.202194021943957,0.0032658974571006,
-0.00926373894736408));
#33459=CARTESIAN_POINT('Ctrl Pts',(-0.202201959897997,0.00320808475490152,
-0.00923419745669377));
#33460=CARTESIAN_POINT('Ctrl Pts',(-0.202207969334436,0.0031650605155377,
-0.00921179363609146));
#33461=CARTESIAN_POINT('Ctrl Pts',(-0.202213978770875,0.00312203627617388,
-0.00918938981548915));
#33462=CARTESIAN_POINT('Ctrl Pts',(-0.202218055227422,0.00309368573465424,
-0.00917434201417049));
#33463=CARTESIAN_POINT('Ctrl Pts',(-0.202223379993947,0.00305695144231377,
-0.00915460154150268));
#33464=CARTESIAN_POINT('Ctrl Pts',(-0.202228704760472,0.00302021714997329,
-0.00913486106883488));
#33465=CARTESIAN_POINT('Ctrl Pts',(-0.202235280308945,0.00297516564357389,
-0.0091103060139232));
#33466=CARTESIAN_POINT('Ctrl Pts',(-0.202242310233515,0.00292764956256295,
-0.00908379936175299));
#33467=CARTESIAN_POINT('Ctrl Pts',(-0.202256370042748,0.00283261767028968,
-0.00903078620789074));
#33468=CARTESIAN_POINT('Ctrl Pts',(-0.202272243236238,0.00272760700184593,
-0.00897017266924841));
#33469=CARTESIAN_POINT('Ctrl Pts',(-0.202290729295407,0.00260802662900566,
-0.00889712143907862));
#33470=CARTESIAN_POINT('',(-0.200288489608108,0.00260606627767471,-0.0088565175084996));
#33471=CARTESIAN_POINT('',(-0.199085603811712,0.00260467847622167,-0.00883205133599132));
#33472=CARTESIAN_POINT('',(-0.200288488520405,0.00260606784889207,-0.0088565123499802));
#33473=CARTESIAN_POINT('',(-0.198998268035306,0.00750170158931661,-0.0102051687696475));
#33474=CARTESIAN_POINT('Ctrl Pts',(-0.199085601119488,0.00260467972009568,
-0.00883204861089906));
#33475=CARTESIAN_POINT('Ctrl Pts',(-0.199067506452137,0.00272371785988628,
-0.00890426028999085));
#33476=CARTESIAN_POINT('Ctrl Pts',(-0.199044131665411,0.00288099175507442,
-0.00899460795740418));
#33477=CARTESIAN_POINT('Ctrl Pts',(-0.199018239202327,0.00306188063533018,
-0.00909245634302826));
#33478=CARTESIAN_POINT('Ctrl Pts',(-0.199005978008815,0.00314889853402773,
-0.00913841719159824));
#33479=CARTESIAN_POINT('Ctrl Pts',(-0.198982790163463,0.00332156603532327,
-0.00922613374755011));
#33480=CARTESIAN_POINT('Ctrl Pts',(-0.198958825555564,0.0035139176367545,
-0.00931866793364172));
#33481=CARTESIAN_POINT('Ctrl Pts',(-0.198922764022766,0.003829290069547,
-0.00946178592376709));
#33482=CARTESIAN_POINT('Ctrl Pts',(-0.198881879694765,0.00433562257220421,
-0.00966303763238278));
#33483=CARTESIAN_POINT('Ctrl Pts',(-0.198863131383457,0.00496409099012789,
-0.00986064921761845));
#33484=CARTESIAN_POINT('Ctrl Pts',(-0.198868335412294,0.00544577509415154,
-0.00997929788943944));
#33485=CARTESIAN_POINT('Ctrl Pts',(-0.198881970765267,0.00582907039941651,
-0.010053649419941));
#33486=CARTESIAN_POINT('Ctrl Pts',(-0.198892111562041,0.00604451891685977,
-0.0100897483235882));
#33487=CARTESIAN_POINT('Ctrl Pts',(-0.198902678405336,0.0062347615700293,
-0.0101175891596819));
#33488=CARTESIAN_POINT('Ctrl Pts',(-0.19890880151892,0.00633269713647193,
-0.0101303069565454));
#33489=CARTESIAN_POINT('Ctrl Pts',(-0.198920775760608,0.00651489848546796,
-0.0101522995605522));
#33490=CARTESIAN_POINT('Ctrl Pts',(-0.198945485503522,0.00685728554587353,
-0.0101857637123629));
#33491=CARTESIAN_POINT('Ctrl Pts',(-0.198975049131093,0.00722635221066761,
-0.010204694340746));
#33492=CARTESIAN_POINT('Ctrl Pts',(-0.198998268035306,0.00750170158931661,
-0.0102051687696475));
#33493=CARTESIAN_POINT('',(-0.199090547585037,0.0123998542045573,-0.00882937998736431));
#33494=CARTESIAN_POINT('Ctrl Pts',(-0.198998268042099,0.0075017016698774,
-0.0102051687697863));
#33495=CARTESIAN_POINT('Ctrl Pts',(-0.198975262697197,0.00777716699517044,
-0.0102045984688354));
#33496=CARTESIAN_POINT('Ctrl Pts',(-0.19894598350055,0.00814639028559267,
-0.0101855245739562));
#33497=CARTESIAN_POINT('Ctrl Pts',(-0.198921535655541,0.00848891979571509,
-0.0101519135771396));
#33498=CARTESIAN_POINT('Ctrl Pts',(-0.198909699198878,0.00867120867347047,
-0.0101298369351647));
#33499=CARTESIAN_POINT('Ctrl Pts',(-0.198903651182801,0.0087691668271986,
-0.010117076818613));
#33500=CARTESIAN_POINT('Ctrl Pts',(-0.198893222445148,0.0089595786910395,
-0.0100891311615914));
#33501=CARTESIAN_POINT('Ctrl Pts',(-0.198883240814823,0.00917515726562705,
-0.0100529157275236));
#33502=CARTESIAN_POINT('Ctrl Pts',(-0.198869893334788,0.00955867496945718,
-0.00997833705459149));
#33503=CARTESIAN_POINT('Ctrl Pts',(-0.198865044854715,0.0100400285423306,
-0.00985955619907535));
#33504=CARTESIAN_POINT('Ctrl Pts',(-0.198884354860069,0.0106695831171145,
-0.00966124188583534));
#33505=CARTESIAN_POINT('Ctrl Pts',(-0.198925753482806,0.0111752154117488,
-0.00945993219594404));
#33506=CARTESIAN_POINT('Ctrl Pts',(-0.198962259694651,0.011490639491165,
-0.00931660497153037));
#33507=CARTESIAN_POINT('Ctrl Pts',(-0.198986515375409,0.0116829856636076,
-0.00922395071753861));
#33508=CARTESIAN_POINT('Ctrl Pts',(-0.199009988182743,0.011855702949848,
-0.0091360949988362));
#33509=CARTESIAN_POINT('Ctrl Pts',(-0.199022383731062,0.0119426366934164,
-0.00909011953258369));
#33510=CARTESIAN_POINT('Ctrl Pts',(-0.199048581320397,0.0121235063356898,
-0.00899215974570331));
#33511=CARTESIAN_POINT('Ctrl Pts',(-0.19907223476441,0.0122807914137443,
-0.00890169526387644));
#33512=CARTESIAN_POINT('Ctrl Pts',(-0.199090547585037,0.0123998542045573,
-0.00882937998736431));
#33513=CARTESIAN_POINT('',(-0.200292338257129,0.0123986218814099,-0.00885373242023577));
#33514=CARTESIAN_POINT('',(-0.1990905477074,0.0123998504040343,-0.00882937376053058));
#33515=CARTESIAN_POINT('',(-0.200198408071207,0.00750103329744417,-0.0102322930460279));
#33516=CARTESIAN_POINT('Ctrl Pts',(-0.200292336411079,0.0123986205739213,
-0.00885372980557329));
#33517=CARTESIAN_POINT('Ctrl Pts',(-0.200273857423805,0.0122788598610061,
-0.00892666423347511));
#33518=CARTESIAN_POINT('Ctrl Pts',(-0.200257986138083,0.0121736699411429,
-0.00898719795378537));
#33519=CARTESIAN_POINT('Ctrl Pts',(-0.2002439262477,0.0120784622944802,
-0.00904014962650077));
#33520=CARTESIAN_POINT('Ctrl Pts',(-0.20023689627133,0.0120308582600157,
-0.00906662558028448));
#33521=CARTESIAN_POINT('Ctrl Pts',(-0.200230320168875,0.0119857198874726,
-0.00909115471047935));
#33522=CARTESIAN_POINT('Ctrl Pts',(-0.200224991193952,0.0119488887897826,
-0.0091108881514725));
#33523=CARTESIAN_POINT('Ctrl Pts',(-0.200219662219028,0.0119120576920926,
-0.00913062159246565));
#33524=CARTESIAN_POINT('Ctrl Pts',(-0.20021557791321,0.0118835999835593,
-0.00914568084411158));
#33525=CARTESIAN_POINT('Ctrl Pts',(-0.200209569574122,0.0118404999931127,
-0.00916805714683687));
#33526=CARTESIAN_POINT('Ctrl Pts',(-0.200203561235034,0.0117974000026662,
-0.00919043344956217));
#33527=CARTESIAN_POINT('Ctrl Pts',(-0.200195633296685,0.0117395438100094,
-0.00921990941307956));
#33528=CARTESIAN_POINT('Ctrl Pts',(-0.200188609958376,0.0116865548788483,
-0.00924619873884898));
#33529=CARTESIAN_POINT('Ctrl Pts',(-0.200181586620067,0.0116335659476873,
-0.0092724880646184));
#33530=CARTESIAN_POINT('Ctrl Pts',(-0.200175464829421,0.0115855163576409,
-0.00929573837995581));
#33531=CARTESIAN_POINT('Ctrl Pts',(-0.200169630008592,0.0115385156030165,
-0.00931804389564718));
#33532=CARTESIAN_POINT('Ctrl Pts',(-0.200157960366936,0.0114445140937676,
-0.00936265492702992));
#33533=CARTESIAN_POINT('Ctrl Pts',(-0.200147438913252,0.0113547089314509,
-0.00940347437178023));
#33534=CARTESIAN_POINT('Ctrl Pts',(-0.200137609106914,0.0112610547873119,
-0.00944427013630663));
#33535=CARTESIAN_POINT('Ctrl Pts',(-0.200120051269694,0.0110937713067034,
-0.00951713885500349));
#33536=CARTESIAN_POINT('Ctrl Pts',(-0.200104710590186,0.0109140070200952,
-0.0095894788353709));
#33537=CARTESIAN_POINT('Ctrl Pts',(-0.200093291444196,0.0107306172547326,
-0.0096564589648824));
#33538=CARTESIAN_POINT('Ctrl Pts',(-0.200091924505863,0.0107086644308998,
-0.00966447687679018));
#33539=CARTESIAN_POINT('Ctrl Pts',(-0.200090613761087,0.010686660781902,
-0.00967242046945206));
#33540=CARTESIAN_POINT('Ctrl Pts',(-0.200089362133423,0.0106646224704097,
-0.00968028375905126));
#33541=CARTESIAN_POINT('Ctrl Pts',(-0.200077654643436,0.010458480245711,
-0.00975383549244965));
#33542=CARTESIAN_POINT('Ctrl Pts',(-0.200071117844305,0.010249176179895,
-0.00982014029840789));
#33543=CARTESIAN_POINT('Ctrl Pts',(-0.200068825516657,0.0100482127987205,
-0.00987669426350142));
#33544=CARTESIAN_POINT('Ctrl Pts',(-0.20006653318901,0.00984724941754597,
-0.00993324822859494));
#33545=CARTESIAN_POINT('Ctrl Pts',(-0.200068467409846,0.00965487328195331,
-0.00998087145327418));
#33546=CARTESIAN_POINT('Ctrl Pts',(-0.200074230964292,0.00944461437737611,
-0.0100254863843596));
#33547=CARTESIAN_POINT('Ctrl Pts',(-0.200077112741515,0.00933948492508751,
-0.0100477938499023));
#33548=CARTESIAN_POINT('Ctrl Pts',(-0.200080956650382,0.00922984032252973,
-0.0100691336047581));
#33549=CARTESIAN_POINT('Ctrl Pts',(-0.200085593257487,0.00912138630961319,
-0.0100882582187389));
#33550=CARTESIAN_POINT('Ctrl Pts',(-0.20008791156104,0.00906715930315493,
-0.0100978205257293));
#33551=CARTESIAN_POINT('Ctrl Pts',(-0.200090426979645,0.00901323845330599,
-0.0101068764881864));
#33552=CARTESIAN_POINT('Ctrl Pts',(-0.200093439296429,0.00895446814128281,
-0.0101161684714052));
#33553=CARTESIAN_POINT('Ctrl Pts',(-0.200096451613213,0.00889569782925962,
-0.0101254604546241));
#33554=CARTESIAN_POINT('Ctrl Pts',(-0.20009996431432,0.00883205290627755,
-0.0101348326651809));
#33555=CARTESIAN_POINT('Ctrl Pts',(-0.200102728596934,0.00878404736045819,
-0.0101415338671528));
#33556=CARTESIAN_POINT('Ctrl Pts',(-0.200105492879549,0.00873604181463882,
-0.0101482350691247));
#33557=CARTESIAN_POINT('Ctrl Pts',(-0.200107503860301,0.00870370514200726,
-0.0101524828667423));
#33558=CARTESIAN_POINT('Ctrl Pts',(-0.200109992697036,0.00866481179141373,
-0.0101574129882443));
#33559=CARTESIAN_POINT('Ctrl Pts',(-0.200112481533771,0.0086259184408202,
-0.0101623431097463));
#33560=CARTESIAN_POINT('Ctrl Pts',(-0.200115450847707,0.008580454442893,
-0.0101678389360936));
#33561=CARTESIAN_POINT('Ctrl Pts',(-0.200118598464806,0.00853385386382148,
-0.010173088425976));
#33562=CARTESIAN_POINT('Ctrl Pts',(-0.200124893699004,0.00844065270567845,
-0.0101835874057408));
#33563=CARTESIAN_POINT('Ctrl Pts',(-0.200131898901286,0.0083429189224858,
-0.010193245062841));
#33564=CARTESIAN_POINT('Ctrl Pts',(-0.20013983500335,0.00823665261474254,
-0.0102018289916747));
#33565=CARTESIAN_POINT('Ctrl Pts',(-0.200155707207479,0.00802411999925601,
-0.0102189968493419));
#33566=CARTESIAN_POINT('Ctrl Pts',(-0.200175305948972,0.00777745593880945,
-0.0102317401265822));
#33567=CARTESIAN_POINT('Ctrl Pts',(-0.200198408092455,0.00750103375755189,
-0.0102322930261764));
#33568=CARTESIAN_POINT('Ctrl Pts',(-0.200198408053672,0.00750103329896434,
-0.0102322930253509));
#33569=CARTESIAN_POINT('Ctrl Pts',(-0.2001750414276,0.00722473781003592,
-0.0102317956646293));
#33570=CARTESIAN_POINT('Ctrl Pts',(-0.200155217020202,0.00697821917512664,
-0.0102191136148449));
#33571=CARTESIAN_POINT('Ctrl Pts',(-0.200139160143905,0.00676583736411692,
-0.0102020103849557));
#33572=CARTESIAN_POINT('Ctrl Pts',(-0.200131131701314,0.00665964639986116,
-0.0101934587652799));
#33573=CARTESIAN_POINT('Ctrl Pts',(-0.200124044414963,0.00656198933436801,
-0.0101838339575191));
#33574=CARTESIAN_POINT('Ctrl Pts',(-0.200117675154785,0.00646887989036955,
-0.0101733710542036));
#33575=CARTESIAN_POINT('Ctrl Pts',(-0.200114490524696,0.00642232516837032,
-0.0101681396025458));
#33576=CARTESIAN_POINT('Ctrl Pts',(-0.200111486208921,0.00637691075266694,
-0.0101626627715528));
#33577=CARTESIAN_POINT('Ctrl Pts',(-0.200108967406514,0.00633805215836633,
-0.0101577484283255));
#33578=CARTESIAN_POINT('Ctrl Pts',(-0.200106448604107,0.00629919356406571,
-0.0101528340850982));
#33579=CARTESIAN_POINT('Ctrl Pts',(-0.200104412705854,0.00626687691983241,
-0.0101485983115396));
#33580=CARTESIAN_POINT('Ctrl Pts',(-0.200101616155769,0.00621895242659197,
-0.0101419232912671));
#33581=CARTESIAN_POINT('Ctrl Pts',(-0.200098819605684,0.00617102793335153,
-0.0101352482709947));
#33582=CARTESIAN_POINT('Ctrl Pts',(-0.200095267259168,0.00610752485173003,
-0.0101259176528732));
#33583=CARTESIAN_POINT('Ctrl Pts',(-0.200092218919278,0.00604886456963942,
-0.0101166636401912));
#33584=CARTESIAN_POINT('Ctrl Pts',(-0.200089170579389,0.0059902042875488,
-0.0101074096275093));
#33585=CARTESIAN_POINT('Ctrl Pts',(-0.200086622783407,0.00593636187616354,
-0.0100983869607788));
#33586=CARTESIAN_POINT('Ctrl Pts',(-0.200084272753936,0.00588221105991508,
-0.0100888589275013));
#33587=CARTESIAN_POINT('Ctrl Pts',(-0.200079572694994,0.00577390942741817,
-0.0100698028609464));
#33588=CARTESIAN_POINT('Ctrl Pts',(-0.20007566789051,0.00566440786363879,
-0.0100485377791556));
#33589=CARTESIAN_POINT('Ctrl Pts',(-0.200072733636695,0.00555930929747007,
-0.0100262824238011));
#33590=CARTESIAN_POINT('Ctrl Pts',(-0.200066865129066,0.00534911216513262,
-0.00998177171309202));
#33591=CARTESIAN_POINT('Ctrl Pts',(-0.200064860248902,0.00515635425120098,
-0.0099341348136642));
#33592=CARTESIAN_POINT('Ctrl Pts',(-0.200067068255993,0.00495556995531808,
-0.00987772033772398));
#33593=CARTESIAN_POINT('Ctrl Pts',(-0.200069276263084,0.00475478565943518,
-0.00982130586178375));
#33594=CARTESIAN_POINT('Ctrl Pts',(-0.200075713987207,0.004546208178983,
-0.00975534338054551));
#33595=CARTESIAN_POINT('Ctrl Pts',(-0.200087321533276,0.00434016439324928,
-0.00968195214074013));
#33596=CARTESIAN_POINT('Ctrl Pts',(-0.2000886527572,0.00431653403973075,
-0.00967353518734554));
#33597=CARTESIAN_POINT('Ctrl Pts',(-0.200090052016831,0.00429293545299616,
-0.00966502305895532));
#33598=CARTESIAN_POINT('Ctrl Pts',(-0.200091515596528,0.00426939032521055,
-0.00965642358470294));
#33599=CARTESIAN_POINT('Ctrl Pts',(-0.200102813632993,0.00408763478913916,
-0.009590040336886));
#33600=CARTESIAN_POINT('Ctrl Pts',(-0.200117944500455,0.00390914660919813,
-0.00951826971542129));
#33601=CARTESIAN_POINT('Ctrl Pts',(-0.200135198996426,0.00374331233281143,
-0.00944613006251162));
#33602=CARTESIAN_POINT('Ctrl Pts',(-0.200144943842591,0.00364965387329946,
-0.00940538764840724));
#33603=CARTESIAN_POINT('Ctrl Pts',(-0.200155362599063,0.00355996581759564,
-0.00936467522534425));
#33604=CARTESIAN_POINT('Ctrl Pts',(-0.200166923307577,0.00346601444258958,
-0.00932014774930243));
#33605=CARTESIAN_POINT('Ctrl Pts',(-0.200172703661834,0.00341903875508654,
-0.00929788401128153));
#33606=CARTESIAN_POINT('Ctrl Pts',(-0.200178769436932,0.0033709977718656,
-0.00927466910998229));
#33607=CARTESIAN_POINT('Ctrl Pts',(-0.200185729564161,0.00331800612595654,
-0.00924841316153132));
#33608=CARTESIAN_POINT('Ctrl Pts',(-0.200192689691389,0.00326501448004748,
-0.00922215721308034));
#33609=CARTESIAN_POINT('Ctrl Pts',(-0.20020054722797,0.00320714423423817,
-0.00919271239613813));
#33610=CARTESIAN_POINT('Ctrl Pts',(-0.200206498554751,0.0031640587926023,
-0.00917037262902342));
#33611=CARTESIAN_POINT('Ctrl Pts',(-0.200212449881531,0.00312097335096644,
-0.00914803286190872));
#33612=CARTESIAN_POINT('Ctrl Pts',(-0.200216490557461,0.00309255879840688,
-0.00913301582033758));
#33613=CARTESIAN_POINT('Ctrl Pts',(-0.200221766654028,0.00305575582272453,
-0.00911332320001298));
#33614=CARTESIAN_POINT('Ctrl Pts',(-0.200227042750594,0.00301895284704218,
-0.00909363057968837));
#33615=CARTESIAN_POINT('Ctrl Pts',(-0.200233556728865,0.00297382752400723,
-0.00906914078631249));
#33616=CARTESIAN_POINT('Ctrl Pts',(-0.200240520992314,0.0029262323204959,
-0.00904270432387586));
#33617=CARTESIAN_POINT('Ctrl Pts',(-0.200254449480275,0.00283104217957486,
-0.00898983154680711));
#33618=CARTESIAN_POINT('Ctrl Pts',(-0.200270175007452,0.00272585285310391,
-0.00892937760645072));
#33619=CARTESIAN_POINT('Ctrl Pts',(-0.20028848823233,0.00260606466462287,
-0.00885651981476795));
#33620=CARTESIAN_POINT('',(-0.198286049999512,0.00260395535089921,-0.00881591880117876));
#33621=CARTESIAN_POINT('',(-0.197087022945346,0.00260284474309971,-0.00879175610761492));
#33622=CARTESIAN_POINT('',(-0.198286048907163,0.00260395688255514,-0.00881591368481554));
#33623=CARTESIAN_POINT('',(-0.196999277771019,0.00750268308291533,-0.0101599897056429));
#33624=CARTESIAN_POINT('Ctrl Pts',(-0.19708702016317,0.00260284594471271,
-0.00879175341490894));
#33625=CARTESIAN_POINT('Ctrl Pts',(-0.197068834773877,0.00272208793814125,
-0.00886375452525914));
#33626=CARTESIAN_POINT('Ctrl Pts',(-0.197045347018576,0.00287958672224235,
-0.00895381700776416));
#33627=CARTESIAN_POINT('Ctrl Pts',(-0.197019337786194,0.0030606704278004,
-0.00905132901012702));
#33628=CARTESIAN_POINT('Ctrl Pts',(-0.197007030683302,0.00314771264160573,
-0.00909709763797359));
#33629=CARTESIAN_POINT('Ctrl Pts',(-0.196983739637954,0.00332057904228507,
-0.00918452681865033));
#33630=CARTESIAN_POINT('Ctrl Pts',(-0.196959681604442,0.00351309773812326,
-0.00927673815620894));
#33631=CARTESIAN_POINT('Ctrl Pts',(-0.196923484098549,0.00382889007914085,
-0.0094194146781178));
#33632=CARTESIAN_POINT('Ctrl Pts',(-0.196882627187949,0.00433458182040128,
-0.00961962280043831));
#33633=CARTESIAN_POINT('Ctrl Pts',(-0.196864021895861,0.00496479377443585,
-0.00981699691993611));
#33634=CARTESIAN_POINT('Ctrl Pts',(-0.196869394342641,0.00544543475974735,
-0.00993489940569601));
#33635=CARTESIAN_POINT('Ctrl Pts',(-0.196883099379931,0.00582913403511029,
-0.0100090605613923));
#33636=CARTESIAN_POINT('Ctrl Pts',(-0.196893270946229,0.00604484605787118,
-0.0100450608561695));
#33637=CARTESIAN_POINT('Ctrl Pts',(-0.196903863329604,0.00623549696952723,
-0.0100728439930441));
#33638=CARTESIAN_POINT('Ctrl Pts',(-0.196909981015821,0.00633340968562837,
-0.0100855011664594));
#33639=CARTESIAN_POINT('Ctrl Pts',(-0.196921948697463,0.0065157190270304,
-0.0101074090344271));
#33640=CARTESIAN_POINT('Ctrl Pts',(-0.196946621808918,0.00685819946467974,
-0.0101407227075091));
#33641=CARTESIAN_POINT('Ctrl Pts',(-0.196976119313645,0.00722732122593311,
-0.0101595453695121));
#33642=CARTESIAN_POINT('Ctrl Pts',(-0.196999277771019,0.00750268308291533,
-0.0101599897056429));
#33643=CARTESIAN_POINT('',(-0.19708967999411,0.0124019686593504,-0.00878888197156201));
#33644=CARTESIAN_POINT('Ctrl Pts',(-0.196999277761509,0.00750268319688206,
-0.0101599897053952));
#33645=CARTESIAN_POINT('Ctrl Pts',(-0.19697629483056,0.00777809536223536,
-0.010159391190194));
#33646=CARTESIAN_POINT('Ctrl Pts',(-0.196947035992263,0.00814725538564192,
-0.0101403577789055));
#33647=CARTESIAN_POINT('Ctrl Pts',(-0.196922590041325,0.00848974553611497,
-0.0101068472176815));
#33648=CARTESIAN_POINT('Ctrl Pts',(-0.196910746879266,0.00867202861783065,
-0.0100848385512457));
#33649=CARTESIAN_POINT('Ctrl Pts',(-0.196904694182073,0.00876996963382525,
-0.0100721206783229));
#33650=CARTESIAN_POINT('Ctrl Pts',(-0.196894243760702,0.00896043688002101,
-0.0100442557114248));
#33651=CARTESIAN_POINT('Ctrl Pts',(-0.196884229454297,0.00917604072854748,
-0.0100081532861656));
#33652=CARTESIAN_POINT('Ctrl Pts',(-0.196870802252705,0.00955960072650904,
-0.00993381012963068));
#33653=CARTESIAN_POINT('Ctrl Pts',(-0.196865786671437,0.0100406836425149,
-0.00981551941099423));
#33654=CARTESIAN_POINT('Ctrl Pts',(-0.196884786269139,0.0106707171059872,
-0.00961778134897869));
#33655=CARTESIAN_POINT('Ctrl Pts',(-0.196925832894908,0.0111762928595007,
-0.00941727326247245));
#33656=CARTESIAN_POINT('Ctrl Pts',(-0.196962111865516,0.0114919544302138,
-0.00927443101340539));
#33657=CARTESIAN_POINT('Ctrl Pts',(-0.196986222319099,0.0116844289439496,
-0.00918210195977756));
#33658=CARTESIAN_POINT('Ctrl Pts',(-0.197009561269637,0.0118572808422539,
-0.00909455157396046));
#33659=CARTESIAN_POINT('Ctrl Pts',(-0.197021886668872,0.0119442782511614,
-0.00904874043222638));
#33660=CARTESIAN_POINT('Ctrl Pts',(-0.197047939559998,0.0121253088794259,
-0.0089511188934817));
#33661=CARTESIAN_POINT('Ctrl Pts',(-0.197071465199352,0.0122827607284905,
-0.00886095937504394));
#33662=CARTESIAN_POINT('Ctrl Pts',(-0.19708967999411,0.0124019686593504,
-0.00878888197156201));
#33663=CARTESIAN_POINT('',(-0.198291539773098,0.0124007197494604,-0.00881318649061618));
#33664=CARTESIAN_POINT('',(-0.197089680117917,0.0124019648222841,-0.00878887565627935));
#33665=CARTESIAN_POINT('',(-0.198199421594319,0.00750212679056316,-0.0101871141141493));
#33666=CARTESIAN_POINT('Ctrl Pts',(-0.19829153792328,0.0124007184247131,
-0.00881318383781034));
#33667=CARTESIAN_POINT('Ctrl Pts',(-0.198273154963815,0.0122808214712712,
-0.00888587603724278));
#33668=CARTESIAN_POINT('Ctrl Pts',(-0.198257366571701,0.0121755265252124,
-0.008946205391425));
#33669=CARTESIAN_POINT('Ctrl Pts',(-0.19824338083647,0.0120802313201533,
-0.00899897686821169));
#33670=CARTESIAN_POINT('Ctrl Pts',(-0.198236387938163,0.0120325835084961,
-0.00902536272241327));
#33671=CARTESIAN_POINT('Ctrl Pts',(-0.19822984672429,0.0119874059341052,
-0.0090498079275906));
#33672=CARTESIAN_POINT('Ctrl Pts',(-0.198224546066974,0.0119505437898245,
-0.00906947374403427));
#33673=CARTESIAN_POINT('Ctrl Pts',(-0.198219245409658,0.0119136816455438,
-0.00908913956047794));
#33674=CARTESIAN_POINT('Ctrl Pts',(-0.198215182862346,0.0118852005663994,
-0.0091041471282794));
#33675=CARTESIAN_POINT('Ctrl Pts',(-0.198209207227433,0.0118420675052475,
-0.00912644603588376));
#33676=CARTESIAN_POINT('Ctrl Pts',(-0.198203231592519,0.0117989344440956,
-0.00914874494348811));
#33677=CARTESIAN_POINT('Ctrl Pts',(-0.198195347282797,0.0117410363097808,
-0.00917811846332321));
#33678=CARTESIAN_POINT('Ctrl Pts',(-0.198188363332505,0.0116880111449667,
-0.00920431629631211));
#33679=CARTESIAN_POINT('Ctrl Pts',(-0.198181379382213,0.0116349859801525,
-0.00923051412930102));
#33680=CARTESIAN_POINT('Ctrl Pts',(-0.198175292753102,0.0115869053439776,
-0.00925368344306097));
#33681=CARTESIAN_POINT('Ctrl Pts',(-0.198169491817117,0.0115398731891329,
-0.00927591228520045));
#33682=CARTESIAN_POINT('Ctrl Pts',(-0.198157889945145,0.0114458088794436,
-0.0093203699694794));
#33683=CARTESIAN_POINT('Ctrl Pts',(-0.19814743116075,0.0113559392858479,
-0.00936105307203295));
#33684=CARTESIAN_POINT('Ctrl Pts',(-0.198137665924961,0.0112622449179336,
-0.00940170329857409));
#33685=CARTESIAN_POINT('Ctrl Pts',(-0.198119918429903,0.0110919632813885,
-0.00947558166773796));
#33686=CARTESIAN_POINT('Ctrl Pts',(-0.198104472435404,0.0109088411223429,
-0.00954888130057903));
#33687=CARTESIAN_POINT('Ctrl Pts',(-0.198093103285736,0.0107220794811649,
-0.00961660935126367));
#33688=CARTESIAN_POINT('Ctrl Pts',(-0.198091961100495,0.0107033167419592,
-0.00962341355229707));
#33689=CARTESIAN_POINT('Ctrl Pts',(-0.19809086006255,0.0106845181021202,
-0.00963016337228091));
#33690=CARTESIAN_POINT('Ctrl Pts',(-0.198089801972049,0.0106656934819478,
-0.00963685515692382));
#33691=CARTESIAN_POINT('Ctrl Pts',(-0.198078211798985,0.0104594912662437,
-0.00971015601546697));
#33692=CARTESIAN_POINT('Ctrl Pts',(-0.198071773321818,0.0102500417112847,
-0.00977626718318716));
#33693=CARTESIAN_POINT('Ctrl Pts',(-0.198069561648013,0.0100490540489262,
-0.00983262714102995));
#33694=CARTESIAN_POINT('Ctrl Pts',(-0.198067349974208,0.00984806638656765,
-0.00988898709887274));
#33695=CARTESIAN_POINT('Ctrl Pts',(-0.198069347056296,0.00965578772279335,
-0.00993642202513691));
#33696=CARTESIAN_POINT('Ctrl Pts',(-0.198075160204693,0.00944555197793135,
-0.00998088478378631));
#33697=CARTESIAN_POINT('Ctrl Pts',(-0.198078066778892,0.00934043410550035,
-0.010003116163111));
#33698=CARTESIAN_POINT('Ctrl Pts',(-0.198081932177224,0.00923078260354119,
-0.0100243883948405));
#33699=CARTESIAN_POINT('Ctrl Pts',(-0.19808658619968,0.00912232210711473,
-0.0100434533383869));
#33700=CARTESIAN_POINT('Ctrl Pts',(-0.198088913210908,0.00906809185890151,
-0.0100529858101601));
#33701=CARTESIAN_POINT('Ctrl Pts',(-0.198091436320725,0.0090141678228968,
-0.0100620138170739));
#33702=CARTESIAN_POINT('Ctrl Pts',(-0.198094455876335,0.00895538944683462,
-0.0100712781216205));
#33703=CARTESIAN_POINT('Ctrl Pts',(-0.198097475431945,0.00889661107077245,
-0.0100805424261671));
#33704=CARTESIAN_POINT('Ctrl Pts',(-0.198100994909325,0.00883295335593808,
-0.0100898876623028));
#33705=CARTESIAN_POINT('Ctrl Pts',(-0.198103763339097,0.00878494462583791,
-0.0100965688979994));
#33706=CARTESIAN_POINT('Ctrl Pts',(-0.198106531768869,0.00873693589573774,
-0.0101032501336961));
#33707=CARTESIAN_POINT('Ctrl Pts',(-0.198108544282875,0.00870460546688416,
-0.0101074843223612));
#33708=CARTESIAN_POINT('Ctrl Pts',(-0.198111034743449,0.00866571681355967,
-0.0101123992216654));
#33709=CARTESIAN_POINT('Ctrl Pts',(-0.198113525204022,0.00862682816023517,
-0.0101173141209696));
#33710=CARTESIAN_POINT('Ctrl Pts',(-0.198116496223594,0.00858136740023335,
-0.0101227934913069));
#33711=CARTESIAN_POINT('Ctrl Pts',(-0.198119644971167,0.00853477128033713,
-0.0101280274800034));
#33712=CARTESIAN_POINT('Ctrl Pts',(-0.198125942466314,0.00844157904054469,
-0.0101384954573962));
#33713=CARTESIAN_POINT('Ctrl Pts',(-0.198132947640148,0.0083438589764961,
-0.0101481254404693));
#33714=CARTESIAN_POINT('Ctrl Pts',(-0.198140881896705,0.00823760956696105,
-0.0101566869216774));
#33715=CARTESIAN_POINT('Ctrl Pts',(-0.198156750409818,0.00802511074789094,
-0.0101738098840936));
#33716=CARTESIAN_POINT('Ctrl Pts',(-0.198176338188712,0.00777849317508189,
-0.0101865293230802));
#33717=CARTESIAN_POINT('Ctrl Pts',(-0.198199421628184,0.00750212729749527,
-0.0101871140925375));
#33718=CARTESIAN_POINT('Ctrl Pts',(-0.198199421585483,0.00750212679134634,
-0.0101871140916879));
#33719=CARTESIAN_POINT('Ctrl Pts',(-0.19817611086679,0.00722581833102842,
-0.0101866502867765));
#33720=CARTESIAN_POINT('Ctrl Pts',(-0.198156325937573,0.00697926626484938,
-0.0101740436271574));
#33721=CARTESIAN_POINT('Ctrl Pts',(-0.198140292280466,0.00676682765207862,
-0.0101570226512735));
#33722=CARTESIAN_POINT('Ctrl Pts',(-0.198132275447017,0.00666060828083482,
-0.010148512158135));
#33723=CARTESIAN_POINT('Ctrl Pts',(-0.198125195705892,0.0065629169676353,
-0.0101389301595227));
#33724=CARTESIAN_POINT('Ctrl Pts',(-0.19811882975459,0.00646976830575511,
-0.0101285110517695));
#33725=CARTESIAN_POINT('Ctrl Pts',(-0.198115646778939,0.00642319397481502,
-0.0101233014978929));
#33726=CARTESIAN_POINT('Ctrl Pts',(-0.198112643055707,0.00637775867941244,
-0.0101178469343614));
#33727=CARTESIAN_POINT('Ctrl Pts',(-0.198110124028647,0.00633887748420828,
-0.0101129516600973));
#33728=CARTESIAN_POINT('Ctrl Pts',(-0.198107605001588,0.00629999628900412,
-0.0101080563858333));
#33729=CARTESIAN_POINT('Ctrl Pts',(-0.198105568069999,0.00626765542999263,
-0.0101038361134122));
#33730=CARTESIAN_POINT('Ctrl Pts',(-0.198102768660702,0.00621970700526403,
-0.0100971867469011));
#33731=CARTESIAN_POINT('Ctrl Pts',(-0.198099969251406,0.00617175858053543,
-0.0100905373803899));
#33732=CARTESIAN_POINT('Ctrl Pts',(-0.198096412203787,0.00610823162866769,
-0.0100812432595164));
#33733=CARTESIAN_POINT('Ctrl Pts',(-0.198093357310053,0.00604954828080428,
-0.0100720247747581));
#33734=CARTESIAN_POINT('Ctrl Pts',(-0.198090302416319,0.00599086493294086,
-0.0100628062899997));
#33735=CARTESIAN_POINT('Ctrl Pts',(-0.198087746225221,0.00593700044571326,
-0.0100538176925686));
#33736=CARTESIAN_POINT('Ctrl Pts',(-0.198085385863729,0.00588282738046454,
-0.0100443253007111));
#33737=CARTESIAN_POINT('Ctrl Pts',(-0.198080665140746,0.0057744812499671,
-0.0100253405169961));
#33738=CARTESIAN_POINT('Ctrl Pts',(-0.198076731913763,0.00566493425632279,
-0.0100041534600163));
#33739=CARTESIAN_POINT('Ctrl Pts',(-0.198073762684054,0.0055598002853358,
-0.0099819807918791));
#33740=CARTESIAN_POINT('Ctrl Pts',(-0.198067824224635,0.00534953234336182,
-0.00993763545560475));
#33741=CARTESIAN_POINT('Ctrl Pts',(-0.198065723172711,0.00515674447587092,
-0.0098901830470329));
#33742=CARTESIAN_POINT('Ctrl Pts',(-0.198067795176596,0.00495584284339765,
-0.00983396133677063));
#33743=CARTESIAN_POINT('Ctrl Pts',(-0.19806986718048,0.00475494121092437,
-0.00977773962650836));
#33744=CARTESIAN_POINT('Ctrl Pts',(-0.198076129141512,0.00454615886947251,
-0.00971197455341941));
#33745=CARTESIAN_POINT('Ctrl Pts',(-0.19808751697505,0.00433996447480952,
-0.00963882206161961));
#33746=CARTESIAN_POINT('Ctrl Pts',(-0.1980886606595,0.00431925629338696,
-0.0096314753290657));
#33747=CARTESIAN_POINT('Ctrl Pts',(-0.198089856071713,0.00429857301439935,
-0.00962405606956587));
#33748=CARTESIAN_POINT('Ctrl Pts',(-0.198091100757126,0.00427792906636229,
-0.00961656945493562));
#33749=CARTESIAN_POINT('Ctrl Pts',(-0.19810224958662,0.00409301820096132,
-0.0095495107514493));
#33750=CARTESIAN_POINT('Ctrl Pts',(-0.198117351628113,0.00391134860607491,
-0.00947685497202321));
#33751=CARTESIAN_POINT('Ctrl Pts',(-0.198134642942845,0.0037426810059623,
-0.00940378604143685));
#33752=CARTESIAN_POINT('Ctrl Pts',(-0.198144253824731,0.00364893195287393,
-0.00936317276984185));
#33753=CARTESIAN_POINT('Ctrl Pts',(-0.19815453763596,0.00355913397483952,
-0.00932258020023471));
#33754=CARTESIAN_POINT('Ctrl Pts',(-0.198165951518634,0.0034650713667194,
-0.00927818672101255));
#33755=CARTESIAN_POINT('Ctrl Pts',(-0.19817165845997,0.00341804006265935,
-0.00925598998140148));
#33756=CARTESIAN_POINT('Ctrl Pts',(-0.198177647851039,0.00336994309909578,
-0.00923284565855996));
#33757=CARTESIAN_POINT('Ctrl Pts',(-0.198184521108951,0.00331689198911531,
-0.00920667124833827));
#33758=CARTESIAN_POINT('Ctrl Pts',(-0.198191394366863,0.00326384087913483,
-0.00918049683811658));
#33759=CARTESIAN_POINT('Ctrl Pts',(-0.19819915453481,0.00320590715697485,
-0.00915114497768505));
#33760=CARTESIAN_POINT('Ctrl Pts',(-0.198205034234217,0.00316276107666219,
-0.00912886912670075));
#33761=CARTESIAN_POINT('Ctrl Pts',(-0.198210913933625,0.00311961499634954,
-0.00910659327571644));
#33762=CARTESIAN_POINT('Ctrl Pts',(-0.198214908743702,0.00309114345848673,
-0.00909161049026879));
#33763=CARTESIAN_POINT('Ctrl Pts',(-0.198220123131444,0.00305428016161934,
-0.00907197000303025));
#33764=CARTESIAN_POINT('Ctrl Pts',(-0.198225337519186,0.00301741686475196,
-0.00905232951579172));
#33765=CARTESIAN_POINT('Ctrl Pts',(-0.198231773934725,0.00297222742744097,
-0.00902791004712459));
#33766=CARTESIAN_POINT('Ctrl Pts',(-0.198238655187191,0.00292456530403474,
-0.00900155052998051));
#33767=CARTESIAN_POINT('Ctrl Pts',(-0.198252417653548,0.00282924132440047,
-0.00894883164345515));
#33768=CARTESIAN_POINT('Ctrl Pts',(-0.198267955385782,0.00272390777960448,
-0.00888855753184361));
#33769=CARTESIAN_POINT('Ctrl Pts',(-0.19828604862211,0.00260395376029585,
-0.00881592108484782));
#33770=CARTESIAN_POINT('',(-0.196289740186323,0.00260194423827529,-0.00877559941110405));
#33771=CARTESIAN_POINT('',(-0.195088737224831,0.00260009358768204,-0.00875100653258347));
#33772=CARTESIAN_POINT('',(-0.196289739083861,0.00260194595557777,-0.00877559392180319));
#33773=CARTESIAN_POINT('',(-0.195000274942555,0.00750353096665004,-0.0101148103080916));
#33774=CARTESIAN_POINT('Ctrl Pts',(-0.195088731428378,0.00260009275075466,
-0.00875100644688389));
#33775=CARTESIAN_POINT('Ctrl Pts',(-0.19507056550841,0.00271953784598169,
-0.00882281095420666));
#33776=CARTESIAN_POINT('Ctrl Pts',(-0.195047104552263,0.00287727544354604,
-0.00891261530507464));
#33777=CARTESIAN_POINT('Ctrl Pts',(-0.19502112831294,0.0030585954650411,
-0.00900983362472126));
#33778=CARTESIAN_POINT('Ctrl Pts',(-0.195008840275359,0.00314572278523736,
-0.00905545099263045));
#33779=CARTESIAN_POINT('Ctrl Pts',(-0.194985579883127,0.0033188059569336,
-0.00914261832470328));
#33780=CARTESIAN_POINT('Ctrl Pts',(-0.194961558956498,0.00351153316062807,
-0.00923454340707606));
#33781=CARTESIAN_POINT('Ctrl Pts',(-0.194925419797059,0.00382775789515487,
-0.00937681516219749));
#33782=CARTESIAN_POINT('Ctrl Pts',(-0.194884704941291,0.0043332136886723,
-0.00957614800626863));
#33783=CARTESIAN_POINT('Ctrl Pts',(-0.194866033057843,0.00496456833265218,
-0.00977314711040076));
#33784=CARTESIAN_POINT('Ctrl Pts',(-0.194871276563153,0.00544563633208474,
-0.00989065977731558));
#33785=CARTESIAN_POINT('Ctrl Pts',(-0.194884841613502,0.00582946020051222,
-0.00996453896154419));
#33786=CARTESIAN_POINT('Ctrl Pts',(-0.194894925268009,0.00604519454255553,
-0.0100003920022963));
#33787=CARTESIAN_POINT('Ctrl Pts',(-0.194905432082424,0.00623580302069773,
-0.0100280526202424));
#33788=CARTESIAN_POINT('Ctrl Pts',(-0.194911508299211,0.00633376414709155,
-0.0100406629644592));
#33789=CARTESIAN_POINT('Ctrl Pts',(-0.194923395497329,0.00651612336821955,
-0.0100624828569292));
#33790=CARTESIAN_POINT('Ctrl Pts',(-0.194947915530162,0.0068587387170376,
-0.0100956620679014));
#33791=CARTESIAN_POINT('Ctrl Pts',(-0.194977244056656,0.00722802825436263,
-0.0101143934759757));
#33792=CARTESIAN_POINT('Ctrl Pts',(-0.195000274942555,0.00750353096665004,
-0.0101148103080916));
#33793=CARTESIAN_POINT('',(-0.195088829404437,0.0124036829985792,-0.00874872615458748));
#33794=CARTESIAN_POINT('Ctrl Pts',(-0.195000274941086,0.00750353098422301,
-0.0101148103080518));
#33795=CARTESIAN_POINT('Ctrl Pts',(-0.19497724729087,0.00777891435449093,
-0.0101141862235937));
#33796=CARTESIAN_POINT('Ctrl Pts',(-0.194947927290943,0.00814801528533906,
-0.0100951955251351));
#33797=CARTESIAN_POINT('Ctrl Pts',(-0.19492342235388,0.00849042376455305,
-0.0100617947839754));
#33798=CARTESIAN_POINT('Ctrl Pts',(-0.194911546715732,0.0086726534583307,
-0.0100398642542001));
#33799=CARTESIAN_POINT('Ctrl Pts',(-0.194905476612654,0.00877055768838091,
-0.010027193464408));
#33800=CARTESIAN_POINT('Ctrl Pts',(-0.194894989814472,0.00896096337319932,
-0.00999943328655211));
#33801=CARTESIAN_POINT('Ctrl Pts',(-0.194884930759344,0.00917651379624448,
-0.00996346768226511));
#33802=CARTESIAN_POINT('Ctrl Pts',(-0.194871414892465,0.00956001074350432,
-0.00988940804155719));
#33803=CARTESIAN_POINT('Ctrl Pts',(-0.194866267314259,0.0100411730412217,
-0.00977154454516943));
#33804=CARTESIAN_POINT('Ctrl Pts',(-0.194885029757862,0.010671297796436,
-0.00957454608000461));
#33805=CARTESIAN_POINT('Ctrl Pts',(-0.194925805250576,0.0111770444460619,
-0.00937480202317456));
#33806=CARTESIAN_POINT('Ctrl Pts',(-0.19496188907685,0.0114928984561674,
-0.00923248932403923));
#33807=CARTESIAN_POINT('Ctrl Pts',(-0.19498587479727,0.0116854970829846,
-0.00914050560741373));
#33808=CARTESIAN_POINT('Ctrl Pts',(-0.195009096984921,0.0118584739142889,
-0.00905328224883865));
#33809=CARTESIAN_POINT('Ctrl Pts',(-0.195021362145538,0.0119455411324728,
-0.00900764103933122));
#33810=CARTESIAN_POINT('Ctrl Pts',(-0.195047288504676,0.0121267277435333,
-0.00891037903369575));
#33811=CARTESIAN_POINT('Ctrl Pts',(-0.195070701448721,0.0122843379937074,
-0.0088205465890419));
#33812=CARTESIAN_POINT('Ctrl Pts',(-0.195088829404437,0.0124036829985792,
-0.00874872615458748));
#33813=CARTESIAN_POINT('',(-0.196290666237131,0.012402736317308,-0.00877278749374763));
#33814=CARTESIAN_POINT('',(-0.195088829525986,0.0124036792402707,-0.0087487199395675));
#33815=CARTESIAN_POINT('',(-0.196200542036419,0.00750313725781679,-0.0101419374936355));
#33816=CARTESIAN_POINT('Ctrl Pts',(-0.196290664392037,0.0124027350217015,
-0.00877278488125371));
#33817=CARTESIAN_POINT('Ctrl Pts',(-0.19627237848276,0.0122827028385748,
-0.00884522665494427));
#33818=CARTESIAN_POINT('Ctrl Pts',(-0.196256673581162,0.0121773026599296,
-0.00890534564544836));
#33819=CARTESIAN_POINT('Ctrl Pts',(-0.196242762233673,0.0120819185796832,
-0.00895793228268215));
#33820=CARTESIAN_POINT('Ctrl Pts',(-0.196235806530618,0.0120342263385952,
-0.00898422571209386));
#33821=CARTESIAN_POINT('Ctrl Pts',(-0.196229300231151,0.0119890086386769,
-0.0090085850142568));
#33822=CARTESIAN_POINT('Ctrl Pts',(-0.196224027764951,0.0119521137132335,
-0.00902818212269904));
#33823=CARTESIAN_POINT('Ctrl Pts',(-0.19621875529875,0.0119152187877902,
-0.00904777923114128));
#33824=CARTESIAN_POINT('Ctrl Pts',(-0.196214714231417,0.0118867117807409,
-0.00906273491264468));
#33825=CARTESIAN_POINT('Ctrl Pts',(-0.196208771113589,0.0118435442940514,
-0.00908495482459714));
#33826=CARTESIAN_POINT('Ctrl Pts',(-0.19620282799576,0.0118003768073619,
-0.00910717473654961));
#33827=CARTESIAN_POINT('Ctrl Pts',(-0.196194987218421,0.0117424366024625,
-0.00913644284299786));
#33828=CARTESIAN_POINT('Ctrl Pts',(-0.196188042371249,0.0116893745499815,
-0.00916254679872934));
#33829=CARTESIAN_POINT('Ctrl Pts',(-0.196181097524077,0.0116363124975004,
-0.00918865075446083));
#33830=CARTESIAN_POINT('Ctrl Pts',(-0.196175045583579,0.0115881996144841,
-0.00921173723675161));
#33831=CARTESIAN_POINT('Ctrl Pts',(-0.196169278080669,0.0115411361970223,
-0.00923388702235407));
#33832=CARTESIAN_POINT('Ctrl Pts',(-0.196157743074849,0.0114470093620985,
-0.009278186593559));
#33833=CARTESIAN_POINT('Ctrl Pts',(-0.196147346135914,0.0113570811040665,
-0.00931872661950712));
#33834=CARTESIAN_POINT('Ctrl Pts',(-0.196137642854787,0.0112633381126882,
-0.00935923068811809));
#33835=CARTESIAN_POINT('Ctrl Pts',(-0.196119711067213,0.0110900998661695,
-0.00943408272473305));
#33836=CARTESIAN_POINT('Ctrl Pts',(-0.196104159211111,0.010903618744401,
-0.00950832225153081));
#33837=CARTESIAN_POINT('Ctrl Pts',(-0.196092840715868,0.0107135413899731,
-0.00957675825515148));
#33838=CARTESIAN_POINT('Ctrl Pts',(-0.196091909842126,0.0106979087449592,
-0.00958238667813743));
#33839=CARTESIAN_POINT('Ctrl Pts',(-0.196091007602874,0.0106822523640472,
-0.00958797717070507));
#33840=CARTESIAN_POINT('Ctrl Pts',(-0.19609013502917,0.0106665779486784,
-0.00959352765109829));
#33841=CARTESIAN_POINT('Ctrl Pts',(-0.19607865283047,0.0104603182930727,
-0.00966656643100897));
#33842=CARTESIAN_POINT('Ctrl Pts',(-0.196072306157994,0.0102508063682596,
-0.00973244927437508));
#33843=CARTESIAN_POINT('Ctrl Pts',(-0.196070171014414,0.0100497920320044,
-0.00978860958523751));
#33844=CARTESIAN_POINT('Ctrl Pts',(-0.196068035870834,0.00984877769574926,
-0.00984476989609994));
#33845=CARTESIAN_POINT('Ctrl Pts',(-0.196070094248627,0.00965650659372004,
-0.00989203246707846));
#33846=CARTESIAN_POINT('Ctrl Pts',(-0.196075963871027,0.00944628266376169,
-0.00993633782451496));
#33847=CARTESIAN_POINT('Ctrl Pts',(-0.196078898682228,0.00934117069878252,
-0.00995849050323321));
#33848=CARTESIAN_POINT('Ctrl Pts',(-0.196082791096299,0.00923152646979285,
-0.0099796884291423));
#33849=CARTESIAN_POINT('Ctrl Pts',(-0.196087469396512,0.00912307680290144,
-0.00999868741761622));
#33850=CARTESIAN_POINT('Ctrl Pts',(-0.196089808546619,0.00906885196945574,
-0.0100081869118532));
#33851=CARTESIAN_POINT('Ctrl Pts',(-0.196092343114862,0.00901493417674492,
-0.0100171838575576));
#33852=CARTESIAN_POINT('Ctrl Pts',(-0.196095374433549,0.00895616243316652,
-0.0100264167229923));
#33853=CARTESIAN_POINT('Ctrl Pts',(-0.196098405752237,0.00889739068958812,
-0.010035649588427));
#33854=CARTESIAN_POINT('Ctrl Pts',(-0.196101937283514,0.00883374017538179,
-0.0100449635987899));
#33855=CARTESIAN_POINT('Ctrl Pts',(-0.196104714320117,0.00878573972656593,
-0.0100516224160801));
#33856=CARTESIAN_POINT('Ctrl Pts',(-0.196107491356719,0.00873773927775008,
-0.0100582812333704));
#33857=CARTESIAN_POINT('Ctrl Pts',(-0.19610950904998,0.00870541800268859,
-0.0100625009696805));
#33858=CARTESIAN_POINT('Ctrl Pts',(-0.196112005669307,0.00866653822219212,
-0.0100673995537587));
#33859=CARTESIAN_POINT('Ctrl Pts',(-0.196114502288634,0.00862765844169564,
-0.010072298137837));
#33860=CARTESIAN_POINT('Ctrl Pts',(-0.196117480435931,0.00858220637125886,
-0.0100777597870329));
#33861=CARTESIAN_POINT('Ctrl Pts',(-0.196120636207888,0.00853561902876165,
-0.0100829772314099));
#33862=CARTESIAN_POINT('Ctrl Pts',(-0.196126947751801,0.00844244434376721,
-0.0100934121201638));
#33863=CARTESIAN_POINT('Ctrl Pts',(-0.196133966574071,0.00834474209293421,
-0.0101030131519277));
#33864=CARTESIAN_POINT('Ctrl Pts',(-0.196141914853224,0.00823851085581078,
-0.0101115512170876));
#33865=CARTESIAN_POINT('Ctrl Pts',(-0.196157811408511,0.00802604842191928,
-0.0101286273441639));
#33866=CARTESIAN_POINT('Ctrl Pts',(-0.196177428716306,0.00777946867134234,
-0.0101413224703218));
#33867=CARTESIAN_POINT('Ctrl Pts',(-0.196200542403418,0.00750313728849443,
-0.0101419374846836));
#33868=CARTESIAN_POINT('Ctrl Pts',(-0.196200542416589,0.00750313713103434,
-0.0101419374850341));
#33869=CARTESIAN_POINT('Ctrl Pts',(-0.196177284241936,0.00722677170552974,
-0.010141504463779));
#33870=CARTESIAN_POINT('Ctrl Pts',(-0.196157539522526,0.00698015070048215,
-0.0101289673247935));
#33871=CARTESIAN_POINT('Ctrl Pts',(-0.196141534742996,0.00676764915535907,
-0.0101120253286253));
#33872=CARTESIAN_POINT('Ctrl Pts',(-0.196133532353232,0.00666139838279753,
-0.0101035543305412));
#33873=CARTESIAN_POINT('Ctrl Pts',(-0.196126464215432,0.00656367714880856,
-0.0100940144642487));
#33874=CARTESIAN_POINT('Ctrl Pts',(-0.196120106043974,0.00647047985556275,
-0.0100836370516775));
#33875=CARTESIAN_POINT('Ctrl Pts',(-0.196116926958245,0.00642388120893984,
-0.0100784483453919));
#33876=CARTESIAN_POINT('Ctrl Pts',(-0.19611392617026,0.00637841690895378,
-0.0100730144654881));
#33877=CARTESIAN_POINT('Ctrl Pts',(-0.196111410478906,0.00633953041564724,
-0.010068140055752));
#33878=CARTESIAN_POINT('Ctrl Pts',(-0.196108894787553,0.0063006439223407,
-0.0100632656460158));
#33879=CARTESIAN_POINT('Ctrl Pts',(-0.196106861587228,0.00626832150873382,
-0.0100590666463675));
#33880=CARTESIAN_POINT('Ctrl Pts',(-0.196104060770134,0.00622029929122412,
-0.0100524357044143));
#33881=CARTESIAN_POINT('Ctrl Pts',(-0.19610125995304,0.00617227707371441,
-0.0100458047624611));
#33882=CARTESIAN_POINT('Ctrl Pts',(-0.196097696376481,0.00610858406790501,
-0.0100365253965468));
#33883=CARTESIAN_POINT('Ctrl Pts',(-0.196094636239161,0.00604977851394286,
-0.0100273247247253));
#33884=CARTESIAN_POINT('Ctrl Pts',(-0.19609157610184,0.00599097295998071,
-0.0100181240529037));
#33885=CARTESIAN_POINT('Ctrl Pts',(-0.196089015934455,0.00593703009000086,
-0.0100091571569817));
#33886=CARTESIAN_POINT('Ctrl Pts',(-0.196086651610151,0.00588278080726641,
-0.00999968780876252));
#33887=CARTESIAN_POINT('Ctrl Pts',(-0.196081922961544,0.00577428224179751,
-0.00998074911232417));
#33888=CARTESIAN_POINT('Ctrl Pts',(-0.196077981909559,0.00566459157770989,
-0.00995961140281356));
#33889=CARTESIAN_POINT('Ctrl Pts',(-0.19607500205802,0.00555945248426065,
-0.00993751976640365));
#33890=CARTESIAN_POINT('Ctrl Pts',(-0.196069042354942,0.00534917429736217,
-0.00989333649358383));
#33891=CARTESIAN_POINT('Ctrl Pts',(-0.196066908198774,0.00515692595402839,
-0.00984620317386021));
#33892=CARTESIAN_POINT('Ctrl Pts',(-0.196068981777312,0.00495587356963853,
-0.00979016583001711));
#33893=CARTESIAN_POINT('Ctrl Pts',(-0.196071055355851,0.00475482118524867,
-0.00973412848617402));
#33894=CARTESIAN_POINT('Ctrl Pts',(-0.196077354771034,0.00454521109940807,
-0.00966835812863127));
#33895=CARTESIAN_POINT('Ctrl Pts',(-0.196088821024484,0.00433885181007513,
-0.00959542674868746));
#33896=CARTESIAN_POINT('Ctrl Pts',(-0.196089792739332,0.00432136376253628,
-0.00958924613310358));
#33897=CARTESIAN_POINT('Ctrl Pts',(-0.196090801571326,0.00430389812924055,
-0.00958301572777096));
#33898=CARTESIAN_POINT('Ctrl Pts',(-0.196091846079231,0.0042864628553818,
-0.00957673843898767));
#33899=CARTESIAN_POINT('Ctrl Pts',(-0.196103126784216,0.00409816157032374,
-0.00950894360225902));
#33900=CARTESIAN_POINT('Ctrl Pts',(-0.196118568741884,0.00391348555761878,
-0.00943549127838421));
#33901=CARTESIAN_POINT('Ctrl Pts',(-0.196136356400838,0.00374185548860918,
-0.00936145714508957));
#33902=CARTESIAN_POINT('Ctrl Pts',(-0.196146073731612,0.00364809463139091,
-0.00932101257823032));
#33903=CARTESIAN_POINT('Ctrl Pts',(-0.196156487876551,0.00355816449055205,
-0.00928053745040833));
#33904=CARTESIAN_POINT('Ctrl Pts',(-0.196168046508536,0.00346400760203785,
-0.00923629354441179));
#33905=CARTESIAN_POINT('Ctrl Pts',(-0.196173825824529,0.00341692915778075,
-0.00921417159141352));
#33906=CARTESIAN_POINT('Ctrl Pts',(-0.196179891183077,0.0033687942155918,
-0.00919111063395478));
#33907=CARTESIAN_POINT('Ctrl Pts',(-0.196186854858822,0.00331568620136784,
-0.00916502378152004));
#33908=CARTESIAN_POINT('Ctrl Pts',(-0.196193818534566,0.00326257818714388,
-0.00913893692908531));
#33909=CARTESIAN_POINT('Ctrl Pts',(-0.196201683566926,0.00320456836380365,
-0.00910967677303251));
#33910=CARTESIAN_POINT('Ctrl Pts',(-0.196207638740065,0.00316139558869042,
-0.00908748652539309));
#33911=CARTESIAN_POINT('Ctrl Pts',(-0.196213593913204,0.0031182228135772,
-0.00906529627775366));
#33912=CARTESIAN_POINT('Ctrl Pts',(-0.196217634816342,0.00308977453463767,
-0.00905039288359229));
#33913=CARTESIAN_POINT('Ctrl Pts',(-0.196222914850236,0.00305290139557111,
-0.00903083600740598));
#33914=CARTESIAN_POINT('Ctrl Pts',(-0.196228194884131,0.00301602825650455,
-0.00901127913121967));
#33915=CARTESIAN_POINT('Ctrl Pts',(-0.196234716492052,0.00297079552253433,
-0.00898694760628085));
#33916=CARTESIAN_POINT('Ctrl Pts',(-0.196241690253741,0.00292307688435604,
-0.00896067750775797));
#33917=CARTESIAN_POINT('Ctrl Pts',(-0.196255637737435,0.00282763987953676,
-0.00890813746019911));
#33918=CARTESIAN_POINT('Ctrl Pts',(-0.196271389759889,0.00272214090200285,
-0.00884804823129562));
#33919=CARTESIAN_POINT('Ctrl Pts',(-0.196289738784128,0.00260194254294682,
-0.00877560186874003));
#33920=CARTESIAN_POINT('',(-0.22252089691926,0.00173296344499172,-0.0086607489990303));
#33921=CARTESIAN_POINT('',(-0.22131752266871,0.001732003051347,-0.00863750155434712));
#33922=CARTESIAN_POINT('',(-0.221317522515984,0.00173199629815866,-0.00863750974697598));
#33923=CARTESIAN_POINT('',(-0.220881156857209,0.0044216146108216,-0.0101613899799023));
#33924=CARTESIAN_POINT('Ctrl Pts',(-0.22131752266871,0.001732003051347,
-0.00863750155434712));
#33925=CARTESIAN_POINT('Ctrl Pts',(-0.221280608098474,0.00186237282555748,
-0.00874426915938514));
#33926=CARTESIAN_POINT('Ctrl Pts',(-0.221233212581849,0.00203562110891459,
-0.00887756445341166));
#33927=CARTESIAN_POINT('Ctrl Pts',(-0.221181445914481,0.00223503566955665,
-0.00902112143140114));
#33928=CARTESIAN_POINT('Ctrl Pts',(-0.221157385236667,0.002329669593433,
-0.00908751775139101));
#33929=CARTESIAN_POINT('Ctrl Pts',(-0.221111886300313,0.00252077303573938,
-0.00921607714287932));
#33930=CARTESIAN_POINT('Ctrl Pts',(-0.221065558612416,0.0027351991985903,
-0.00935230474791183));
#33931=CARTESIAN_POINT('Ctrl Pts',(-0.221015381104576,0.00300050906695994,
-0.00951012073222565));
#33932=CARTESIAN_POINT('Ctrl Pts',(-0.220970549456544,0.00330668853965943,
-0.00967636498042947));
#33933=CARTESIAN_POINT('Ctrl Pts',(-0.220919173025872,0.00375989492422517,
-0.00990132539660816));
#33934=CARTESIAN_POINT('Ctrl Pts',(-0.220892662923779,0.00416326457627243,
-0.0100677775881752));
#33935=CARTESIAN_POINT('Ctrl Pts',(-0.220881156857209,0.0044216146108216,
-0.0101613899799023));
#33936=CARTESIAN_POINT('',(-0.220990770344514,0.00750289496288283,-0.0107022172106033));
#33937=CARTESIAN_POINT('Ctrl Pts',(-0.220881156857209,0.0044216146108216,
-0.0101613899799023));
#33938=CARTESIAN_POINT('Ctrl Pts',(-0.220869650790639,0.00467996464537077,
-0.0102550023716294));
#33939=CARTESIAN_POINT('Ctrl Pts',(-0.22085897332715,0.00517553858083778,
-0.0104075156831151));
#33940=CARTESIAN_POINT('Ctrl Pts',(-0.220872746753963,0.00582497912567758,
-0.0105490747109447));
#33941=CARTESIAN_POINT('Ctrl Pts',(-0.220894825643282,0.00623887119176755,
-0.0106129012161888));
#33942=CARTESIAN_POINT('Ctrl Pts',(-0.220911316471387,0.00650002679818652,
-0.010645792840235));
#33943=CARTESIAN_POINT('Ctrl Pts',(-0.220928204267902,0.00673675762205502,
-0.0106690295622062));
#33944=CARTESIAN_POINT('Ctrl Pts',(-0.220938207005333,0.00686646402018735,
-0.0106790684180989));
#33945=CARTESIAN_POINT('Ctrl Pts',(-0.220958367107639,0.00712002666152971,
-0.0106952223995177));
#33946=CARTESIAN_POINT('Ctrl Pts',(-0.220976662293923,0.00733816544666396,
-0.0107019515992283));
#33947=CARTESIAN_POINT('Ctrl Pts',(-0.220990770344514,0.00750289496288283,
-0.0107022172106033));
#33948=CARTESIAN_POINT('',(-0.220878076795315,0.0105847978297417,-0.0101590210697871));
#33949=CARTESIAN_POINT('Ctrl Pts',(-0.220990765990492,0.00750294549844078,
-0.0107022170957316));
#33950=CARTESIAN_POINT('Ctrl Pts',(-0.22097656165945,0.00766781034107023,
-0.0107018419086198));
#33951=CARTESIAN_POINT('Ctrl Pts',(-0.220958128570126,0.00788622176558849,
-0.010694956094636));
#33952=CARTESIAN_POINT('Ctrl Pts',(-0.220937788273734,0.00814023517284528,
-0.0106785867159598));
#33953=CARTESIAN_POINT('Ctrl Pts',(-0.220927673950829,0.00827039995690873,
-0.0106684092823677));
#33954=CARTESIAN_POINT('Ctrl Pts',(-0.2209106107512,0.0085074164570001,
-0.0106449487005366));
#33955=CARTESIAN_POINT('Ctrl Pts',(-0.220893897670049,0.00876904348654153,
-0.0106117657537804));
#33956=CARTESIAN_POINT('Ctrl Pts',(-0.220871431947319,0.00918327907519644,
-0.0105475333080408));
#33957=CARTESIAN_POINT('Ctrl Pts',(-0.220856863313028,0.00983530374811943,
-0.0104046120531604));
#33958=CARTESIAN_POINT('Ctrl Pts',(-0.220866936794483,0.0103285626661751,
-0.0102520979581623));
#33959=CARTESIAN_POINT('Ctrl Pts',(-0.220878076795315,0.0105847978297417,
-0.0101590210697871));
#33960=CARTESIAN_POINT('',(-0.221311657438852,0.0132815265142635,-0.00862621316345587));
#33961=CARTESIAN_POINT('Ctrl Pts',(-0.220878076795315,0.0105847978297417,
-0.0101590210697871));
#33962=CARTESIAN_POINT('Ctrl Pts',(-0.220878137729977,0.0105861994097892,
-0.0101585119487601));
#33963=CARTESIAN_POINT('Ctrl Pts',(-0.22088943342552,0.0108452945702086,
-0.0100643226589043));
#33964=CARTESIAN_POINT('Ctrl Pts',(-0.220915712841839,0.0112491091634393,
-0.00989717402810534));
#33965=CARTESIAN_POINT('Ctrl Pts',(-0.220966901565007,0.0117033824356887,
-0.00967107301525563));
#33966=CARTESIAN_POINT('Ctrl Pts',(-0.221011958082026,0.0120124705433347,
-0.00950263684076823));
#33967=CARTESIAN_POINT('Ctrl Pts',(-0.221061649944544,0.0122768352979043,
-0.00934477849302234));
#33968=CARTESIAN_POINT('Ctrl Pts',(-0.221107694057363,0.0124917040509188,
-0.009207793630019));
#33969=CARTESIAN_POINT('Ctrl Pts',(-0.221152929443628,0.0126833989489049,
-0.0090783511460067));
#33970=CARTESIAN_POINT('Ctrl Pts',(-0.221176784331268,0.0127781205930578,
-0.00901163571788361));
#33971=CARTESIAN_POINT('Ctrl Pts',(-0.221228121535475,0.0129777814119194,
-0.008867344763671));
#33972=CARTESIAN_POINT('Ctrl Pts',(-0.221275085769101,0.013151123064894,
-0.00873344581796572));
#33973=CARTESIAN_POINT('Ctrl Pts',(-0.221311657037594,0.0132815289113517,
-0.00862621670222814));
#33974=CARTESIAN_POINT('',(-0.222515321099814,0.0132803985666653,-0.00864958405725804));
#33975=CARTESIAN_POINT('',(-0.222515320943395,0.013280405523687,-0.00864959244197508));
#33976=CARTESIAN_POINT('',(-0.222078175707026,0.010589795154743,-0.010183304001148));
#33977=CARTESIAN_POINT('Ctrl Pts',(-0.222515321099814,0.0132803985666653,
-0.00864958405725804));
#33978=CARTESIAN_POINT('Ctrl Pts',(-0.22247838679018,0.0131487451657634,
-0.00875812340870462));
#33979=CARTESIAN_POINT('Ctrl Pts',(-0.222431140247769,0.012974593196174,
-0.00889287803634793));
#33980=CARTESIAN_POINT('Ctrl Pts',(-0.222379701242625,0.0127754092376983,
-0.00903706435333658));
#33981=CARTESIAN_POINT('Ctrl Pts',(-0.222356407099826,0.0126836110770626,
-0.0091018905341631));
#33982=CARTESIAN_POINT('Ctrl Pts',(-0.222310370393322,0.012490449153673,
-0.00923264820054545));
#33983=CARTESIAN_POINT('Ctrl Pts',(-0.222263835967482,0.0122757574562573,
-0.0093697752596197));
#33984=CARTESIAN_POINT('Ctrl Pts',(-0.222213597622187,0.0120127350671868,
-0.0095271791305912));
#33985=CARTESIAN_POINT('Ctrl Pts',(-0.222167895914748,0.0117045189932484,
-0.00969555561414337));
#33986=CARTESIAN_POINT('Ctrl Pts',(-0.222116057296822,0.0112509721833174,
-0.00992190901452015));
#33987=CARTESIAN_POINT('Ctrl Pts',(-0.222089558267121,0.0108477787632884,
-0.0100892171625672));
#33988=CARTESIAN_POINT('Ctrl Pts',(-0.222078175707026,0.010589795154743,
-0.010183304001148));
#33989=CARTESIAN_POINT('',(-0.222191222341661,0.00750354856662756,-0.010729348089511));
#33990=CARTESIAN_POINT('Ctrl Pts',(-0.222078175707026,0.010589795154743,
-0.010183304001148));
#33991=CARTESIAN_POINT('Ctrl Pts',(-0.22206679314693,0.0103318115461975,
-0.0102773908397288));
#33992=CARTESIAN_POINT('Ctrl Pts',(-0.222056594946149,0.00983746833872088,
-0.0104306606633226));
#33993=CARTESIAN_POINT('Ctrl Pts',(-0.2220713925672,0.0091839301427948,
-0.0105742538518266));
#33994=CARTESIAN_POINT('Ctrl Pts',(-0.222094064925071,0.00876980798679073,
-0.0106386169255547));
#33995=CARTESIAN_POINT('Ctrl Pts',(-0.222110874185597,0.00850825014440612,
-0.0106718828955474));
#33996=CARTESIAN_POINT('Ctrl Pts',(-0.222128052876237,0.00827084237768706,
-0.0106954393284925));
#33997=CARTESIAN_POINT('Ctrl Pts',(-0.222138118385459,0.00814180097829653,
-0.0107055572231305));
#33998=CARTESIAN_POINT('Ctrl Pts',(-0.222158491389853,0.00788794183207559,
-0.0107220001061996));
#33999=CARTESIAN_POINT('Ctrl Pts',(-0.222176969724701,0.00766907929165035,
-0.010728960325345));
#34000=CARTESIAN_POINT('Ctrl Pts',(-0.22219122384913,0.00750355041477949,
-0.0107293482161627));
#34001=CARTESIAN_POINT('',(-0.222081204604315,0.00442193154451798,-0.0101876159050024));
#34002=CARTESIAN_POINT('Ctrl Pts',(-0.22219122368108,0.00750354845177293,
-0.010729348213144));
#34003=CARTESIAN_POINT('Ctrl Pts',(-0.222177054476964,0.00733803644934816,
-0.0107290936725269));
#34004=CARTESIAN_POINT('Ctrl Pts',(-0.222158703787922,0.00711934029188453,
-0.0107223125470692));
#34005=CARTESIAN_POINT('Ctrl Pts',(-0.222138508319268,0.0068658863078884,
-0.0107061095911713));
#34006=CARTESIAN_POINT('Ctrl Pts',(-0.222128566128202,0.00673744809951971,
-0.0106961575846219));
#34007=CARTESIAN_POINT('Ctrl Pts',(-0.222111554921162,0.00650011441462726,
-0.0106728327203371));
#34008=CARTESIAN_POINT('Ctrl Pts',(-0.222094975466172,0.00623895487711817,
-0.0106398758531691));
#34009=CARTESIAN_POINT('Ctrl Pts',(-0.222072719549722,0.00582501305167259,
-0.0105759182598013));
#34010=CARTESIAN_POINT('Ctrl Pts',(-0.222058883145086,0.00517694615728237,
-0.0104344345821352));
#34011=CARTESIAN_POINT('Ctrl Pts',(-0.22206961077245,0.00468075083121768,
-0.0102815841682815));
#34012=CARTESIAN_POINT('Ctrl Pts',(-0.222081204604315,0.00442193154451798,
-0.0101876159050024));
#34013=CARTESIAN_POINT('Ctrl Pts',(-0.222081236730105,0.00442121470034128,
-0.0101873556089765));
#34014=CARTESIAN_POINT('Ctrl Pts',(-0.222092852784074,0.00416213643488008,
-0.0100932681026557));
#34015=CARTESIAN_POINT('Ctrl Pts',(-0.222119643967736,0.0037572121452274,
-0.00992571002071133));
#34016=CARTESIAN_POINT('Ctrl Pts',(-0.222171540892955,0.00330489363448679,
-0.0097005072347765));
#34017=CARTESIAN_POINT('Ctrl Pts',(-0.222216824087379,0.00300031071146108,
-0.00953470605702957));
#34018=CARTESIAN_POINT('Ctrl Pts',(-0.22226751910141,0.00273651678297638,
-0.00937745944238771));
#34019=CARTESIAN_POINT('Ctrl Pts',(-0.22231438217505,0.00252220880427444,
-0.00924106999805114));
#34020=CARTESIAN_POINT('Ctrl Pts',(-0.222360856121196,0.00232912295519028,
-0.0091108494752828));
#34021=CARTESIAN_POINT('Ctrl Pts',(-0.222384218798713,0.00223804757091996,
-0.00904677611111708));
#34022=CARTESIAN_POINT('Ctrl Pts',(-0.222436134874479,0.00203916205828335,
-0.00890338236979424));
#34023=CARTESIAN_POINT('Ctrl Pts',(-0.222483927643371,0.0018649090272055,
-0.00876910508506613));
#34024=CARTESIAN_POINT('Ctrl Pts',(-0.222521332224266,0.00173302259371186,
-0.00866080956817125));
#34025=CARTESIAN_POINT('',(-0.220521369425964,0.00173331988493514,-0.00862374985263368));
#34026=CARTESIAN_POINT('',(-0.219242026281106,0.00197737824222187,-0.00879310176875613));
#34027=CARTESIAN_POINT('Ctrl Pts',(-0.220521098969949,0.00173330778007932,
-0.00862373486994674));
#34028=CARTESIAN_POINT('Ctrl Pts',(-0.220437463496804,0.00173270302656685,
-0.00862167993463741));
#34029=CARTESIAN_POINT('Ctrl Pts',(-0.220369227103567,0.00173229065597507,
-0.00862007045367697));
#34030=CARTESIAN_POINT('Ctrl Pts',(-0.220311184555208,0.00173215324673003,
-0.00861887697602086));
#34031=CARTESIAN_POINT('Ctrl Pts',(-0.220282122230284,0.00173208444492447,
-0.00861827939310259));
#34032=CARTESIAN_POINT('Ctrl Pts',(-0.220255615581277,0.00173208457694698,
-0.00861778610679002));
#34033=CARTESIAN_POINT('Ctrl Pts',(-0.220236891963046,0.00173207055296993,
-0.00861742606792021));
#34034=CARTESIAN_POINT('Ctrl Pts',(-0.220218168344816,0.00173205652899288,
-0.00861706602905041));
#34035=CARTESIAN_POINT('Ctrl Pts',(-0.220207227757186,0.00173202834123672,
-0.00861683924709774));
#34036=CARTESIAN_POINT('Ctrl Pts',(-0.220183160781322,0.00173231835779415,
-0.00861662965552147));
#34037=CARTESIAN_POINT('Ctrl Pts',(-0.220159093805458,0.00173260837435157,
-0.00861642006394521));
#34038=CARTESIAN_POINT('Ctrl Pts',(-0.220121900441102,0.00173321658367137,
-0.00861622767665298));
#34039=CARTESIAN_POINT('Ctrl Pts',(-0.220089219607307,0.00173419131657759,
-0.00861641983989896));
#34040=CARTESIAN_POINT('Ctrl Pts',(-0.220056538773513,0.00173516604948381,
-0.00861661200314494));
#34041=CARTESIAN_POINT('Ctrl Pts',(-0.22002837047154,0.00173650736236591,
-0.00861718864907257));
#34042=CARTESIAN_POINT('Ctrl Pts',(-0.220001719326565,0.00173796383479279,
-0.00861788694802301));
#34043=CARTESIAN_POINT('Ctrl Pts',(-0.219948417036616,0.00174087677964655,
-0.00861928354592391));
#34044=CARTESIAN_POINT('Ctrl Pts',(-0.219901183321191,0.00174424799001159,
-0.00862116963247801));
#34045=CARTESIAN_POINT('Ctrl Pts',(-0.219846041444898,0.00175121840781084,
-0.00862583421971319));
#34046=CARTESIAN_POINT('Ctrl Pts',(-0.219790899568604,0.0017581888256101,
-0.00863049880694838));
#34047=CARTESIAN_POINT('Ctrl Pts',(-0.219727849628244,0.00176876278295717,
-0.0086379366743074));
#34048=CARTESIAN_POINT('Ctrl Pts',(-0.219672835763088,0.001780783273963,
-0.00864663676002183));
#34049=CARTESIAN_POINT('Ctrl Pts',(-0.219617821897932,0.00179280376496883,
-0.00865533684573626));
#34050=CARTESIAN_POINT('Ctrl Pts',(-0.219570843848114,0.00180625926555738,
-0.00866531313618264));
#34051=CARTESIAN_POINT('Ctrl Pts',(-0.2195205738428,0.00182568220387981,
-0.00867987985899917));
#34052=CARTESIAN_POINT('Ctrl Pts',(-0.219470303837487,0.00184510514220223,
-0.0086944465818157));
#34053=CARTESIAN_POINT('Ctrl Pts',(-0.219416742624575,0.00187052796332885,
-0.00871356370743997));
#34054=CARTESIAN_POINT('Ctrl Pts',(-0.219375354713411,0.00189334849853141,
-0.00873064671564717));
#34055=CARTESIAN_POINT('Ctrl Pts',(-0.219333967134904,0.00191616885031262,
-0.00874772958654872));
#34056=CARTESIAN_POINT('Ctrl Pts',(-0.219304750253871,0.00193628767794186,
-0.00876290562638991));
#34057=CARTESIAN_POINT('Ctrl Pts',(-0.219242026281106,0.00197737824222187,
-0.00879310176875613));
#34058=CARTESIAN_POINT('',(-0.218875283101098,0.004581383707407,-0.0101734940573489));
#34059=CARTESIAN_POINT('Ctrl Pts',(-0.219242024743306,0.00197737933473877,
-0.00879310257408756));
#34060=CARTESIAN_POINT('Ctrl Pts',(-0.219210397264156,0.00210431985748318,
-0.00888947722217451));
#34061=CARTESIAN_POINT('Ctrl Pts',(-0.219169695880014,0.00227317409004623,
-0.009010265597418));
#34062=CARTESIAN_POINT('Ctrl Pts',(-0.219125114125995,0.00246844791056431,
-0.00914120233515241));
#34063=CARTESIAN_POINT('Ctrl Pts',(-0.219104107029856,0.00256264491586247,
-0.0092027760354157));
#34064=CARTESIAN_POINT('Ctrl Pts',(-0.219065185789401,0.0027495795362576,
-0.00932001390846926));
#34065=CARTESIAN_POINT('Ctrl Pts',(-0.219025709089311,0.00295899128206887,
-0.00944417732113124));
#34066=CARTESIAN_POINT('Ctrl Pts',(-0.218983512591821,0.00321686005853762,
-0.00958744196166714));
#34067=CARTESIAN_POINT('Ctrl Pts',(-0.218946533756309,0.00351210751955368,
-0.00973738318907154));
#34068=CARTESIAN_POINT('Ctrl Pts',(-0.21890460182961,0.00394769638303296,
-0.0099397871903584));
#34069=CARTESIAN_POINT('Ctrl Pts',(-0.218883863192036,0.00433227617929637,
-0.0100887511287044));
#34070=CARTESIAN_POINT('Ctrl Pts',(-0.218875329342033,0.00458003691306957,
-0.0101730362524699));
#34071=CARTESIAN_POINT('Ctrl Pts',(-0.218875283101098,0.004581383707407,
-0.0101734940573489));
#34072=CARTESIAN_POINT('',(-0.218991324367386,0.0075019122725732,-0.0106570283411247));
#34073=CARTESIAN_POINT('Ctrl Pts',(-0.218875283101098,0.004581383707407,
-0.0101734940573489));
#34074=CARTESIAN_POINT('Ctrl Pts',(-0.218866870630764,0.00482640183843447,
-0.0102567810839603));
#34075=CARTESIAN_POINT('Ctrl Pts',(-0.218860428272785,0.00530009638128035,
-0.010394044359322));
#34076=CARTESIAN_POINT('Ctrl Pts',(-0.21887680296636,0.00591647553201763,
-0.0105204386808791));
#34077=CARTESIAN_POINT('Ctrl Pts',(-0.218898906555435,0.00630803933518748,
-0.0105773429465142));
#34078=CARTESIAN_POINT('Ctrl Pts',(-0.218915046210659,0.00655448980943694,
-0.0106066073820039));
#34079=CARTESIAN_POINT('Ctrl Pts',(-0.218931315724247,0.00677698709341947,
-0.0106272402886752));
#34080=CARTESIAN_POINT('Ctrl Pts',(-0.218940988343653,0.00690018648445271,
-0.0106362673398873));
#34081=CARTESIAN_POINT('Ctrl Pts',(-0.218960350606911,0.00713991109271049,
-0.0106507120235621));
#34082=CARTESIAN_POINT('Ctrl Pts',(-0.218977853687112,0.00734620133041628,
-0.0106567570334487));
#34083=CARTESIAN_POINT('Ctrl Pts',(-0.218991324367386,0.0075019122725732,
-0.0106570283411247));
#34084=CARTESIAN_POINT('',(-0.218873033347197,0.0104354629346669,-0.0101677297475496));
#34085=CARTESIAN_POINT('Ctrl Pts',(-0.218991324487739,0.00750191366376445,
-0.0106570283435486));
#34086=CARTESIAN_POINT('Ctrl Pts',(-0.218977714066313,0.00765844874886421,
-0.0106566873977884));
#34087=CARTESIAN_POINT('Ctrl Pts',(-0.218960026395843,0.00786583414945123,
-0.010650493139574));
#34088=CARTESIAN_POINT('Ctrl Pts',(-0.218940437271565,0.00810702606773746,
-0.0106357748472563));
#34089=CARTESIAN_POINT('Ctrl Pts',(-0.218930665620513,0.00823074935764031,
-0.0106266120296459));
#34090=CARTESIAN_POINT('Ctrl Pts',(-0.218914122265686,0.00845551885065929,
-0.0106055490032873));
#34091=CARTESIAN_POINT('Ctrl Pts',(-0.218897729797661,0.00870399621762634,
-0.010575730408042));
#34092=CARTESIAN_POINT('Ctrl Pts',(-0.218875282033582,0.009098281554932,
-0.0105178852734934));
#34093=CARTESIAN_POINT('Ctrl Pts',(-0.218858574729261,0.00971840699337653,
-0.0103892973309567));
#34094=CARTESIAN_POINT('Ctrl Pts',(-0.218864545490841,0.0101899590796915,
-0.010251929948102));
#34095=CARTESIAN_POINT('Ctrl Pts',(-0.218873033347197,0.0104354629346669,
-0.0101677297475496));
#34096=CARTESIAN_POINT('',(-0.219239360238103,0.0130430516485843,-0.00877739741392787));
#34097=CARTESIAN_POINT('Ctrl Pts',(-0.218873033347197,0.0104354629346669,
-0.0101677297475496));
#34098=CARTESIAN_POINT('Ctrl Pts',(-0.218873073881679,0.0104366353592755,
-0.010167327642307));
#34099=CARTESIAN_POINT('Ctrl Pts',(-0.218881669369809,0.0106845336709657,
-0.0100822476343057));
#34100=CARTESIAN_POINT('Ctrl Pts',(-0.218910030592733,0.0112002405915132,
-0.00988053471852809));
#34101=CARTESIAN_POINT('Ctrl Pts',(-0.218966215343186,0.0117059336228815,
-0.00963087579587884));
#34102=CARTESIAN_POINT('Ctrl Pts',(-0.219024577480456,0.0120623302121355,
-0.00943183626992845));
#34103=CARTESIAN_POINT('Ctrl Pts',(-0.219063926983141,0.0122714635384721,
-0.00930705603696086));
#34104=CARTESIAN_POINT('Ctrl Pts',(-0.219102562059971,0.0124578218778547,
-0.00918947672058609));
#34105=CARTESIAN_POINT('Ctrl Pts',(-0.219123412166533,0.0125519183301058,
-0.00912760747078243));
#34106=CARTESIAN_POINT('Ctrl Pts',(-0.219167638695722,0.0127470745854724,
-0.00899597806498157));
#34107=CARTESIAN_POINT('Ctrl Pts',(-0.219207998992883,0.0129160142680807,
-0.00887442197202375));
#34108=CARTESIAN_POINT('Ctrl Pts',(-0.219239355956135,0.0130430487440735,
-0.00877739980923923));
#34109=CARTESIAN_POINT('',(-0.220511173800118,0.0132638184474622,-0.00862591209587123));
#34110=CARTESIAN_POINT('Ctrl Pts',(-0.219239360856092,0.0130430506754479,
-0.00877739805133272));
#34111=CARTESIAN_POINT('Ctrl Pts',(-0.219298950996701,0.0130687144123312,
-0.00875880433339075));
#34112=CARTESIAN_POINT('Ctrl Pts',(-0.219358531392433,0.0130945392596808,
-0.00873977229127666));
#34113=CARTESIAN_POINT('Ctrl Pts',(-0.219411335221623,0.0131167513828459,
-0.00872328489173723));
#34114=CARTESIAN_POINT('Ctrl Pts',(-0.219464140496835,0.013138964114286,
-0.00870679704069332));
#34115=CARTESIAN_POINT('Ctrl Pts',(-0.219500760265905,0.013153861192503,
-0.00869564715063633));
#34116=CARTESIAN_POINT('Ctrl Pts',(-0.219546226692826,0.0131713559086997,
-0.0086825393609088));
#34117=CARTESIAN_POINT('Ctrl Pts',(-0.219591693119748,0.0131888506248964,
-0.00866943157118127));
#34118=CARTESIAN_POINT('Ctrl Pts',(-0.21964621378914,0.0132085111685916,
-0.00865465912376249));
#34119=CARTESIAN_POINT('Ctrl Pts',(-0.219698198990407,0.0132250723510747,
-0.00864224352548852));
#34120=CARTESIAN_POINT('Ctrl Pts',(-0.219750184191674,0.0132416335335577,
-0.00862982792721455));
#34121=CARTESIAN_POINT('Ctrl Pts',(-0.219799465343604,0.0132554691542827,
-0.00861948547653094));
#34122=CARTESIAN_POINT('Ctrl Pts',(-0.219852540605556,0.0132676479975295,
-0.00861050659516199));
#34123=CARTESIAN_POINT('Ctrl Pts',(-0.219905615867508,0.0132798268407764,
-0.00860152771379304));
#34124=CARTESIAN_POINT('Ctrl Pts',(-0.219962601807985,0.0132900276350841,
-0.00859416917716125));
#34125=CARTESIAN_POINT('Ctrl Pts',(-0.22001809697308,0.0132963990632951,
-0.00858991670627559));
#34126=CARTESIAN_POINT('Ctrl Pts',(-0.220073592138176,0.0133027704915062,
-0.00858566423538993));
#34127=CARTESIAN_POINT('Ctrl Pts',(-0.220127543994927,0.0133055155736895,
-0.00858435336394495));
#34128=CARTESIAN_POINT('Ctrl Pts',(-0.220180503294847,0.0133043243406397,
-0.00858630552910945));
#34129=CARTESIAN_POINT('Ctrl Pts',(-0.220206982944806,0.0133037287241147,
-0.0085872816116917));
#34130=CARTESIAN_POINT('Ctrl Pts',(-0.220232730829742,0.0133021797482245,
-0.00858903927174345));
#34131=CARTESIAN_POINT('Ctrl Pts',(-0.22026032775548,0.013299662179195,
-0.00859163540799559));
#34132=CARTESIAN_POINT('Ctrl Pts',(-0.220287924681219,0.0132971446101655,
-0.00859423154424774));
#34133=CARTESIAN_POINT('Ctrl Pts',(-0.22031735564104,0.0132935272221941,
-0.00859777443096918));
#34134=CARTESIAN_POINT('Ctrl Pts',(-0.220343331894914,0.0132899564633698,
-0.00860121291144217));
#34135=CARTESIAN_POINT('Ctrl Pts',(-0.220369308148789,0.0132863857045454,
-0.00860465139191516));
#34136=CARTESIAN_POINT('Ctrl Pts',(-0.22037830388446,0.0132847864229076,
-0.00860614092202279));
#34137=CARTESIAN_POINT('Ctrl Pts',(-0.22040632557493,0.0132804512126285,
-0.00861024553754777));
#34138=CARTESIAN_POINT('Ctrl Pts',(-0.220434276772263,0.0132761269082787,
-0.00861433982724225));
#34139=CARTESIAN_POINT('Ctrl Pts',(-0.220465993395677,0.0132709838364459,
-0.00861918120032084));
#34140=CARTESIAN_POINT('Ctrl Pts',(-0.220510858531432,0.0132638681299273,
-0.00862586523173163));
#34141=CARTESIAN_POINT('',(-0.220090131945959,0.0108157693199988,-0.0100543335553095));
#34142=CARTESIAN_POINT('Ctrl Pts',(-0.220511198231108,0.0132638143311653,
-0.00862591593995484));
#34143=CARTESIAN_POINT('Ctrl Pts',(-0.220474612184434,0.013132908947053,
-0.00873278603088295));
#34144=CARTESIAN_POINT('Ctrl Pts',(-0.220427708291213,0.0129593513417706,
-0.00886587344975926));
#34145=CARTESIAN_POINT('Ctrl Pts',(-0.220376512267889,0.0127601128577709,
-0.00900883800189919));
#34146=CARTESIAN_POINT('Ctrl Pts',(-0.220353002206104,0.0126668690042777,
-0.00907408224202567));
#34147=CARTESIAN_POINT('Ctrl Pts',(-0.220307516279135,0.0124745968776834,
-0.00920306768613607));
#34148=CARTESIAN_POINT('Ctrl Pts',(-0.220261403766907,0.0122600991432045,
-0.009338899311862));
#34149=CARTESIAN_POINT('Ctrl Pts',(-0.220211695130772,0.0119970268718438,
-0.00949498790625071));
#34150=CARTESIAN_POINT('Ctrl Pts',(-0.220166577384904,0.0116890499212551,
-0.009661813304815));
#34151=CARTESIAN_POINT('Ctrl Pts',(-0.220123247623221,0.011305666268294,
-0.00985154441700039));
#34152=CARTESIAN_POINT('Ctrl Pts',(-0.220100481153719,0.0109961152750341,
-0.00998355150383413));
#34153=CARTESIAN_POINT('Ctrl Pts',(-0.220090131945959,0.0108157693199988,
-0.0100543335553095));
#34154=CARTESIAN_POINT('',(-0.22019175144594,0.00750243957431793,-0.010684158764387));
#34155=CARTESIAN_POINT('Ctrl Pts',(-0.220090131945959,0.0108157693199988,
-0.0100543335553095));
#34156=CARTESIAN_POINT('Ctrl Pts',(-0.220085557370637,0.0107360524784264,
-0.0100856207642881));
#34157=CARTESIAN_POINT('Ctrl Pts',(-0.22006845689036,0.0103958729688586,
-0.0102140461491421));
#34158=CARTESIAN_POINT('Ctrl Pts',(-0.220057020156484,0.00982779650229385,
-0.0103888558048875));
#34159=CARTESIAN_POINT('Ctrl Pts',(-0.220072085364924,0.00917638566997734,
-0.0105309147603936));
#34160=CARTESIAN_POINT('Ctrl Pts',(-0.220094819050192,0.00876357564947826,
-0.0105945725520012));
#34161=CARTESIAN_POINT('Ctrl Pts',(-0.220111615632777,0.00850307729270115,
-0.0106274384754032));
#34162=CARTESIAN_POINT('Ctrl Pts',(-0.220128755043961,0.00826671083837223,
-0.0106507003321801));
#34163=CARTESIAN_POINT('Ctrl Pts',(-0.220138784930233,0.00813832419183378,
-0.010660684037487));
#34164=CARTESIAN_POINT('Ctrl Pts',(-0.22015910220265,0.00788550868615409,
-0.0106769231726282));
#34165=CARTESIAN_POINT('Ctrl Pts',(-0.220177533161667,0.00766742881797243,
-0.0106837925977353));
#34166=CARTESIAN_POINT('Ctrl Pts',(-0.22019175281392,0.00750244141589442,
-0.0106841588886674));
#34167=CARTESIAN_POINT('',(-0.220081376539163,0.00442299110476343,-0.0101444921821041));
#34168=CARTESIAN_POINT('Ctrl Pts',(-0.220191752647251,0.00750243947116139,
-0.0106841588854298));
#34169=CARTESIAN_POINT('Ctrl Pts',(-0.220177578180119,0.00733704887202067,
-0.0106838835219745));
#34170=CARTESIAN_POINT('Ctrl Pts',(-0.22015922048139,0.00711852767169112,
-0.0106771046134885));
#34171=CARTESIAN_POINT('Ctrl Pts',(-0.220139015624589,0.00686530054035368,
-0.0106609453039589));
#34172=CARTESIAN_POINT('Ctrl Pts',(-0.220129069993647,0.00673700584535355,
-0.010651026291088));
#34173=CARTESIAN_POINT('Ctrl Pts',(-0.220112044459368,0.00649988309557624,
-0.0106277828308853));
#34174=CARTESIAN_POINT('Ctrl Pts',(-0.220095442997511,0.00623893652743939,
-0.0105949464252065));
#34175=CARTESIAN_POINT('Ctrl Pts',(-0.220073138675426,0.00582541150882776,
-0.0105312604256392));
#34176=CARTESIAN_POINT('Ctrl Pts',(-0.220059160562007,0.00517687267843841,
-0.0103901109544776));
#34177=CARTESIAN_POINT('Ctrl Pts',(-0.220069811611103,0.00468149176814678,
-0.010238002757777));
#34178=CARTESIAN_POINT('Ctrl Pts',(-0.220081376539163,0.00442299110476343,
-0.0101444921821041));
#34179=CARTESIAN_POINT('Ctrl Pts',(-0.22008140790703,0.00442229028145444,
-0.0101442386316291));
#34180=CARTESIAN_POINT('Ctrl Pts',(-0.220092994577836,0.00416353624782033,
-0.010050611906748));
#34181=CARTESIAN_POINT('Ctrl Pts',(-0.22011975529717,0.00375896969551987,
-0.00988387768562756));
#34182=CARTESIAN_POINT('Ctrl Pts',(-0.220171662014429,0.00330655391001369,
-0.0096595890396178));
#34183=CARTESIAN_POINT('Ctrl Pts',(-0.220217007334562,0.00300150929740094,
-0.00949424527209877));
#34184=CARTESIAN_POINT('Ctrl Pts',(-0.220267680085307,0.00273767985326313,
-0.00933766032672383));
#34185=CARTESIAN_POINT('Ctrl Pts',(-0.220314530683991,0.00252326153527256,
-0.00920181247202401));
#34186=CARTESIAN_POINT('Ctrl Pts',(-0.220360978000976,0.00233010820899768,
-0.0090721446842305));
#34187=CARTESIAN_POINT('Ctrl Pts',(-0.220384350015444,0.00223890246433455,
-0.00900828010102458));
#34188=CARTESIAN_POINT('Ctrl Pts',(-0.220436257236716,0.00203984277084597,
-0.00886543629554137));
#34189=CARTESIAN_POINT('Ctrl Pts',(-0.220484038290209,0.00186542210487714,
-0.00873168119613634));
#34190=CARTESIAN_POINT('Ctrl Pts',(-0.2205214329925,0.00173338441996231,
-0.00862380411186018));
#34191=CARTESIAN_POINT('',(-0.218374793789608,0.00221918351113939,-0.0089535596216209));
#34192=CARTESIAN_POINT('',(-0.217726229879918,0.00223894560702424,-0.00895610833897201));
#34193=CARTESIAN_POINT('Ctrl Pts',(-0.218375409693209,0.00221079122986865,
-0.00894874908347634));
#34194=CARTESIAN_POINT('Ctrl Pts',(-0.218295547237171,0.00221203449658772,
-0.00894808355786149));
#34195=CARTESIAN_POINT('Ctrl Pts',(-0.218197262847863,0.00221365986816565,
-0.00894733157532527));
#34196=CARTESIAN_POINT('Ctrl Pts',(-0.218095525843496,0.00221584476839926,
-0.00894690951729281));
#34197=CARTESIAN_POINT('Ctrl Pts',(-0.21806412726539,0.00221644786389076,
-0.00894672852039272));
#34198=CARTESIAN_POINT('Ctrl Pts',(-0.217956617159952,0.00222021619904336,
-0.00894731928771769));
#34199=CARTESIAN_POINT('Ctrl Pts',(-0.217848140139888,0.0022267806586541,
-0.00894987064576114));
#34200=CARTESIAN_POINT('Ctrl Pts',(-0.217779211918502,0.00223241879127506,
-0.00895252955645527));
#34201=CARTESIAN_POINT('Ctrl Pts',(-0.217726229879918,0.00223894560702424,
-0.00895610833897201));
#34202=CARTESIAN_POINT('',(-0.217123286376409,0.00243485131310274,-0.00907883473156682));
#34203=CARTESIAN_POINT('Ctrl Pts',(-0.217725491044994,0.0022390367465584,
-0.00895615833124103));
#34204=CARTESIAN_POINT('Ctrl Pts',(-0.217672196328649,0.00224561982685404,
-0.00895977065528357));
#34205=CARTESIAN_POINT('Ctrl Pts',(-0.217551154797832,0.00226440842063028,
-0.00897066068600668));
#34206=CARTESIAN_POINT('Ctrl Pts',(-0.217408393547704,0.00230150415104225,
-0.00899375480814277));
#34207=CARTESIAN_POINT('Ctrl Pts',(-0.217285693066462,0.00234646807569697,
-0.00902240631599514));
#34208=CARTESIAN_POINT('Ctrl Pts',(-0.217185031478673,0.00239905726908142,
-0.00905606193974296));
#34209=CARTESIAN_POINT('Ctrl Pts',(-0.217158224898363,0.00241473880623142,
-0.00906610084421658));
#34210=CARTESIAN_POINT('Ctrl Pts',(-0.217123288446565,0.00243483964324871,
-0.00907882698336438));
#34211=CARTESIAN_POINT('',(-0.216865219429701,0.00485302928795331,-0.0102164733809617));
#34212=CARTESIAN_POINT('Ctrl Pts',(-0.217123286376409,0.00243485131310274,
-0.00907883473156682));
#34213=CARTESIAN_POINT('Ctrl Pts',(-0.217102113171765,0.00255420866614419,
-0.00915808195356356));
#34214=CARTESIAN_POINT('Ctrl Pts',(-0.21708380628641,0.00266021556918632,
-0.0092245717761884));
#34215=CARTESIAN_POINT('Ctrl Pts',(-0.217067506905344,0.00275710066248676,
-0.009283221761031));
#34216=CARTESIAN_POINT('Ctrl Pts',(-0.217059356949207,0.00280554478791243,
-0.00931254770917369));
#34217=CARTESIAN_POINT('Ctrl Pts',(-0.217051709940288,0.00285174138298016,
-0.00933986164713557));
#34218=CARTESIAN_POINT('Ctrl Pts',(-0.217045421662262,0.00289008361015183,
-0.00936219529050879));
#34219=CARTESIAN_POINT('Ctrl Pts',(-0.217039133384235,0.0029284258373235,
-0.009384528933882));
#34220=CARTESIAN_POINT('Ctrl Pts',(-0.21703420124665,0.00295883822773935,
-0.00940200972756825));
#34221=CARTESIAN_POINT('Ctrl Pts',(-0.217027206770864,0.00300335905250413,
-0.00942710119986508));
#34222=CARTESIAN_POINT('Ctrl Pts',(-0.217020212295079,0.00304787987726892,
-0.0094521926721619));
#34223=CARTESIAN_POINT('Ctrl Pts',(-0.217011160118175,0.00310663789704563,
-0.00948466851452673));
#34224=CARTESIAN_POINT('Ctrl Pts',(-0.217003118562495,0.00316070130514153,
-0.00951375775303658));
#34225=CARTESIAN_POINT('Ctrl Pts',(-0.216995077006816,0.00321476471323742,
-0.00954284699154643));
#34226=CARTESIAN_POINT('Ctrl Pts',(-0.216988042899663,0.00326405254348306,
-0.00956870246583691));
#34227=CARTESIAN_POINT('Ctrl Pts',(-0.216981348057688,0.00331234769037973,
-0.00959353732849681));
#34228=CARTESIAN_POINT('Ctrl Pts',(-0.216967958373738,0.00340893798417307,
-0.0096432070538166));
#34229=CARTESIAN_POINT('Ctrl Pts',(-0.21695592618917,0.00350156050347066,
-0.00968877543301438));
#34230=CARTESIAN_POINT('Ctrl Pts',(-0.216944760158758,0.00359749171350427,
-0.00973398076094292));
#34231=CARTESIAN_POINT('Ctrl Pts',(-0.216922771495283,0.0037864038887724,
-0.00982300118328198));
#34232=CARTESIAN_POINT('Ctrl Pts',(-0.21690415162039,0.00398835918519624,
-0.00991015012701886));
#34233=CARTESIAN_POINT('Ctrl Pts',(-0.216890742090616,0.00419768307541563,
-0.00999111343977628));
#34234=CARTESIAN_POINT('Ctrl Pts',(-0.216890532673751,0.00420095209032992,
-0.00999237784527073));
#34235=CARTESIAN_POINT('Ctrl Pts',(-0.216890324527644,0.00420422288475571,
-0.00999364077261011));
#34236=CARTESIAN_POINT('Ctrl Pts',(-0.216890117659308,0.0042074954350809,
-0.00999490220917792));
#34237=CARTESIAN_POINT('Ctrl Pts',(-0.216876664450443,0.00442031825757234,
-0.010076936850079));
#34238=CARTESIAN_POINT('Ctrl Pts',(-0.216868621236676,0.00464079347560287,
-0.0101522452372161));
#34239=CARTESIAN_POINT('Ctrl Pts',(-0.216865269537596,0.00484988229780852,
-0.010215521621625));
#34240=CARTESIAN_POINT('Ctrl Pts',(-0.216865252717512,0.00485093158400454,
-0.0102158391662741));
#34241=CARTESIAN_POINT('Ctrl Pts',(-0.21686523601491,0.00485198057392772,
-0.0102161564384166));
#34242=CARTESIAN_POINT('Ctrl Pts',(-0.216865219429701,0.00485302928795331,
-0.0102164733809617));
#34243=CARTESIAN_POINT('',(-0.216992039098873,0.00750111755777987,-0.0106118430505361));
#34244=CARTESIAN_POINT('Ctrl Pts',(-0.216865219429701,0.00485302928795331,
-0.0102164733809617));
#34245=CARTESIAN_POINT('Ctrl Pts',(-0.216861931118884,0.0050609521426977,
-0.0102793244231641));
#34246=CARTESIAN_POINT('Ctrl Pts',(-0.216863257542664,0.0052573906192139,
-0.0103315033714261));
#34247=CARTESIAN_POINT('Ctrl Pts',(-0.216868505685461,0.00547448632452407,
-0.0103809849429286));
#34248=CARTESIAN_POINT('Ctrl Pts',(-0.216871142991853,0.00558358165851651,
-0.0104058505134466));
#34249=CARTESIAN_POINT('Ctrl Pts',(-0.216874776812353,0.00569795300210121,
-0.0104297581638601));
#34250=CARTESIAN_POINT('Ctrl Pts',(-0.216879266843606,0.00581122729905882,
-0.0104511884062416));
#34251=CARTESIAN_POINT('Ctrl Pts',(-0.216881511859233,0.00586786444753763,
-0.0104619035274324));
#34252=CARTESIAN_POINT('Ctrl Pts',(-0.216883969709047,0.00592421706211528,
-0.01047205379377));
#34253=CARTESIAN_POINT('Ctrl Pts',(-0.216886933193732,0.00598565404839195,
-0.0104824658612332));
#34254=CARTESIAN_POINT('Ctrl Pts',(-0.216889896678417,0.00604709103466862,
-0.0104928779286964));
#34255=CARTESIAN_POINT('Ctrl Pts',(-0.216893369691221,0.00611364246361058,
-0.0105033779096584));
#34256=CARTESIAN_POINT('Ctrl Pts',(-0.216896123391226,0.00616408061379814,
-0.0105109157434318));
#34257=CARTESIAN_POINT('Ctrl Pts',(-0.216898877091231,0.00621451876398571,
-0.0105184535772053));
#34258=CARTESIAN_POINT('Ctrl Pts',(-0.216900906026196,0.00624880836994755,
-0.0105232721194047));
#34259=CARTESIAN_POINT('Ctrl Pts',(-0.216903405858141,0.00628979497340091,
-0.0105288248191684));
#34260=CARTESIAN_POINT('Ctrl Pts',(-0.216905905690085,0.00633078157685427,
-0.010534377518932));
#34261=CARTESIAN_POINT('Ctrl Pts',(-0.216908879346214,0.00637848184697154,
-0.0105405341876129));
#34262=CARTESIAN_POINT('Ctrl Pts',(-0.216912033183608,0.00642730938192668,
-0.0105464029380313));
#34263=CARTESIAN_POINT('Ctrl Pts',(-0.216918340858396,0.00652496445183697,
-0.010558140438868));
#34264=CARTESIAN_POINT('Ctrl Pts',(-0.216925365659119,0.00662711239577533,
-0.0105688859918395));
#34265=CARTESIAN_POINT('Ctrl Pts',(-0.2169333224102,0.00673786809107805,
-0.0105783972974196));
#34266=CARTESIAN_POINT('Ctrl Pts',(-0.216949235882187,0.00695937906166578,
-0.0105974198725104));
#34267=CARTESIAN_POINT('Ctrl Pts',(-0.216968880550106,0.00721532289054462,
-0.0106113550043929));
#34268=CARTESIAN_POINT('Ctrl Pts',(-0.21699203903428,0.00750111756314772,
-0.0106118429721946));
#34269=CARTESIAN_POINT('',(-0.216863263875865,0.0101606619361279,-0.010212275920378));
#34270=CARTESIAN_POINT('Ctrl Pts',(-0.216992039166016,0.00750111918887558,
-0.0106118429749703));
#34271=CARTESIAN_POINT('Ctrl Pts',(-0.216968632225441,0.00778826296106311,
-0.0106112783068527));
#34272=CARTESIAN_POINT('Ctrl Pts',(-0.216948771168368,0.00804539121894196,
-0.0105971483131848));
#34273=CARTESIAN_POINT('Ctrl Pts',(-0.216932675029404,0.00826792612051201,
-0.0105778926417949));
#34274=CARTESIAN_POINT('Ctrl Pts',(-0.216924626959922,0.00837919357129703,
-0.0105682648061));
#34275=CARTESIAN_POINT('Ctrl Pts',(-0.216917519271334,0.00848181317185611,
-0.0105573930115986));
#34276=CARTESIAN_POINT('Ctrl Pts',(-0.216911135474933,0.00857989135437507,
-0.0105455248340113));
#34277=CARTESIAN_POINT('Ctrl Pts',(-0.216907943576732,0.00862893044563455,
-0.0105395907452177));
#34278=CARTESIAN_POINT('Ctrl Pts',(-0.21690493355368,0.00867683009665796,
-0.010533367524606));
#34279=CARTESIAN_POINT('Ctrl Pts',(-0.216902401326156,0.00871801683620453,
-0.0105277512234802));
#34280=CARTESIAN_POINT('Ctrl Pts',(-0.216899869098632,0.00875920357575109,
-0.0105221349223544));
#34281=CARTESIAN_POINT('Ctrl Pts',(-0.216897811733291,0.00879369422056019,
-0.0105172560114583));
#34282=CARTESIAN_POINT('Ctrl Pts',(-0.216895024263018,0.00884428163387125,
-0.0105096476733168));
#34283=CARTESIAN_POINT('Ctrl Pts',(-0.216892236792745,0.00889486904718231,
-0.0105020393351752));
#34284=CARTESIAN_POINT('Ctrl Pts',(-0.21688872467329,0.00896151771075859,
-0.0104914585369431));
#34285=CARTESIAN_POINT('Ctrl Pts',(-0.216885723173758,0.00902305138276646,
-0.0104809685050821));
#34286=CARTESIAN_POINT('Ctrl Pts',(-0.216882721674225,0.00908458505477434,
-0.0104704784732212));
#34287=CARTESIAN_POINT('Ctrl Pts',(-0.216880226901671,0.00914103396809379,
-0.0104602530991236));
#34288=CARTESIAN_POINT('Ctrl Pts',(-0.216877944706416,0.00919776531074823,
-0.0104494608864153));
#34289=CARTESIAN_POINT('Ctrl Pts',(-0.216873380315907,0.0093112279960571,
-0.0104278764609987));
#34290=CARTESIAN_POINT('Ctrl Pts',(-0.216869671153504,0.00942577893288784,
-0.0104038046864359));
#34291=CARTESIAN_POINT('Ctrl Pts',(-0.216866955637489,0.00953491448523924,
-0.0103788076593657));
#34292=CARTESIAN_POINT('Ctrl Pts',(-0.216861524605459,0.00975318558994206,
-0.0103288136052253));
#34293=CARTESIAN_POINT('Ctrl Pts',(-0.21686004247206,0.00995004301390614,
-0.0102762708499468));
#34294=CARTESIAN_POINT('Ctrl Pts',(-0.216863248962655,0.0101596890081031,
-0.0102125715953075));
#34295=CARTESIAN_POINT('Ctrl Pts',(-0.216863253922439,0.0101600132874919,
-0.0102124730656149));
#34296=CARTESIAN_POINT('Ctrl Pts',(-0.216863258893508,0.0101603375965186,
-0.0102123745061583));
#34297=CARTESIAN_POINT('Ctrl Pts',(-0.216863263875865,0.0101606619361279,
-0.010212275920378));
#34298=CARTESIAN_POINT('',(-0.217121128085406,0.012579797101843,-0.00906899462937275));
#34299=CARTESIAN_POINT('Ctrl Pts',(-0.216863263875865,0.0101606619361279,
-0.010212275920378));
#34300=CARTESIAN_POINT('Ctrl Pts',(-0.21686647997781,0.0103700218636815,
-0.0101486367803184));
#34301=CARTESIAN_POINT('Ctrl Pts',(-0.21687439950964,0.010591699526372,
-0.0100726047017749));
#34302=CARTESIAN_POINT('Ctrl Pts',(-0.216887811284844,0.01080539853155,
-0.00998985337042852));
#34303=CARTESIAN_POINT('Ctrl Pts',(-0.216901243837455,0.0110194285973771,
-0.00990697384143589));
#34304=CARTESIAN_POINT('Ctrl Pts',(-0.216920179082265,0.0112256173796445,
-0.00981766775388043));
#34305=CARTESIAN_POINT('Ctrl Pts',(-0.216942545157854,0.0114176480916229,
-0.00972674550743857));
#34306=CARTESIAN_POINT('Ctrl Pts',(-0.216953728195649,0.0115136634476121,
-0.00968128438421765));
#34307=CARTESIAN_POINT('Ctrl Pts',(-0.216965766307836,0.011606196353727,
-0.00963554356500761));
#34308=CARTESIAN_POINT('Ctrl Pts',(-0.216979152369634,0.0117026516621678,
-0.00958571758408353));
#34309=CARTESIAN_POINT('Ctrl Pts',(-0.216985845400533,0.0117508793163882,
-0.0095608045936215));
#34310=CARTESIAN_POINT('Ctrl Pts',(-0.21699287531768,0.0118000881067751,
-0.00953487462933585));
#34311=CARTESIAN_POINT('Ctrl Pts',(-0.217000911950288,0.0118540545891475,
-0.00950570975585976));
#34312=CARTESIAN_POINT('Ctrl Pts',(-0.217008948582896,0.0119080210715199,
-0.00947654488238367));
#34313=CARTESIAN_POINT('Ctrl Pts',(-0.217017995097714,0.0119666640174066,
-0.00944399243305965));
#34314=CARTESIAN_POINT('Ctrl Pts',(-0.21702497551412,0.0120110411913712,
-0.00941887608284972));
#34315=CARTESIAN_POINT('Ctrl Pts',(-0.217031955930525,0.0120554183653357,
-0.00939375973263978));
#34316=CARTESIAN_POINT('Ctrl Pts',(-0.217036865614439,0.012085659087643,
-0.00937630582863259));
#34317=CARTESIAN_POINT('Ctrl Pts',(-0.217043142812678,0.0121239056967825,
-0.00935393704026712));
#34318=CARTESIAN_POINT('Ctrl Pts',(-0.217049420010916,0.012162152305922,
-0.00933156825190165));
#34319=CARTESIAN_POINT('Ctrl Pts',(-0.21705706731629,0.0122083289073836,
-0.00930415691288176));
#34320=CARTESIAN_POINT('Ctrl Pts',(-0.217065224007411,0.0122568003427244,
-0.0092746964595612));
#34321=CARTESIAN_POINT('Ctrl Pts',(-0.217081537389652,0.0123537432134059,
-0.00921577555292007));
#34322=CARTESIAN_POINT('Ctrl Pts',(-0.217099884128624,0.0124599993389447,
-0.00914886769251459));
#34323=CARTESIAN_POINT('Ctrl Pts',(-0.217121128085406,0.012579797101843,
-0.00906899462937275));
#34324=CARTESIAN_POINT('',(-0.218370318086279,0.0127783343977889,-0.00895639519171424));
#34325=CARTESIAN_POINT('Ctrl Pts',(-0.217121134551835,0.0125797994500258,
-0.00906899318316964));
#34326=CARTESIAN_POINT('Ctrl Pts',(-0.217191804233479,0.0126054620271479,
-0.00905318806274778));
#34327=CARTESIAN_POINT('Ctrl Pts',(-0.217256223599339,0.0126283520543175,
-0.00903890986338815));
#34328=CARTESIAN_POINT('Ctrl Pts',(-0.217302115212182,0.0126446977363176,
-0.0090286476961318));
#34329=CARTESIAN_POINT('Ctrl Pts',(-0.217348008224749,0.0126610439168714,
-0.00901838521587279));
#34330=CARTESIAN_POINT('Ctrl Pts',(-0.217375371780285,0.0126708651259043,
-0.00901216817068204));
#34331=CARTESIAN_POINT('Ctrl Pts',(-0.217421043282157,0.0126856582776629,
-0.00900283837934702));
#34332=CARTESIAN_POINT('Ctrl Pts',(-0.217466714784029,0.0127004514294214,
-0.008993508588012));
#34333=CARTESIAN_POINT('Ctrl Pts',(-0.217530695084449,0.0127201865022325,
-0.00898102254617446));
#34334=CARTESIAN_POINT('Ctrl Pts',(-0.217583564792478,0.0127352872287596,
-0.00897146523766335));
#34335=CARTESIAN_POINT('Ctrl Pts',(-0.217636434500507,0.0127503879552868,
-0.00896190792915224));
#34336=CARTESIAN_POINT('Ctrl Pts',(-0.217678193008114,0.0127608763428775,
-0.00895531057012255));
#34337=CARTESIAN_POINT('Ctrl Pts',(-0.217729528732368,0.0127712441764474,
-0.0089489621938623));
#34338=CARTESIAN_POINT('Ctrl Pts',(-0.217780864456622,0.0127816120100172,
-0.00894261381760204));
#34339=CARTESIAN_POINT('Ctrl Pts',(-0.217841777631961,0.0127918506441235,
-0.00893650234048543));
#34340=CARTESIAN_POINT('Ctrl Pts',(-0.217895152298986,0.0127988050770367,
-0.00893256964675583));
#34341=CARTESIAN_POINT('Ctrl Pts',(-0.217948526966011,0.0128057595099498,
-0.00892863695302623));
#34342=CARTESIAN_POINT('Ctrl Pts',(-0.217994363019984,0.012809433646628,
-0.00892688845320798));
#34343=CARTESIAN_POINT('Ctrl Pts',(-0.21805055697462,0.0128092199536068,
-0.0089281316531678));
#34344=CARTESIAN_POINT('Ctrl Pts',(-0.218106750929257,0.0128090062605855,
-0.00892937485312762));
#34345=CARTESIAN_POINT('Ctrl Pts',(-0.218173302827974,0.0128049031209714,
-0.00893360751126326));
#34346=CARTESIAN_POINT('Ctrl Pts',(-0.218210920925695,0.0128010511373276,
-0.00893709374166423));
#34347=CARTESIAN_POINT('Ctrl Pts',(-0.218229729974556,0.0127991251455056,
-0.00893883685686471));
#34348=CARTESIAN_POINT('Ctrl Pts',(-0.218241305558444,0.0127972624849013,
-0.00894039412328682));
#34349=CARTESIAN_POINT('Ctrl Pts',(-0.218265649751042,0.0127936761158908,
-0.00894342788658745));
#34350=CARTESIAN_POINT('Ctrl Pts',(-0.218289993402882,0.0127900898265444,
-0.0089464615824991));
#34351=CARTESIAN_POINT('Ctrl Pts',(-0.218327105109004,0.0127847794349534,
-0.00895097104991555));
#34352=CARTESIAN_POINT('Ctrl Pts',(-0.218370317942987,0.0127783336174386,
-0.00895639540594475));
#34353=CARTESIAN_POINT('',(-0.218192328823198,0.00750145352954351,-0.0106389704498565));
#34354=CARTESIAN_POINT('Ctrl Pts',(-0.21837032082272,0.0127783331878846,
-0.00895639576742774));
#34355=CARTESIAN_POINT('Ctrl Pts',(-0.2183439323543,0.012652728887447,-0.00904519967598788));
#34356=CARTESIAN_POINT('Ctrl Pts',(-0.218310137320484,0.012487227094208,
-0.00915553509374897));
#34357=CARTESIAN_POINT('Ctrl Pts',(-0.218273310798793,0.0122983058782609,
-0.00927380836242531));
#34358=CARTESIAN_POINT('Ctrl Pts',(-0.218256491297685,0.0122105314035711,
-0.00932747218006369));
#34359=CARTESIAN_POINT('Ctrl Pts',(-0.218223737672891,0.0120283826649878,
-0.00943442067100643));
#34360=CARTESIAN_POINT('Ctrl Pts',(-0.218190747060741,0.011826330921257,
-0.00954666467228927));
#34361=CARTESIAN_POINT('Ctrl Pts',(-0.218141804676599,0.011482855228234,
-0.00972545966649745));
#34362=CARTESIAN_POINT('Ctrl Pts',(-0.218096132925033,0.0110017408951039,
-0.00994723586626805));
#34363=CARTESIAN_POINT('Ctrl Pts',(-0.21806416032289,0.0102673499403875,
-0.0102164366774509));
#34364=CARTESIAN_POINT('Ctrl Pts',(-0.218060939651304,0.00959120948818163,
-0.0104014795600675));
#34365=CARTESIAN_POINT('Ctrl Pts',(-0.218079867987217,0.00900424255639963,
-0.0105156946566394));
#34366=CARTESIAN_POINT('Ctrl Pts',(-0.218102229010278,0.0086333641300724,
-0.0105668629736167));
#34367=CARTESIAN_POINT('Ctrl Pts',(-0.218118265007893,0.00839965564503378,
-0.0105932637896215));
#34368=CARTESIAN_POINT('Ctrl Pts',(-0.218134302478235,0.00818786903454358,
-0.010611949873552));
#34369=CARTESIAN_POINT('Ctrl Pts',(-0.218143594577732,0.00807273732045675,
-0.0106199877322447));
#34370=CARTESIAN_POINT('Ctrl Pts',(-0.218162363505145,0.007845797986924,
-0.0106330829467462));
#34371=CARTESIAN_POINT('Ctrl Pts',(-0.218179293357208,0.00764982103741828,
-0.0106386516765767));
#34372=CARTESIAN_POINT('Ctrl Pts',(-0.218192328410096,0.00750146607432276,
-0.0106389704552747));
#34373=CARTESIAN_POINT('',(-0.218168819694483,0.00722390949581899,-0.0106342099373409));
#34374=CARTESIAN_POINT('Ctrl Pts',(-0.218168819694483,0.00722390949581899,
-0.0106342099373409));
#34375=CARTESIAN_POINT('Ctrl Pts',(-0.218176520975478,0.00731811245431353,
-0.0106372886165177));
#34376=CARTESIAN_POINT('Ctrl Pts',(-0.218184399517934,0.00741054312879059,
-0.0106388058153284));
#34377=CARTESIAN_POINT('Ctrl Pts',(-0.218192384061994,0.00750144032682139,
-0.0106389717172126));
#34378=CARTESIAN_POINT('',(-0.218067226304046,0.00503956785288683,-0.0102972720892691));
#34379=CARTESIAN_POINT('Ctrl Pts',(-0.218067226304046,0.00503956785288683,
-0.0102972720892691));
#34380=CARTESIAN_POINT('Ctrl Pts',(-0.218067185525726,0.00505809304800469,
-0.0103024611533192));
#34381=CARTESIAN_POINT('Ctrl Pts',(-0.218067177931978,0.00507743493358728,
-0.0103078133779122));
#34382=CARTESIAN_POINT('Ctrl Pts',(-0.218067213740286,0.00509763683519755,
-0.0103133285534128));
#34383=CARTESIAN_POINT('Ctrl Pts',(-0.218067323085079,0.0051593256681294,
-0.0103301697769081));
#34384=CARTESIAN_POINT('Ctrl Pts',(-0.218067839272296,0.00522906185989146,
-0.0103484334274165));
#34385=CARTESIAN_POINT('Ctrl Pts',(-0.218068679804542,0.00529559666923563,
-0.0103650231422464));
#34386=CARTESIAN_POINT('Ctrl Pts',(-0.218070360869035,0.00542866628792398,
-0.0103982025719062));
#34387=CARTESIAN_POINT('Ctrl Pts',(-0.218073329595319,0.00554881996646211,
-0.0104251247091534));
#34388=CARTESIAN_POINT('Ctrl Pts',(-0.218076908899421,0.00566137842301226,
-0.0104483888337291));
#34389=CARTESIAN_POINT('Ctrl Pts',(-0.218078698551471,0.00571765765128734,
-0.0104600208960169));
#34390=CARTESIAN_POINT('Ctrl Pts',(-0.218080642275032,0.00577205172292444,
-0.0104706744407793));
#34391=CARTESIAN_POINT('Ctrl Pts',(-0.218082316864294,0.00581688288328235,
-0.0104791407821068));
#34392=CARTESIAN_POINT('Ctrl Pts',(-0.218083991453555,0.00586171404364027,
-0.0104876071234344));
#34393=CARTESIAN_POINT('Ctrl Pts',(-0.218085392599717,0.00589694463862414,
-0.0104940791762582));
#34394=CARTESIAN_POINT('Ctrl Pts',(-0.218087902510866,0.00595381709000237,
-0.0105039369644601));
#34395=CARTESIAN_POINT('Ctrl Pts',(-0.218090412422016,0.0060106895413806,
-0.010513794752662));
#34396=CARTESIAN_POINT('Ctrl Pts',(-0.218094039354121,0.00608926915687774,
-0.0105266693991204));
#34397=CARTESIAN_POINT('Ctrl Pts',(-0.218097647768551,0.00616140852413473,
-0.0105374851630196));
#34398=CARTESIAN_POINT('Ctrl Pts',(-0.21810125618298,0.00623354789139173,
-0.0105483009269187));
#34399=CARTESIAN_POINT('Ctrl Pts',(-0.218104840027185,0.00629920841664498,
-0.0105573273134242));
#34400=CARTESIAN_POINT('Ctrl Pts',(-0.21810864713066,0.00636524535728989,
-0.0105657273357896));
#34401=CARTESIAN_POINT('Ctrl Pts',(-0.21811626133761,0.0064973192385797,
-0.0105825273805204));
#34402=CARTESIAN_POINT('Ctrl Pts',(-0.218124774963466,0.00663092686543204,
-0.010596538903368));
#34403=CARTESIAN_POINT('Ctrl Pts',(-0.21813377702416,0.00676090874178825,
-0.0106073825650924));
#34404=CARTESIAN_POINT('Ctrl Pts',(-0.218144821541264,0.00692038190082795,
-0.0106206865197607));
#34405=CARTESIAN_POINT('Ctrl Pts',(-0.218156597381377,0.00707438379641082,
-0.0106293941026331));
#34406=CARTESIAN_POINT('Ctrl Pts',(-0.218168819694483,0.00722390949581899,
-0.0106342099373409));
#34407=CARTESIAN_POINT('',(-0.218239365786335,0.00292191358914088,-0.00940513443333053));
#34408=CARTESIAN_POINT('Ctrl Pts',(-0.218239365786335,0.00292191358914088,
-0.00940513443333053));
#34409=CARTESIAN_POINT('Ctrl Pts',(-0.218238792806652,0.0029251222736152,
-0.00940698975198401));
#34410=CARTESIAN_POINT('Ctrl Pts',(-0.218238445755819,0.00292708854324504,
-0.00940812657818748));
#34411=CARTESIAN_POINT('Ctrl Pts',(-0.21823756891017,0.00293204686566356,
-0.0094109852334095));
#34412=CARTESIAN_POINT('Ctrl Pts',(-0.218235815218872,0.0029419635105006,
-0.00941670254385354));
#34413=CARTESIAN_POINT('Ctrl Pts',(-0.218231942760466,0.0029638601938198,
-0.00942928697033889));
#34414=CARTESIAN_POINT('Ctrl Pts',(-0.21822787405026,0.00298719841881205,
-0.00944252702285582));
#34415=CARTESIAN_POINT('Ctrl Pts',(-0.218223805340055,0.00301053664380429,
-0.00945576707537276));
#34416=CARTESIAN_POINT('Ctrl Pts',(-0.218219539291199,0.00303528553849307,
-0.00946971592895734));
#34417=CARTESIAN_POINT('Ctrl Pts',(-0.218213751414185,0.0030701619301952,
-0.0094890281096133));
#34418=CARTESIAN_POINT('Ctrl Pts',(-0.218207963537172,0.00310503832189734,
-0.00950834029026926));
#34419=CARTESIAN_POINT('Ctrl Pts',(-0.218200656891965,0.00315012600620321,
-0.00953286696427101));
#34420=CARTESIAN_POINT('Ctrl Pts',(-0.218195678764406,0.00318147339027357,
-0.00954966258126009));
#34421=CARTESIAN_POINT('Ctrl Pts',(-0.218190700636847,0.00321282077434394,
-0.00956645819824917));
#34422=CARTESIAN_POINT('Ctrl Pts',(-0.218188047637253,0.0032303403141343,
-0.00957568617622878));
#34423=CARTESIAN_POINT('Ctrl Pts',(-0.218185146908979,0.00324971646011447,
-0.00958586023691622));
#34424=CARTESIAN_POINT('Ctrl Pts',(-0.218182246180705,0.00326909260609464,
-0.00959603429760365));
#34425=CARTESIAN_POINT('Ctrl Pts',(-0.218179098878308,0.00329035409754875,
-0.00960709906973049));
#34426=CARTESIAN_POINT('Ctrl Pts',(-0.218176253632057,0.00331011660456465,
-0.00961729005975538));
#34427=CARTESIAN_POINT('Ctrl Pts',(-0.218170563139556,0.00334964161859643,
-0.00963767203980516));
#34428=CARTESIAN_POINT('Ctrl Pts',(-0.218166080234634,0.00338315645788068,
-0.00965458901309295));
#34429=CARTESIAN_POINT('Ctrl Pts',(-0.218162997197411,0.00340695588194977,
-0.00966651052277642));
#34430=CARTESIAN_POINT('Ctrl Pts',(-0.218159914160189,0.00343075530601885,
-0.00967843203245989));
#34431=CARTESIAN_POINT('Ctrl Pts',(-0.218158229993477,0.00344481455338721,
-0.00968540588559376));
#34432=CARTESIAN_POINT('Ctrl Pts',(-0.218155623561165,0.00346732892055049,
-0.0096964817580923));
#34433=CARTESIAN_POINT('Ctrl Pts',(-0.218153017128853,0.00348984328771378,
-0.00970755763059083));
#34434=CARTESIAN_POINT('Ctrl Pts',(-0.218149489538936,0.00352083904218928,
-0.00972268272617012));
#34435=CARTESIAN_POINT('Ctrl Pts',(-0.218145698752299,0.00355603855260194,
-0.00973953220309792));
#34436=CARTESIAN_POINT('Ctrl Pts',(-0.218138117179025,0.00362643757342724,
-0.00977323115695354));
#34437=CARTESIAN_POINT('Ctrl Pts',(-0.218129480285224,0.00371359685156356,
-0.00981394704659143));
#34438=CARTESIAN_POINT('Ctrl Pts',(-0.218120327490645,0.00382045082663618,
-0.0098609864964249));
#34439=CARTESIAN_POINT('Ctrl Pts',(-0.218111430575817,0.0039243175426439,
-0.00990671088967925));
#34440=CARTESIAN_POINT('Ctrl Pts',(-0.218102045208114,0.00404676564641263,
-0.00995845054893569));
#34441=CARTESIAN_POINT('Ctrl Pts',(-0.218093488760285,0.00419254916904724,
-0.0100150756804606));
#34442=CARTESIAN_POINT('Ctrl Pts',(-0.218093242672536,0.00419674197658215,
-0.0100167042477625));
#34443=CARTESIAN_POINT('Ctrl Pts',(-0.218092997270442,0.00420095411548004,
-0.0100183367377336));
#34444=CARTESIAN_POINT('Ctrl Pts',(-0.218092752585342,0.00420518570318234,
-0.0100199731032982));
#34445=CARTESIAN_POINT('Ctrl Pts',(-0.218088376403874,0.00428086744973251,
-0.0100492394242707));
#34446=CARTESIAN_POINT('Ctrl Pts',(-0.218084231623577,0.00436280105608194,
-0.0100796894394523));
#34447=CARTESIAN_POINT('Ctrl Pts',(-0.218080684506125,0.00444451868101746,
-0.0101086817016788));
#34448=CARTESIAN_POINT('Ctrl Pts',(-0.218078910947399,0.00448537749348523,
-0.0101231778327921));
#34449=CARTESIAN_POINT('Ctrl Pts',(-0.218077285414237,0.00452615834643487,
-0.0101373736765752));
#34450=CARTESIAN_POINT('Ctrl Pts',(-0.218075624279617,0.00457624654385498,
-0.0101542910449909));
#34451=CARTESIAN_POINT('Ctrl Pts',(-0.218073963144998,0.0046263347412751,
-0.0101712084134067));
#34452=CARTESIAN_POINT('Ctrl Pts',(-0.218072272056151,0.00468581839975855,
-0.0101905884528484));
#34453=CARTESIAN_POINT('Ctrl Pts',(-0.218071447583993,0.00471612569496449,
-0.0102002835390278));
#34454=CARTESIAN_POINT('Ctrl Pts',(-0.218070623111836,0.00474643299017044,
-0.0102099786252072));
#34455=CARTESIAN_POINT('Ctrl Pts',(-0.218070659325998,0.00474747926921614,
-0.0102102591521145));
#34456=CARTESIAN_POINT('Ctrl Pts',(-0.218070464943007,0.0047579619995227,
-0.0102135587519226));
#34457=CARTESIAN_POINT('Ctrl Pts',(-0.218070270560016,0.00476844472982926,
-0.0102168583517308));
#34458=CARTESIAN_POINT('Ctrl Pts',(-0.218069847248265,0.00478838736452002,
-0.0102231010164984));
#34459=CARTESIAN_POINT('Ctrl Pts',(-0.218069478328105,0.00480837573778782,
-0.0102292653606357));
#34460=CARTESIAN_POINT('Ctrl Pts',(-0.218068740487783,0.00484835248432341,
-0.0102415940489103));
#34461=CARTESIAN_POINT('Ctrl Pts',(-0.218068218029874,0.00488848284454727,
-0.010253708712889));
#34462=CARTESIAN_POINT('Ctrl Pts',(-0.218067808892948,0.00493538064483942,
-0.0102674371328632));
#34463=CARTESIAN_POINT('Ctrl Pts',(-0.218067533740465,0.00496692032110471,
-0.0102766697603835));
#34464=CARTESIAN_POINT('Ctrl Pts',(-0.218067310047023,0.00500152274259813,
-0.0102866230349954));
#34465=CARTESIAN_POINT('Ctrl Pts',(-0.218067226304046,0.00503956785288683,
-0.0102972720892691));
#34466=CARTESIAN_POINT('Ctrl Pts',(-0.218376761434817,0.00221897027385242,
-0.00895460279999876));
#34467=CARTESIAN_POINT('Ctrl Pts',(-0.218355952991769,0.00231749375230912,
-0.00902431860700982));
#34468=CARTESIAN_POINT('Ctrl Pts',(-0.218334517744941,0.00242125175277667,
-0.00909488120513588));
#34469=CARTESIAN_POINT('Ctrl Pts',(-0.218312034443821,0.00253513217699072,
-0.00916849870701569));
#34470=CARTESIAN_POINT('Ctrl Pts',(-0.21830047926189,0.00259366046041081,
-0.00920633405970635));
#34471=CARTESIAN_POINT('Ctrl Pts',(-0.218288648360434,0.00265490126580173,
-0.00924491974098864));
#34472=CARTESIAN_POINT('Ctrl Pts',(-0.218277484656516,0.00271395923175535,
-0.00928118760704619));
#34473=CARTESIAN_POINT('Ctrl Pts',(-0.218271902804557,0.00274348821473217,
-0.00929932154007497));
#34474=CARTESIAN_POINT('Ctrl Pts',(-0.218266487013573,0.00277244827579136,
-0.0093169127990102));
#34475=CARTESIAN_POINT('Ctrl Pts',(-0.218260030845217,0.00280768393378573,
-0.00933797457472041));
#34476=CARTESIAN_POINT('Ctrl Pts',(-0.218253574676861,0.00284291959178011,
-0.00935903635043062));
#34477=CARTESIAN_POINT('Ctrl Pts',(-0.218246081021776,0.00288451657071139,
-0.00938342616520849));
#34478=CARTESIAN_POINT('Ctrl Pts',(-0.218242518753658,0.00290434037807777,
-0.00939494737615413));
#34479=CARTESIAN_POINT('Ctrl Pts',(-0.218240737619598,0.00291425228176096,
-0.00940070798162694));
#34480=CARTESIAN_POINT('Ctrl Pts',(-0.218239938766018,0.00291870490466656,
-0.00940327911467706));
#34481=CARTESIAN_POINT('Ctrl Pts',(-0.218239365786335,0.00292191358914088,
-0.00940513443333053));
#34482=CARTESIAN_POINT('',(-0.216308829828652,0.00249826452155856,-0.00910474619664736));
#34483=CARTESIAN_POINT('',(-0.21509802079524,0.00254314437078809,-0.00910972203361875));
#34484=CARTESIAN_POINT('',(-0.215098016915191,0.0025432095719676,-0.00910961934179909));
#34485=CARTESIAN_POINT('',(-0.21499263029402,0.00750051042987691,-0.0105666547348202));
#34486=CARTESIAN_POINT('Ctrl Pts',(-0.215098014875374,0.00254314350555366,
-0.00910972191547035));
#34487=CARTESIAN_POINT('Ctrl Pts',(-0.215078880714392,0.00266192639885594,
-0.00918587769076132));
#34488=CARTESIAN_POINT('Ctrl Pts',(-0.215054137693622,0.00281927250189698,
-0.00928133661873205));
#34489=CARTESIAN_POINT('Ctrl Pts',(-0.215026681725501,0.00300083501512849,
-0.0093849589510143));
#34490=CARTESIAN_POINT('Ctrl Pts',(-0.215013620542869,0.00308864591147306,
-0.00943387030120433));
#34491=CARTESIAN_POINT('Ctrl Pts',(-0.214989036432337,0.0032621192389327,
-0.00952675263777239));
#34492=CARTESIAN_POINT('Ctrl Pts',(-0.214963579756326,0.00345572023067802,
-0.00962485021407883));
#34493=CARTESIAN_POINT('Ctrl Pts',(-0.214925234692333,0.00377343520887324,
-0.00977659470988523));
#34494=CARTESIAN_POINT('Ctrl Pts',(-0.214881440536056,0.00428400451155548,
-0.00998993632116904));
#34495=CARTESIAN_POINT('Ctrl Pts',(-0.214860207112644,0.0049215028701946,
-0.0102002226568554));
#34496=CARTESIAN_POINT('Ctrl Pts',(-0.214864229236519,0.0054097933709423,
-0.0103262195562019));
#34497=CARTESIAN_POINT('Ctrl Pts',(-0.214877231587741,0.00579919116479696,
-0.0104053314765542));
#34498=CARTESIAN_POINT('Ctrl Pts',(-0.2148871035798,0.00601821428182061,
-0.0104437537652626));
#34499=CARTESIAN_POINT('Ctrl Pts',(-0.214897480943101,0.00621158765416454,
-0.010473381553683));
#34500=CARTESIAN_POINT('Ctrl Pts',(-0.214903550546303,0.00631154295636838,
-0.0104869694861788));
#34501=CARTESIAN_POINT('Ctrl Pts',(-0.214915416994173,0.00649705465937709,
-0.01051040061382));
#34502=CARTESIAN_POINT('Ctrl Pts',(-0.214939982118418,0.00684552155670783,
-0.0105460281812664));
#34503=CARTESIAN_POINT('Ctrl Pts',(-0.21496945372088,0.00722074018422242,
-0.0105661467154913));
#34504=CARTESIAN_POINT('Ctrl Pts',(-0.21499263029402,0.00750051042987691,
-0.0105666547348202));
#34505=CARTESIAN_POINT('',(-0.215095414441432,0.0124591460413101,-0.00910819331956975));
#34506=CARTESIAN_POINT('Ctrl Pts',(-0.214992630415778,0.00750051189965118,
-0.010566654737489));
#34507=CARTESIAN_POINT('Ctrl Pts',(-0.214969342612911,0.00778055055796294,
-0.0105661125628055));
#34508=CARTESIAN_POINT('Ctrl Pts',(-0.214939714956889,0.00815615289366023,
-0.0105459126315921));
#34509=CARTESIAN_POINT('Ctrl Pts',(-0.214914988096678,0.00850509262545842,
-0.0105101549770463));
#34510=CARTESIAN_POINT('Ctrl Pts',(-0.214903033354419,0.00869081285498103,
-0.0104866497375707));
#34511=CARTESIAN_POINT('Ctrl Pts',(-0.214896904227771,0.00879108378126653,
-0.0104729875780705));
#34512=CARTESIAN_POINT('Ctrl Pts',(-0.214886455051281,0.00898415541890412,
-0.0104433475154732));
#34513=CARTESIAN_POINT('Ctrl Pts',(-0.214876476790143,0.00920293166221906,
-0.0104049125080223));
#34514=CARTESIAN_POINT('Ctrl Pts',(-0.214863260859888,0.00959187816631272,
-0.0103257769396539));
#34515=CARTESIAN_POINT('Ctrl Pts',(-0.214858821715445,0.0100779610425055,
-0.0102003615124657));
#34516=CARTESIAN_POINT('Ctrl Pts',(-0.214879534188101,0.0107186135739898,
-0.00998899566147673));
#34517=CARTESIAN_POINT('Ctrl Pts',(-0.214923072812692,0.0112295676181993,
-0.00977519129368386));
#34518=CARTESIAN_POINT('Ctrl Pts',(-0.214961205141803,0.0115466288585745,
-0.0096236389989249));
#34519=CARTESIAN_POINT('Ctrl Pts',(-0.214986555872579,0.0117399447159114,
-0.00952561889921954));
#34520=CARTESIAN_POINT('Ctrl Pts',(-0.215011037359278,0.0119130572004991,
-0.00943287805535147));
#34521=CARTESIAN_POINT('Ctrl Pts',(-0.215024090110732,0.0120009612740028,
-0.0093838919409602));
#34522=CARTESIAN_POINT('Ctrl Pts',(-0.215051519974409,0.0121826213746208,
-0.00928015774996104));
#34523=CARTESIAN_POINT('Ctrl Pts',(-0.215076266198542,0.0123401831812057,
-0.00918451547138759));
#34524=CARTESIAN_POINT('Ctrl Pts',(-0.215095408231139,0.0124591472231019,
-0.00910819364212774));
#34525=CARTESIAN_POINT('',(-0.216305506198624,0.0125054790081327,-0.00910194677041158));
#34526=CARTESIAN_POINT('',(-0.216305506198628,0.0125054790081358,-0.00910194677040962));
#34527=CARTESIAN_POINT('',(-0.21606291203367,0.0101163502415278,-0.0102080466013605));
#34528=CARTESIAN_POINT('Ctrl Pts',(-0.216305504030195,0.0125055507042171,
-0.00910205625925057));
#34529=CARTESIAN_POINT('Ctrl Pts',(-0.216285573012244,0.0123847852099932,
-0.00918076999389213));
#34530=CARTESIAN_POINT('Ctrl Pts',(-0.216268459633762,0.0122785427758774,
-0.00924611596648593));
#34531=CARTESIAN_POINT('Ctrl Pts',(-0.216253300799397,0.0121823096002432,
-0.00930328007396658));
#34532=CARTESIAN_POINT('Ctrl Pts',(-0.216245721382214,0.0121341930124262,
-0.0093318621277069));
#34533=CARTESIAN_POINT('Ctrl Pts',(-0.21623863170164,0.0120885445419686,
-0.00935834388998212));
#34534=CARTESIAN_POINT('Ctrl Pts',(-0.216232891551287,0.012051317695906,
-0.00937963114515802));
#34535=CARTESIAN_POINT('Ctrl Pts',(-0.216227151400934,0.0120140908498435,
-0.00940091840033392));
#34536=CARTESIAN_POINT('Ctrl Pts',(-0.216222758129353,0.0119853611814783,
-0.00941714121196255));
#34537=CARTESIAN_POINT('Ctrl Pts',(-0.216216277214704,0.0119417188391278,
-0.00944131001650295));
#34538=CARTESIAN_POINT('Ctrl Pts',(-0.216209796300054,0.0118980764967773,
-0.00946547882104336));
#34539=CARTESIAN_POINT('Ctrl Pts',(-0.216201232533199,0.0118393910761824,
-0.00949736036638175));
#34540=CARTESIAN_POINT('Ctrl Pts',(-0.216193646182268,0.0117856311521386,
-0.00952578762890845));
#34541=CARTESIAN_POINT('Ctrl Pts',(-0.216186059831338,0.0117318712280949,
-0.00955421489143515));
#34542=CARTESIAN_POINT('Ctrl Pts',(-0.216179447590711,0.0116831194740222,
-0.00957934676861737));
#34543=CARTESIAN_POINT('Ctrl Pts',(-0.216173143906361,0.0116354147837649,
-0.00960345893009553));
#34544=CARTESIAN_POINT('Ctrl Pts',(-0.216160536537661,0.0115400054032504,
-0.00965168325305186));
#34545=CARTESIAN_POINT('Ctrl Pts',(-0.216149163753679,0.011448784674882,
-0.0096958139505624));
#34546=CARTESIAN_POINT('Ctrl Pts',(-0.216138525624132,0.0113536345020631,
-0.0097399040558179));
#34547=CARTESIAN_POINT('Ctrl Pts',(-0.216119015322928,0.0111791293390033,
-0.00982076519121042));
#34548=CARTESIAN_POINT('Ctrl Pts',(-0.216101987621509,0.0109911688732712,
-0.00990098102958284));
#34549=CARTESIAN_POINT('Ctrl Pts',(-0.216089376752195,0.0107988963082568,
-0.00997514789234148));
#34550=CARTESIAN_POINT('Ctrl Pts',(-0.216088235290362,0.0107814929247929,
-0.00998186104121329));
#34551=CARTESIAN_POINT('Ctrl Pts',(-0.216087130014783,0.010764054992567,
-0.0099885262252447));
#34552=CARTESIAN_POINT('Ctrl Pts',(-0.216086062359817,0.0107465897968397,
-0.00999514054140734));
#34553=CARTESIAN_POINT('Ctrl Pts',(-0.216073208630083,0.0105363225168689,
-0.0100747717284893));
#34554=CARTESIAN_POINT('Ctrl Pts',(-0.216065806914254,0.0103219438699067,
-0.0101467674241031));
#34555=CARTESIAN_POINT('Ctrl Pts',(-0.21606291203367,0.0101163502415278,
-0.0102080466013605));
#34556=CARTESIAN_POINT('',(-0.216192971496085,0.00750084397878958,-0.0105937835194403));
#34557=CARTESIAN_POINT('Ctrl Pts',(-0.216062905705723,0.0101159003354215,
-0.0102081806868227));
#34558=CARTESIAN_POINT('Ctrl Pts',(-0.216060015292875,0.00991016956652308,
-0.0102694889169385));
#34559=CARTESIAN_POINT('Ctrl Pts',(-0.216061617126363,0.00971354178683412,
-0.0103209970309253));
#34560=CARTESIAN_POINT('Ctrl Pts',(-0.21606719175661,0.00949795270790532,
-0.0103693828238878));
#34561=CARTESIAN_POINT('Ctrl Pts',(-0.216069979071733,0.00939015816844091,
-0.0103935757203691));
#34562=CARTESIAN_POINT('Ctrl Pts',(-0.216073764939323,0.00927757116026392,
-0.0104167477640333));
#34563=CARTESIAN_POINT('Ctrl Pts',(-0.21607838814934,0.0091661349877902,
-0.0104375189787289));
#34564=CARTESIAN_POINT('Ctrl Pts',(-0.216080699754349,0.00911041690155334,
-0.0104479045860768));
#34565=CARTESIAN_POINT('Ctrl Pts',(-0.216083219538258,0.00905499630344108,
-0.0104577417300695));
#34566=CARTESIAN_POINT('Ctrl Pts',(-0.216086249687527,0.00899457404370174,
-0.0104678359117436));
#34567=CARTESIAN_POINT('Ctrl Pts',(-0.216089279836797,0.0089341517839624,
-0.0104779300934177));
#34568=CARTESIAN_POINT('Ctrl Pts',(-0.216092824138265,0.00886869900919264,
-0.010488112205039));
#34569=CARTESIAN_POINT('Ctrl Pts',(-0.216095620120263,0.00881928313990659,
-0.0104953976695696));
#34570=CARTESIAN_POINT('Ctrl Pts',(-0.216098416102261,0.00876986727062052,
-0.0105026831341002));
#34571=CARTESIAN_POINT('Ctrl Pts',(-0.21610045846058,0.00873652214479988,
-0.0105073081857298));
#34572=CARTESIAN_POINT('Ctrl Pts',(-0.216102985135538,0.00869646623545131,
-0.0105126682511252));
#34573=CARTESIAN_POINT('Ctrl Pts',(-0.216105511810496,0.00865641032610275,
-0.0105180283165205));
#34574=CARTESIAN_POINT('Ctrl Pts',(-0.21610852564855,0.0086096276180213,
-0.0105239968074858));
#34575=CARTESIAN_POINT('Ctrl Pts',(-0.216111722711867,0.00856168836907106,
-0.0105296950506111));
#34576=CARTESIAN_POINT('Ctrl Pts',(-0.216118116838502,0.00846580987117058,
-0.0105410915368618));
#34577=CARTESIAN_POINT('Ctrl Pts',(-0.216125240347082,0.00836532088670505,
-0.010551563202669));
#34578=CARTESIAN_POINT('Ctrl Pts',(-0.216133315547689,0.00825611658081511,
-0.0105608620487624));
#34579=CARTESIAN_POINT('Ctrl Pts',(-0.216149465933751,0.00803770817395129,
-0.0105794597235006));
#34580=CARTESIAN_POINT('Ctrl Pts',(-0.21616942628362,0.00778443696992211,
-0.0105932247541572));
#34581=CARTESIAN_POINT('Ctrl Pts',(-0.216192971885712,0.00750084401094905,
-0.0105937834231419));
#34582=CARTESIAN_POINT('',(-0.216064562234792,0.00488811599144484,-0.0102094142070321));
#34583=CARTESIAN_POINT('Ctrl Pts',(-0.216192971951985,0.00750084321272765,
-0.0105937834247143));
#34584=CARTESIAN_POINT('Ctrl Pts',(-0.216169508654091,0.00721699231932673,
-0.0105932796528161));
#34585=CARTESIAN_POINT('Ctrl Pts',(-0.216149636727297,0.0069635594796243,
-0.010579541065668));
#34586=CARTESIAN_POINT('Ctrl Pts',(-0.216133576495944,0.00674505389894682,
-0.0105609655730863));
#34587=CARTESIAN_POINT('Ctrl Pts',(-0.216125546380267,0.00663580110860809,
-0.0105516778267954));
#34588=CARTESIAN_POINT('Ctrl Pts',(-0.216118468404311,0.00653527978127621,
-0.0105412154642067));
#34589=CARTESIAN_POINT('Ctrl Pts',(-0.216112124596152,0.00643941830546403,
-0.0105298339080441));
#34590=CARTESIAN_POINT('Ctrl Pts',(-0.216108952692073,0.00639148756755795,
-0.0105241431299627));
#34591=CARTESIAN_POINT('Ctrl Pts',(-0.216105965202961,0.00634472567739711,
-0.0105181838109217));
#34592=CARTESIAN_POINT('Ctrl Pts',(-0.216103460103315,0.00630465700703719,
-0.0105128275687491));
#34593=CARTESIAN_POINT('Ctrl Pts',(-0.216100955003668,0.00626458833667726,
-0.0105074713265765));
#34594=CARTESIAN_POINT('Ctrl Pts',(-0.216098929471675,0.00623119702191735,
-0.0105028436523896));
#34595=CARTESIAN_POINT('Ctrl Pts',(-0.216096169915181,0.00618188883829889,
-0.0104955812314442));
#34596=CARTESIAN_POINT('Ctrl Pts',(-0.216093410358688,0.00613258065468043,
-0.0104883188104988));
#34597=CARTESIAN_POINT('Ctrl Pts',(-0.216089922022156,0.00606738903619435,
-0.0104781880715125));
#34598=CARTESIAN_POINT('Ctrl Pts',(-0.216086942406758,0.00600717401362571,
-0.0104681413248275));
#34599=CARTESIAN_POINT('Ctrl Pts',(-0.216083962791361,0.00594695899105708,
-0.0104580945781425));
#34600=CARTESIAN_POINT('Ctrl Pts',(-0.216081488159746,0.00589169212150471,
-0.010448298718238));
#34601=CARTESIAN_POINT('Ctrl Pts',(-0.216079222483585,0.00583612546404543,
-0.0104379565789868));
#34602=CARTESIAN_POINT('Ctrl Pts',(-0.216074691131264,0.00572499214912688,
-0.0104172723004846));
#34603=CARTESIAN_POINT('Ctrl Pts',(-0.21607100017286,0.00561269828959701,
-0.0103941983821629));
#34604=CARTESIAN_POINT('Ctrl Pts',(-0.216068305392988,0.00550514230539665,
-0.01037009988483));
#34605=CARTESIAN_POINT('Ctrl Pts',(-0.216062915833244,0.00529003033699593,
-0.0103219028901643));
#34606=CARTESIAN_POINT('Ctrl Pts',(-0.21606148974563,0.00509366268594511,
-0.010270561045398));
#34607=CARTESIAN_POINT('Ctrl Pts',(-0.216064562234792,0.00488811599144484,
-0.0102094142070321));
#34608=CARTESIAN_POINT('Ctrl Pts',(-0.216064562234792,0.00488811599144484,
-0.0102094142070321));
#34609=CARTESIAN_POINT('Ctrl Pts',(-0.216067634723955,0.00468256929694457,
-0.0101482673686662));
#34610=CARTESIAN_POINT('Ctrl Pts',(-0.21607522582377,0.00446813446215115,
-0.0100764011159303));
#34611=CARTESIAN_POINT('Ctrl Pts',(-0.216088338924692,0.00425716728514312,
-0.00999661661287887));
#34612=CARTESIAN_POINT('Ctrl Pts',(-0.216089502570561,0.00423844623011241,
-0.00998953660122299));
#34613=CARTESIAN_POINT('Ctrl Pts',(-0.216090709717795,0.00421975125104769,
-0.00998239617590539));
#34614=CARTESIAN_POINT('Ctrl Pts',(-0.21609195844297,0.00420109267159996,
-0.00997519932710212));
#34615=CARTESIAN_POINT('Ctrl Pts',(-0.216104781575639,0.00400948811007565,
-0.0099012950374873));
#34616=CARTESIAN_POINT('Ctrl Pts',(-0.216121989182533,0.00382182884714497,
-0.00982121910009571));
#34617=CARTESIAN_POINT('Ctrl Pts',(-0.216141498420156,0.00364853401298664,
-0.00974097652987249));
#34618=CARTESIAN_POINT('Ctrl Pts',(-0.216152202950225,0.00355344881288889,
-0.00969694820737177));
#34619=CARTESIAN_POINT('Ctrl Pts',(-0.216163596637211,0.00346261072515542,
-0.00965303427445999));
#34620=CARTESIAN_POINT('Ctrl Pts',(-0.216176231034628,0.00336745049549093,
-0.00960497891364581));
#34621=CARTESIAN_POINT('Ctrl Pts',(-0.216182548233336,0.00331987038065869,
-0.00958095123323872));
#34622=CARTESIAN_POINT('Ctrl Pts',(-0.21618917555074,0.0032712106596776,
-0.00955589038338166));
#34623=CARTESIAN_POINT('Ctrl Pts',(-0.216196774500355,0.0032175566238911,
-0.00952754662918728));
#34624=CARTESIAN_POINT('Ctrl Pts',(-0.21620437344997,0.0031639025881046,
-0.0094992028749929));
#34625=CARTESIAN_POINT('Ctrl Pts',(-0.21621294731804,0.00310533630168092,
-0.00946741828469016));
#34626=CARTESIAN_POINT('Ctrl Pts',(-0.216219436071743,0.00306177318974593,
-0.00944331847681517));
#34627=CARTESIAN_POINT('Ctrl Pts',(-0.216225924825445,0.00301821007781095,
-0.00941921866894019));
#34628=CARTESIAN_POINT('Ctrl Pts',(-0.216230323693065,0.00298952042971264,
-0.00940303591356076));
#34629=CARTESIAN_POINT('Ctrl Pts',(-0.216236072810317,0.00295233499613605,
-0.00938179523158231));
#34630=CARTESIAN_POINT('Ctrl Pts',(-0.21624182192757,0.00291514956255945,
-0.00936055454960386));
#34631=CARTESIAN_POINT('Ctrl Pts',(-0.216248923937414,0.00286954355307472,
-0.009334126324145));
#34632=CARTESIAN_POINT('Ctrl Pts',(-0.216256517647776,0.00282146039342472,
-0.00930559553315848));
#34633=CARTESIAN_POINT('Ctrl Pts',(-0.216271705068501,0.00272529407412471,
-0.00924853395118545));
#34634=CARTESIAN_POINT('Ctrl Pts',(-0.216288854896236,0.00261908279258283,
-0.0091832809841745));
#34635=CARTESIAN_POINT('Ctrl Pts',(-0.216308831619352,0.00249832230384034,
-0.0091046579272641));
#34636=CARTESIAN_POINT('',(-0.191002128727803,0.00750279694962982,-0.0100254048439417));
#34637=CARTESIAN_POINT('',(-0.190954131521021,0.0114757689203866,-0.00915712253688136));
#34638=CARTESIAN_POINT('Ctrl Pts',(-0.190954094375179,0.0114755956741647,
-0.00915648079316597));
#34639=CARTESIAN_POINT('Ctrl Pts',(-0.190949712020098,0.0114114603137452,
-0.00918577312088179));
#34640=CARTESIAN_POINT('Ctrl Pts',(-0.190945071320235,0.0113437322707912,
-0.00921585170663403));
#34641=CARTESIAN_POINT('Ctrl Pts',(-0.190940278164648,0.0112720433793392,
-0.00924659321808342));
#34642=CARTESIAN_POINT('Ctrl Pts',(-0.190935484712584,0.0112003500536294,
-0.00927733663102393));
#34643=CARTESIAN_POINT('Ctrl Pts',(-0.190930538969924,0.0111246908651552,
-0.00930873403932449));
#34644=CARTESIAN_POINT('Ctrl Pts',(-0.190925612592709,0.0110457932672867,
-0.00934019431223972));
#34645=CARTESIAN_POINT('Ctrl Pts',(-0.190920686215494,0.0109668956694181,
-0.00937165458515496));
#34646=CARTESIAN_POINT('Ctrl Pts',(-0.190915778457101,0.0108847753427232,
-0.00940321350242323));
#34647=CARTESIAN_POINT('Ctrl Pts',(-0.190910892877424,0.0107962805502497,
-0.00943565448019979));
#34648=CARTESIAN_POINT('Ctrl Pts',(-0.190908982581279,0.0107616784616149,
-0.00944833913154536));
#34649=CARTESIAN_POINT('Ctrl Pts',(-0.19090707603451,0.0107260969951283,
-0.00946114643072369));
#34650=CARTESIAN_POINT('Ctrl Pts',(-0.190905267900651,0.0106913983121456,
-0.00947340659224363));
#34651=CARTESIAN_POINT('Ctrl Pts',(-0.190904763884623,0.0106817260789378,
-0.0094768241035493));
#34652=CARTESIAN_POINT('Ctrl Pts',(-0.190904267515394,0.0106721226257211,
-0.00948019962700674));
#34653=CARTESIAN_POINT('Ctrl Pts',(-0.190903780843293,0.0106626287092986,
-0.00948351987320058));
#34654=CARTESIAN_POINT('Ctrl Pts',(-0.190902664550575,0.0106408522611478,
-0.00949113561004409));
#34655=CARTESIAN_POINT('Ctrl Pts',(-0.190901598866219,0.010619657350123,
-0.0094984750067754));
#34656=CARTESIAN_POINT('Ctrl Pts',(-0.190900336275497,0.0105935509108808,
-0.00950738083319582));
#34657=CARTESIAN_POINT('Ctrl Pts',(-0.190899073684775,0.0105674444716387,
-0.00951628665961624));
#34658=CARTESIAN_POINT('Ctrl Pts',(-0.190897615764644,0.0105364013707763,
-0.00952668559938698));
#34659=CARTESIAN_POINT('Ctrl Pts',(-0.190896985542716,0.0105229623294542,
-0.00953115285039524));
#34660=CARTESIAN_POINT('Ctrl Pts',(-0.190896670431751,0.0105162428087932,
-0.00953338647589937));
#34661=CARTESIAN_POINT('Ctrl Pts',(-0.190896561953082,0.0105139287668234,
-0.00953415071739028));
#34662=CARTESIAN_POINT('Ctrl Pts',(-0.190896511796388,0.0105128545877792,
-0.00953450644811207));
#34663=CARTESIAN_POINT('Ctrl Pts',(-0.190896486718041,0.0105123174982571,
-0.00953468431347296));
#34664=CARTESIAN_POINT('Ctrl Pts',(-0.190896476230896,0.010512090212176,
-0.00953475955545459));
#34665=CARTESIAN_POINT('Ctrl Pts',(-0.19089646182634,0.0105117765703442,
-0.00953486338619688));
#34666=CARTESIAN_POINT('Ctrl Pts',(-0.190896447421783,0.0105114629285123,
-0.00953496721693918));
#34667=CARTESIAN_POINT('Ctrl Pts',(-0.190896429099489,0.0105110629359991,
-0.00953509965162892));
#34668=CARTESIAN_POINT('Ctrl Pts',(-0.19089638835623,0.0105101803497181,
-0.00953539165248889));
#34669=CARTESIAN_POINT('Ctrl Pts',(-0.190896225383196,0.0105066500045945,
-0.00953655965592877));
#34670=CARTESIAN_POINT('Ctrl Pts',(-0.190895703714802,0.0104953975208178,
-0.00954027885553927));
#34671=CARTESIAN_POINT('Ctrl Pts',(-0.190895127071901,0.0104827302132629,
-0.00954442716706281));
#34672=CARTESIAN_POINT('Ctrl Pts',(-0.190893973786097,0.0104573955981532,
-0.00955272379010988));
#34673=CARTESIAN_POINT('Ctrl Pts',(-0.19089259953884,0.0104264180483005,
-0.00956278615109603));
#34674=CARTESIAN_POINT('Ctrl Pts',(-0.190890902985786,0.0103836168892928,
-0.00957629011243121));
#34675=CARTESIAN_POINT('Ctrl Pts',(-0.190889206432731,0.010340815730285,
-0.0095897940737664));
#34676=CARTESIAN_POINT('Ctrl Pts',(-0.190887188717151,0.0102861734770876,
-0.00960668668092587));
#34677=CARTESIAN_POINT('Ctrl Pts',(-0.190885238302781,0.0102249868586566,
-0.00962483435560046));
#34678=CARTESIAN_POINT('Ctrl Pts',(-0.190884263095595,0.0101943935494411,
-0.00963390819293776));
#34679=CARTESIAN_POINT('Ctrl Pts',(-0.190883304145586,0.0101621723310017,
-0.00964332198835475));
#34680=CARTESIAN_POINT('Ctrl Pts',(-0.190882305478128,0.010123072861922,
-0.00965445185984557));
#34681=CARTESIAN_POINT('Ctrl Pts',(-0.190881306810671,0.0100839733928422,
-0.0096655817313364));
#34682=CARTESIAN_POINT('Ctrl Pts',(-0.190880270863819,0.0100379635616817,
-0.00967831595867959));
#34683=CARTESIAN_POINT('Ctrl Pts',(-0.190879609294718,0.0100059172322142,
-0.00968700170894241));
#34684=CARTESIAN_POINT('Ctrl Pts',(-0.190878947725618,0.00997387090274672,
-0.00969568745920523));
#34685=CARTESIAN_POINT('Ctrl Pts',(-0.190878657565483,0.00995582424085349,
-0.00970046013451214));
#34686=CARTESIAN_POINT('Ctrl Pts',(-0.190878343369803,0.00993486250300072,
-0.00970597129447378));
#34687=CARTESIAN_POINT('Ctrl Pts',(-0.190878029174123,0.00991390076514795,
-0.00971148245443542));
#34688=CARTESIAN_POINT('Ctrl Pts',(-0.190877692134822,0.00989001008289119,
-0.00971767787286489));
#34689=CARTESIAN_POINT('Ctrl Pts',(-0.190877422907681,0.0098672072748013,
-0.00972349682048002));
#34690=CARTESIAN_POINT('Ctrl Pts',(-0.1908768844534,0.00982160165862154,
-0.00973513471571027));
#34691=CARTESIAN_POINT('Ctrl Pts',(-0.190876616187465,0.00978035869652348,
-0.00974531472603288));
#34692=CARTESIAN_POINT('Ctrl Pts',(-0.190876473111491,0.00974219455184456,
-0.00975451522161448));
#34693=CARTESIAN_POINT('Ctrl Pts',(-0.190876330035517,0.00970403040716564,
-0.00976371571719607));
#34694=CARTESIAN_POINT('Ctrl Pts',(-0.190876311814032,0.00966894964395492,
-0.00977195208813503));
#34695=CARTESIAN_POINT('Ctrl Pts',(-0.190876488385096,0.00963105439853278,
-0.00978061835509751));
#34696=CARTESIAN_POINT('Ctrl Pts',(-0.190876664956159,0.00959315915311064,
-0.00978928462205999));
#34697=CARTESIAN_POINT('Ctrl Pts',(-0.19087703863711,0.00955242519301168,
-0.00979827588427239));
#34698=CARTESIAN_POINT('Ctrl Pts',(-0.190877227802085,0.00953392878073028,
-0.00980230657795196));
#34699=CARTESIAN_POINT('Ctrl Pts',(-0.190877322384573,0.00952468057458957,
-0.00980432192479174));
#34700=CARTESIAN_POINT('Ctrl Pts',(-0.190877370417995,0.00952099580690186,
-0.00980511608364548));
#34701=CARTESIAN_POINT('Ctrl Pts',(-0.190877416245437,0.00951868580370159,
-0.00980561603274182));
#34702=CARTESIAN_POINT('Ctrl Pts',(-0.190877462072879,0.00951637580050133,
-0.00980611598183816));
#34703=CARTESIAN_POINT('Ctrl Pts',(-0.190877505748922,0.009515440046279,
-0.00980631926023749));
#34704=CARTESIAN_POINT('Ctrl Pts',(-0.190877592138407,0.00951168488289209,
-0.00980712931189838));
#34705=CARTESIAN_POINT('Ctrl Pts',(-0.190877764917375,0.00950417455611826,
-0.00980874941522017));
#34706=CARTESIAN_POINT('Ctrl Pts',(-0.190878108686614,0.00948538517546544,
-0.00981279043480945));
#34707=CARTESIAN_POINT('Ctrl Pts',(-0.190878570724653,0.00946280542795435,
-0.00981753707052625));
#34708=CARTESIAN_POINT('Ctrl Pts',(-0.190879494800731,0.00941764593293216,
-0.00982703034195985));
#34709=CARTESIAN_POINT('Ctrl Pts',(-0.190880889082616,0.00935735369003375,
-0.00983947571397337));
#34710=CARTESIAN_POINT('Ctrl Pts',(-0.190883526254305,0.00927378471309401,
-0.00985531897787881));
#34711=CARTESIAN_POINT('Ctrl Pts',(-0.190886163425994,0.00919021573615428,
-0.00987116224178425));
#34712=CARTESIAN_POINT('Ctrl Pts',(-0.190890046919921,0.00908333562718222,
-0.0098902484430308));
#34713=CARTESIAN_POINT('Ctrl Pts',(-0.19089556723871,0.00896203269271428,
-0.00990916826768047));
#34714=CARTESIAN_POINT('Ctrl Pts',(-0.190898327398105,0.00890138122548031,
-0.00991862818000531));
#34715=CARTESIAN_POINT('Ctrl Pts',(-0.190901494806612,0.00883714055904416,
-0.00992813433623493));
#34716=CARTESIAN_POINT('Ctrl Pts',(-0.190905913041937,0.00875970557271916,
-0.0099385485861674));
#34717=CARTESIAN_POINT('Ctrl Pts',(-0.190910331277262,0.00868227058639415,
-0.00994896283609988));
#34718=CARTESIAN_POINT('Ctrl Pts',(-0.190916009238766,0.00859158540031464,
-0.0099598880920389));
#34719=CARTESIAN_POINT('Ctrl Pts',(-0.190920299492141,0.00852624126001904,
-0.00996706295173374));
#34720=CARTESIAN_POINT('Ctrl Pts',(-0.190924589745517,0.00846089711972344,
-0.00997423781142858));
#34721=CARTESIAN_POINT('Ctrl Pts',(-0.190927481335499,0.00842094452761956,
-0.0099781492331332));
#34722=CARTESIAN_POINT('Ctrl Pts',(-0.190930754362073,0.00837603777468225,
-0.00998237237824975));
#34723=CARTESIAN_POINT('Ctrl Pts',(-0.190934027388647,0.00833113102174495,
-0.0099865955233663));
#34724=CARTESIAN_POINT('Ctrl Pts',(-0.190937686315205,0.00828125394742464,
-0.00999093235948039));
#34725=CARTESIAN_POINT('Ctrl Pts',(-0.190941295904069,0.00823342278523267,
-0.00999471241801912));
#34726=CARTESIAN_POINT('Ctrl Pts',(-0.190948515081796,0.00813776046084873,
-0.0100022725350966));
#34727=CARTESIAN_POINT('Ctrl Pts',(-0.190955532508425,0.00805029181322841,
-0.010007800356196));
#34728=CARTESIAN_POINT('Ctrl Pts',(-0.190962490680233,0.00796595757437065,
-0.0100121008424296));
#34729=CARTESIAN_POINT('Ctrl Pts',(-0.19097640702385,0.00779728909665514,
-0.010020701814897));
#34730=CARTESIAN_POINT('Ctrl Pts',(-0.190990092174909,0.00764116175118779,
-0.0100241361536859));
#34731=CARTESIAN_POINT('Ctrl Pts',(-0.191002150316979,0.00750280017557725,
-0.0100244496327049));
#34732=CARTESIAN_POINT('',(-0.191550785002591,0.0118950229056552,-0.00896386114240554));
#34733=CARTESIAN_POINT('Ctrl Pts',(-0.190954112929703,0.0114756574972142,
-0.00915645285326651));
#34734=CARTESIAN_POINT('Ctrl Pts',(-0.190982008539415,0.0115054322583542,
-0.00914338889688701));
#34735=CARTESIAN_POINT('Ctrl Pts',(-0.19101287342955,0.0115380979044843,
-0.00912884832062592));
#34736=CARTESIAN_POINT('Ctrl Pts',(-0.191106704839325,0.0116251376084165,
-0.00908978613440817));
#34737=CARTESIAN_POINT('Ctrl Pts',(-0.191229718411826,0.0117176478910505,
-0.00904729586658412));
#34738=CARTESIAN_POINT('Ctrl Pts',(-0.191370919388666,0.0118051770272004,
-0.00900648410289972));
#34739=CARTESIAN_POINT('Ctrl Pts',(-0.191495260460881,0.0118685913453507,
-0.00897644371887849));
#34740=CARTESIAN_POINT('Ctrl Pts',(-0.191550246290606,0.0118947665274591,
-0.00896398319195776));
#34741=CARTESIAN_POINT('',(-0.19224419201362,0.0121632767044805,-0.00883255225498704));
#34742=CARTESIAN_POINT('Ctrl Pts',(-0.191550785002591,0.0118950229056552,
-0.00896386114240554));
#34743=CARTESIAN_POINT('Ctrl Pts',(-0.191605544537764,0.0119210766204984,
-0.00895145795873606));
#34744=CARTESIAN_POINT('Ctrl Pts',(-0.191677122179383,0.0119519839958818,
-0.00893663396839678));
#34745=CARTESIAN_POINT('Ctrl Pts',(-0.19179224763391,0.0119993353150033,
-0.00891377444744784));
#34746=CARTESIAN_POINT('Ctrl Pts',(-0.191909096678037,0.012044435087274,
-0.00889178266758456));
#34747=CARTESIAN_POINT('Ctrl Pts',(-0.191939931439879,0.0120558519308887,
-0.00888617858607348));
#34748=CARTESIAN_POINT('Ctrl Pts',(-0.19204879387273,0.0120964762074764,
-0.00886617854625054));
#34749=CARTESIAN_POINT('Ctrl Pts',(-0.192155333347995,0.0121356773845727,
-0.00884660375394572));
#34750=CARTESIAN_POINT('Ctrl Pts',(-0.192242639246286,0.0121676311322629,
-0.00883037490798918));
#34751=CARTESIAN_POINT('',(-0.192083217793351,0.0103603962460601,-0.00960945776125992));
#34752=CARTESIAN_POINT('Ctrl Pts',(-0.192083217793351,0.0103603962460601,
-0.00960945776125992));
#34753=CARTESIAN_POINT('Ctrl Pts',(-0.192085199140223,0.0104074107317101,
-0.00959475205438907));
#34754=CARTESIAN_POINT('Ctrl Pts',(-0.192087605796192,0.0104586710651692,
-0.00957826631006171));
#34755=CARTESIAN_POINT('Ctrl Pts',(-0.192090621658018,0.0105149888983772,
-0.00955956027685326));
#34756=CARTESIAN_POINT('Ctrl Pts',(-0.19209365489289,0.0105716311537188,
-0.00954074648645924));
#34757=CARTESIAN_POINT('Ctrl Pts',(-0.192097307609679,0.0106333734291636,
-0.00951962630166627));
#34758=CARTESIAN_POINT('Ctrl Pts',(-0.192101334370423,0.0106965037041797,
-0.00949723574375678));
#34759=CARTESIAN_POINT('Ctrl Pts',(-0.192105873419757,0.0107676654768694,
-0.0094719966363405));
#34760=CARTESIAN_POINT('Ctrl Pts',(-0.19211088773952,0.0108405851111344,
-0.00944513150529008));
#34761=CARTESIAN_POINT('Ctrl Pts',(-0.192116025794393,0.0109101028658402,
-0.0094185854425774));
#34762=CARTESIAN_POINT('Ctrl Pts',(-0.192135418226145,0.0111724819853732,
-0.0093183933033018));
#34763=CARTESIAN_POINT('Ctrl Pts',(-0.192156505092465,0.0113871237995003,
-0.00922445471737479));
#34764=CARTESIAN_POINT('Ctrl Pts',(-0.192178577024194,0.0115925865308087,
-0.00912711081785286));
#34765=CARTESIAN_POINT('Ctrl Pts',(-0.192200229318518,0.0117941429503239,
-0.00903161764629643));
#34766=CARTESIAN_POINT('Ctrl Pts',(-0.192222852910695,0.0119862268713765,
-0.00893168204109561));
#34767=CARTESIAN_POINT('Ctrl Pts',(-0.192244557816236,0.0121587843232118,
-0.00883537905873995));
#34768=CARTESIAN_POINT('',(-0.192075076622818,0.00956760145971055,-0.00982142515813679));
#34769=CARTESIAN_POINT('Ctrl Pts',(-0.192075076622818,0.00956760145971055,
-0.00982142515813679));
#34770=CARTESIAN_POINT('Ctrl Pts',(-0.192073708408936,0.00962478404706063,
-0.00980871295728778));
#34771=CARTESIAN_POINT('Ctrl Pts',(-0.192072762001713,0.00967780303936765,
-0.00979636424425594));
#34772=CARTESIAN_POINT('Ctrl Pts',(-0.192072138417696,0.00972752489408203,
-0.00978441260142664));
#34773=CARTESIAN_POINT('Ctrl Pts',(-0.1920711088619,0.00980961715801607,
-0.00976468008293502));
#34774=CARTESIAN_POINT('Ctrl Pts',(-0.192070963831367,0.00988266913471998,
-0.00974582350900616));
#34775=CARTESIAN_POINT('Ctrl Pts',(-0.192071049839845,0.00991534567965813,
-0.0097372756757167));
#34776=CARTESIAN_POINT('Ctrl Pts',(-0.192071092844084,0.00993168395212721,
-0.00973300175907198));
#34777=CARTESIAN_POINT('Ctrl Pts',(-0.192071192640264,0.00993794032390922,
-0.00973134918095328));
#34778=CARTESIAN_POINT('Ctrl Pts',(-0.192071408671919,0.00995217223025025,
-0.0097275694112986));
#34779=CARTESIAN_POINT('Ctrl Pts',(-0.192071624703575,0.00996640413659128,
-0.00972378964164391));
#34780=CARTESIAN_POINT('Ctrl Pts',(-0.192071957564754,0.00998860428775286,
-0.00971785558555461));
#34781=CARTESIAN_POINT('Ctrl Pts',(-0.19207246071673,0.0100145240014813,
-0.00971078580027881));
#34782=CARTESIAN_POINT('Ctrl Pts',(-0.192073467020682,0.010066363428938,
-0.00969664622972721));
#34783=CARTESIAN_POINT('Ctrl Pts',(-0.192075153115435,0.0101331011051023,
-0.00967802702342739));
#34784=CARTESIAN_POINT('Ctrl Pts',(-0.192077829300968,0.0102151293872966,
-0.00965373321717447));
#34785=CARTESIAN_POINT('Ctrl Pts',(-0.19207925462564,0.0102588172904748,
-0.00964079444255896));
#34786=CARTESIAN_POINT('Ctrl Pts',(-0.192080960098135,0.010306848665772,
-0.00962627732697882));
#34787=CARTESIAN_POINT('Ctrl Pts',(-0.192083217793351,0.0103603962460601,
-0.00960945776125992));
#34788=CARTESIAN_POINT('',(-0.192177608446634,0.00780160333064341,-0.010046203453906));
#34789=CARTESIAN_POINT('Ctrl Pts',(-0.192177608446634,0.00780160333064341,
-0.010046203453906));
#34790=CARTESIAN_POINT('Ctrl Pts',(-0.192167966362081,0.00792071951974089,
-0.0100422162115806));
#34791=CARTESIAN_POINT('Ctrl Pts',(-0.192158463911435,0.00804293334057657,
-0.0100358383462041));
#34792=CARTESIAN_POINT('Ctrl Pts',(-0.192149221874634,0.00816902089203289,
-0.0100267146508605));
#34793=CARTESIAN_POINT('Ctrl Pts',(-0.192140658477299,0.00828584987955978,
-0.0100182609052117));
#34794=CARTESIAN_POINT('Ctrl Pts',(-0.192132320993025,0.00840599740158487,
-0.0100073464338714));
#34795=CARTESIAN_POINT('Ctrl Pts',(-0.192124643137378,0.00852403942360911,
-0.00999438297314338));
#34796=CARTESIAN_POINT('Ctrl Pts',(-0.192120804209555,0.00858306043462123,
-0.00998790124277939));
#34797=CARTESIAN_POINT('Ctrl Pts',(-0.192117128736142,0.00864156067840806,
-0.00998097171308127));
#34798=CARTESIAN_POINT('Ctrl Pts',(-0.192113255424149,0.00870685231601164,
-0.00997253562426482));
#34799=CARTESIAN_POINT('Ctrl Pts',(-0.192109382112156,0.00877214395361522,
-0.00996409953544838));
#34800=CARTESIAN_POINT('Ctrl Pts',(-0.192105316501578,0.00884419624784911,
-0.00995391015699222));
#34801=CARTESIAN_POINT('Ctrl Pts',(-0.192102640615622,0.00889274882880993,
-0.0099466716761585));
#34802=CARTESIAN_POINT('Ctrl Pts',(-0.192099964729666,0.00894130140977075,
-0.00993943319532478));
#34803=CARTESIAN_POINT('Ctrl Pts',(-0.192098671392472,0.00896640363023614,
-0.00993546631412305));
#34804=CARTESIAN_POINT('Ctrl Pts',(-0.192096901885914,0.0090014033603828,
-0.00992984074869916));
#34805=CARTESIAN_POINT('Ctrl Pts',(-0.192095132379357,0.00903640309052946,
-0.00992421518327526));
#34806=CARTESIAN_POINT('Ctrl Pts',(-0.192092889846057,0.00908127598741976,
-0.00991679012291164));
#34807=CARTESIAN_POINT('Ctrl Pts',(-0.192090632228416,0.00913068544408291,
-0.0099081590733559));
#34808=CARTESIAN_POINT('Ctrl Pts',(-0.192086116993135,0.00922950435740919,
-0.00989089697424441));
#34809=CARTESIAN_POINT('Ctrl Pts',(-0.192081547517015,0.00934643028253622,
-0.00986853887825808));
#34810=CARTESIAN_POINT('Ctrl Pts',(-0.192078312514945,0.00945039149167174,
-0.00984674944504866));
#34811=CARTESIAN_POINT('Ctrl Pts',(-0.192077036897294,0.00949138520680904,
-0.00983815749209412));
#34812=CARTESIAN_POINT('Ctrl Pts',(-0.19207596737083,0.00953037606040437,
-0.00982971706688361));
#34813=CARTESIAN_POINT('Ctrl Pts',(-0.192075076622818,0.00956760145971055,
-0.00982142515813679));
#34814=CARTESIAN_POINT('',(-0.192202406927022,0.00750306323134365,-0.0100515763887981));
#34815=CARTESIAN_POINT('Ctrl Pts',(-0.192202513508821,0.00750308895613145,
-0.010051578743107));
#34816=CARTESIAN_POINT('Ctrl Pts',(-0.19219416019488,0.00760065611110659,
-0.0100513580199758));
#34817=CARTESIAN_POINT('Ctrl Pts',(-0.192185833516719,0.00770000348444694,
-0.0100496541681167));
#34818=CARTESIAN_POINT('Ctrl Pts',(-0.192177608446634,0.00780160333064341,
-0.010046203453906));
#34819=CARTESIAN_POINT('',(-0.192248325555084,0.00283771562762635,-0.00883349052758685));
#34820=CARTESIAN_POINT('Ctrl Pts',(-0.192202406132311,0.0075030381940905,
-0.0100515763327894));
#34821=CARTESIAN_POINT('Ctrl Pts',(-0.192180243642943,0.00724060161082699,
-0.0100511599388438));
#34822=CARTESIAN_POINT('Ctrl Pts',(-0.192161403564018,0.00700671406050332,
-0.010039924073732));
#34823=CARTESIAN_POINT('Ctrl Pts',(-0.192146104291984,0.00680544197489901,
-0.010024804214849));
#34824=CARTESIAN_POINT('Ctrl Pts',(-0.192138454655968,0.00670480593209685,
-0.0100172442854074));
#34825=CARTESIAN_POINT('Ctrl Pts',(-0.192131689594209,0.00661232353382941,
-0.0100087410484208));
#34826=CARTESIAN_POINT('Ctrl Pts',(-0.192125592592653,0.00652423194571237,
-0.0099995109234971));
#34827=CARTESIAN_POINT('Ctrl Pts',(-0.192122544091875,0.00648018615165385,
-0.00999489586103524));
#34828=CARTESIAN_POINT('Ctrl Pts',(-0.192119663317349,0.00643724085037231,
-0.00999006751205205));
#34829=CARTESIAN_POINT('Ctrl Pts',(-0.192117246548196,0.00640051459612932,
-0.00998573832613764));
#34830=CARTESIAN_POINT('Ctrl Pts',(-0.192114829779043,0.00636378834188632,
-0.00998140914022324));
#34831=CARTESIAN_POINT('Ctrl Pts',(-0.192112874722809,0.00633326978455562,
-0.00997768108228416));
#34832=CARTESIAN_POINT('Ctrl Pts',(-0.192110173707211,0.00628802258600407,
-0.00997180968673719));
#34833=CARTESIAN_POINT('Ctrl Pts',(-0.192107472691613,0.00624277538745251,
-0.00996593829119022));
#34834=CARTESIAN_POINT('Ctrl Pts',(-0.192104029975276,0.00618282343766615,
-0.00995773385839349));
#34835=CARTESIAN_POINT('Ctrl Pts',(-0.192101053261483,0.00612740831063799,
-0.00994959447270961));
#34836=CARTESIAN_POINT('Ctrl Pts',(-0.192098076547689,0.00607199318360983,
-0.00994145508702573));
#34837=CARTESIAN_POINT('Ctrl Pts',(-0.192095562803207,0.00602109455563342,
-0.0099335162360786));
#34838=CARTESIAN_POINT('Ctrl Pts',(-0.192093220004145,0.00596989500140285,
-0.00992513296170256));
#34839=CARTESIAN_POINT('Ctrl Pts',(-0.192088534406023,0.0058674958929417,
-0.00990836641295047));
#34840=CARTESIAN_POINT('Ctrl Pts',(-0.192084536208433,0.005763920479537,
-0.00988966016638157));
#34841=CARTESIAN_POINT('Ctrl Pts',(-0.192081415054645,0.00566425619301311,
-0.00987003838255628));
#34842=CARTESIAN_POINT('Ctrl Pts',(-0.192075172747069,0.00546492761996531,
-0.00983079481490569));
#34843=CARTESIAN_POINT('Ctrl Pts',(-0.192072423513269,0.00528110931116734,
-0.0097885680268741));
#34844=CARTESIAN_POINT('Ctrl Pts',(-0.192073251416343,0.00509090909543717,
-0.00973895831064353));
#34845=CARTESIAN_POINT('Ctrl Pts',(-0.192074079319417,0.00490070887970699,
-0.00968934859441295));
#34846=CARTESIAN_POINT('Ctrl Pts',(-0.192078496030296,0.00470428524458125,
-0.00963182068569001));
#34847=CARTESIAN_POINT('Ctrl Pts',(-0.192087498668996,0.00450687929544704,
-0.00956675209872605));
#34848=CARTESIAN_POINT('Ctrl Pts',(-0.192090597557793,0.0044389282085873,
-0.00954435418607945));
#34849=CARTESIAN_POINT('Ctrl Pts',(-0.192094240798635,0.00437085466656924,
-0.00952106564267644));
#34850=CARTESIAN_POINT('Ctrl Pts',(-0.192098321240294,0.00430350915708436,
-0.00949717571328445));
#34851=CARTESIAN_POINT('Ctrl Pts',(-0.192106094964564,0.00417520799137725,
-0.00945166257049145));
#34852=CARTESIAN_POINT('Ctrl Pts',(-0.192115455498677,0.00404957328148242,
-0.00940391344723426));
#34853=CARTESIAN_POINT('Ctrl Pts',(-0.192125661936788,0.00393218901364697,
-0.0093566959282813));
#34854=CARTESIAN_POINT('Ctrl Pts',(-0.192133443844579,0.00384268927451646,
-0.00932069488907387));
#34855=CARTESIAN_POINT('Ctrl Pts',(-0.192141713192645,0.00375792550577707,
-0.00928514457643751));
#34856=CARTESIAN_POINT('Ctrl Pts',(-0.192150961541251,0.00366809730207177,
-0.00924584842708775));
#34857=CARTESIAN_POINT('Ctrl Pts',(-0.192155585715555,0.00362318320021912,
-0.00922620035241287));
#34858=CARTESIAN_POINT('Ctrl Pts',(-0.192160454647697,0.00357700519549584,
-0.00920561480746488));
#34859=CARTESIAN_POINT('Ctrl Pts',(-0.192166084452628,0.00352564880435533,
-0.00918214278170644));
#34860=CARTESIAN_POINT('Ctrl Pts',(-0.192171714257559,0.00347429241321481,
-0.009158670755948));
#34861=CARTESIAN_POINT('Ctrl Pts',(-0.192178107904039,0.00341782177126255,
-0.00913216947701166));
#34862=CARTESIAN_POINT('Ctrl Pts',(-0.192182856103435,0.00337653518451095,
-0.00911243306662588));
#34863=CARTESIAN_POINT('Ctrl Pts',(-0.192187604302832,0.00333524859775935,
-0.0090926966562401));
#34864=CARTESIAN_POINT('Ctrl Pts',(-0.192190702779538,0.00330904560688187,
-0.00907993339924628));
#34865=CARTESIAN_POINT('Ctrl Pts',(-0.192194848209666,0.00327420029768371,
-0.00906276405503103));
#34866=CARTESIAN_POINT('Ctrl Pts',(-0.192198993639795,0.00323935498848554,
-0.00904559471081578));
#34867=CARTESIAN_POINT('Ctrl Pts',(-0.192204188357678,0.00319592462016647,
-0.00902390474551468));
#34868=CARTESIAN_POINT('Ctrl Pts',(-0.192209757191958,0.00314991669976397,
-0.00900039555100338));
#34869=CARTESIAN_POINT('Ctrl Pts',(-0.192220894802916,0.00305790133484018,
-0.00895337740514728));
#34870=CARTESIAN_POINT('Ctrl Pts',(-0.192233524872454,0.00295546957808864,
-0.00889928118286497));
#34871=CARTESIAN_POINT('Ctrl Pts',(-0.192248325555084,0.00283771562762635,
-0.00883349052758685));
#34872=CARTESIAN_POINT('',(-0.191553952154239,0.00311173424349743,-0.00896743066851387));
#34873=CARTESIAN_POINT('Ctrl Pts',(-0.192248325784721,0.00283771380064023,
-0.00883348950682583));
#34874=CARTESIAN_POINT('Ctrl Pts',(-0.192159559175055,0.00287026003210736,
-0.00884999395305135));
#34875=CARTESIAN_POINT('Ctrl Pts',(-0.192051952701296,0.002909925198048,
-0.00886976448652076));
#34876=CARTESIAN_POINT('Ctrl Pts',(-0.191942427586231,0.00295087481736943,
-0.00888988564171143));
#34877=CARTESIAN_POINT('Ctrl Pts',(-0.191911532237965,0.00296233637983365,
-0.0088955006447997));
#34878=CARTESIAN_POINT('Ctrl Pts',(-0.191794791792164,0.00300748343666059,
-0.00891747224580303));
#34879=CARTESIAN_POINT('Ctrl Pts',(-0.19167990500933,0.00305483718076373,
-0.00894028783858838));
#34880=CARTESIAN_POINT('Ctrl Pts',(-0.191608493575298,0.00308573597984556,
-0.00895507813941301));
#34881=CARTESIAN_POINT('Ctrl Pts',(-0.191553952154239,0.00311173424349743,
-0.00896743066851387));
#34882=CARTESIAN_POINT('',(-0.190960920351713,0.00353164358673204,-0.00915988485915696));
#34883=CARTESIAN_POINT('Ctrl Pts',(-0.191553952154239,0.00311173424349743,
-0.00896743066851387));
#34884=CARTESIAN_POINT('Ctrl Pts',(-0.19155359586138,0.00311190407764358,
-0.00896751136164249));
#34885=CARTESIAN_POINT('Ctrl Pts',(-0.191498295283096,0.00313827803607244,
-0.00898004191267913));
#34886=CARTESIAN_POINT('Ctrl Pts',(-0.191373471881798,0.0032020936917313,
-0.00901021252823672));
#34887=CARTESIAN_POINT('Ctrl Pts',(-0.191231596802177,0.00329042310218504,
-0.00905130621942784));
#34888=CARTESIAN_POINT('Ctrl Pts',(-0.191109723337658,0.0033824962913484,
-0.0090935043810653));
#34889=CARTESIAN_POINT('Ctrl Pts',(-0.191016448616462,0.00346942958168849,
-0.0091324314801918));
#34890=CARTESIAN_POINT('Ctrl Pts',(-0.190985875275939,0.00350190193797071,
-0.00914685397494124));
#34891=CARTESIAN_POINT('Ctrl Pts',(-0.190959572667231,0.0035301458997474,
-0.00915922254898372));
#34892=CARTESIAN_POINT('Ctrl Pts',(-0.191002127391188,0.00750278968961046,
-0.0100244491176612));
#34893=CARTESIAN_POINT('Ctrl Pts',(-0.190990221104079,0.00736450438490425,
-0.0100242208049121));
#34894=CARTESIAN_POINT('Ctrl Pts',(-0.190976714774398,0.00720855534636783,
-0.01002089006384));
#34895=CARTESIAN_POINT('Ctrl Pts',(-0.19096297251905,0.00703989889402128,
-0.0100123976464476));
#34896=CARTESIAN_POINT('Ctrl Pts',(-0.190956101391376,0.006955570667848,
-0.0100081514377514));
#34897=CARTESIAN_POINT('Ctrl Pts',(-0.190949169912125,0.00686806652701917,
-0.0100026753145071));
#34898=CARTESIAN_POINT('Ctrl Pts',(-0.190942056597734,0.0067725971625629,
-0.00999519316408741));
#34899=CARTESIAN_POINT('Ctrl Pts',(-0.190938499940539,0.00672486248033477,
-0.00999145208887758));
#34900=CARTESIAN_POINT('Ctrl Pts',(-0.190934898866426,0.00667513881342257,
-0.00998716338353452));
#34901=CARTESIAN_POINT('Ctrl Pts',(-0.190931658652001,0.00663007179450303,
-0.00998295529844936));
#34902=CARTESIAN_POINT('Ctrl Pts',(-0.190928418437576,0.00658500477558349,
-0.0099787472133642));
#34903=CARTESIAN_POINT('Ctrl Pts',(-0.190925534780746,0.00654457897619451,
-0.00997481061464137));
#34904=CARTESIAN_POINT('Ctrl Pts',(-0.19092132251379,0.00647953294953688,
-0.00996770967567637));
#34905=CARTESIAN_POINT('Ctrl Pts',(-0.190917110246834,0.00641448692287925,
-0.00996060873671137));
#34906=CARTESIAN_POINT('Ctrl Pts',(-0.190911579923794,0.00632486907082429,
-0.00994987435196803));
#34907=CARTESIAN_POINT('Ctrl Pts',(-0.190907267674604,0.00624812638706539,
-0.00993961898765824));
#34908=CARTESIAN_POINT('Ctrl Pts',(-0.190902955425414,0.00617138370330648,
-0.00992936362334845));
#34909=CARTESIAN_POINT('Ctrl Pts',(-0.190899852732142,0.0061074629321523,
-0.00991996732482893));
#34910=CARTESIAN_POINT('Ctrl Pts',(-0.19089715233397,0.00604732256013647,
-0.00991064863510685));
#34911=CARTESIAN_POINT('Ctrl Pts',(-0.190891751537625,0.00592704181610479,
-0.00989201125566268));
#34912=CARTESIAN_POINT('Ctrl Pts',(-0.190887966444545,0.00582194003441517,
-0.00987339125729909));
#34913=CARTESIAN_POINT('Ctrl Pts',(-0.190885369196734,0.0057370259760568,
-0.00985739551877355));
#34914=CARTESIAN_POINT('Ctrl Pts',(-0.190882771948922,0.00565211191769842,
-0.00984139978024802));
#34915=CARTESIAN_POINT('Ctrl Pts',(-0.190881361562531,0.00558737163844979,
-0.00982807330323891));
#34916=CARTESIAN_POINT('Ctrl Pts',(-0.190880516547924,0.00554736685038776,
-0.00981970824679295));
#34917=CARTESIAN_POINT('Ctrl Pts',(-0.190879671533318,0.00550736206232573,
-0.00981134319034699));
#34918=CARTESIAN_POINT('Ctrl Pts',(-0.190879390734427,0.00549208313057967,
-0.00980799146704673));
#34919=CARTESIAN_POINT('Ctrl Pts',(-0.190879230051964,0.0054773044431616,
-0.00980478925362853));
#34920=CARTESIAN_POINT('Ctrl Pts',(-0.190879069369502,0.00546252575574354,
-0.00980158704021034));
#34921=CARTESIAN_POINT('Ctrl Pts',(-0.190879028737872,0.0054482467302615,
-0.00979853728640441));
#34922=CARTESIAN_POINT('Ctrl Pts',(-0.190878983617291,0.00540844431622106,
-0.00978961469117975));
#34923=CARTESIAN_POINT('Ctrl Pts',(-0.19087893849671,0.00536864190218062,
-0.00978069209595509));
#34924=CARTESIAN_POINT('Ctrl Pts',(-0.190878890080572,0.0053033293280606,
-0.00976584248435005));
#34925=CARTESIAN_POINT('Ctrl Pts',(-0.190879598832768,0.00521811957514347,
-0.00974492384284556));
#34926=CARTESIAN_POINT('Ctrl Pts',(-0.190880307584965,0.00513290982222635,
-0.00972400520134109));
#34927=CARTESIAN_POINT('Ctrl Pts',(-0.190881774469879,0.00502780711904499,
-0.00969697509695359));
#34928=CARTESIAN_POINT('Ctrl Pts',(-0.190884578999687,0.00490824705285926,
-0.00966337665691388));
#34929=CARTESIAN_POINT('Ctrl Pts',(-0.19088598126459,0.00484846701976639,
-0.00964657743689403));
#34930=CARTESIAN_POINT('Ctrl Pts',(-0.190887716330757,0.00478505569684817,
-0.00962820893403036));
#34931=CARTESIAN_POINT('Ctrl Pts',(-0.190890410878822,0.00470957227208617,
-0.00960523613729057));
#34932=CARTESIAN_POINT('Ctrl Pts',(-0.190893105426888,0.00463408884732416,
-0.00958226334055077));
#34933=CARTESIAN_POINT('Ctrl Pts',(-0.190896767981085,0.0045466489712431,
-0.00955429495332745));
#34934=CARTESIAN_POINT('Ctrl Pts',(-0.190899553155149,0.00448481957625672,
-0.00953379913870298));
#34935=CARTESIAN_POINT('Ctrl Pts',(-0.190902338329213,0.00442299018127034,
-0.0095133033240785));
#34936=CARTESIAN_POINT('Ctrl Pts',(-0.190904235759669,0.00438660942184642,
-0.00950076099502019));
#34937=CARTESIAN_POINT('Ctrl Pts',(-0.190906434316899,0.00434482368852979,
-0.00948618781464346));
#34938=CARTESIAN_POINT('Ctrl Pts',(-0.190907050637439,0.00433310991307086,
-0.00948210252167129));
#34939=CARTESIAN_POINT('Ctrl Pts',(-0.190907690955913,0.0043209760970172,
-0.00947784468285007));
#34940=CARTESIAN_POINT('Ctrl Pts',(-0.190908348288388,0.00430858853902742,
-0.00947346796251659));
#34941=CARTESIAN_POINT('Ctrl Pts',(-0.190910035812157,0.00427678682632307,
-0.00946223191399535));
#34942=CARTESIAN_POINT('Ctrl Pts',(-0.190911835469614,0.00424331587844342,
-0.00945020363068093));
#34943=CARTESIAN_POINT('Ctrl Pts',(-0.190913629094266,0.00421096117813992,
-0.00943837282589162));
#34944=CARTESIAN_POINT('Ctrl Pts',(-0.190918613666388,0.00412104585670863,
-0.00940549443093067));
#34945=CARTESIAN_POINT('Ctrl Pts',(-0.190923547291744,0.00403969563693671,
-0.00937427513158476));
#34946=CARTESIAN_POINT('Ctrl Pts',(-0.190928497783178,0.00396137688375242,
-0.00934312046999013));
#34947=CARTESIAN_POINT('Ctrl Pts',(-0.190938398766047,0.00380473937738384,
-0.00928081114680089));
#34948=CARTESIAN_POINT('Ctrl Pts',(-0.190948372721054,0.00366035364625716,
-0.00921849341705995));
#34949=CARTESIAN_POINT('Ctrl Pts',(-0.190957165817421,0.00353276917114798,
-0.00916037178863552));
#34950=CARTESIAN_POINT('Ctrl Pts',(-0.227150244243996,0.0164740029315869,
0.00232534147293063));
#34951=CARTESIAN_POINT('Ctrl Pts',(-0.237845216608682,0.0163630583331681,
0.00229659353481578));
#34952=CARTESIAN_POINT('Ctrl Pts',(-0.227150244243996,0.0164948323843597,
0.00192393728845175));
#34953=CARTESIAN_POINT('Ctrl Pts',(-0.237845216608682,0.0163665512368261,
0.0018892790127829));
#34954=CARTESIAN_POINT('Ctrl Pts',(-0.227150244243996,0.0165287121322363,
0.00114598487796074));
#34955=CARTESIAN_POINT('Ctrl Pts',(-0.237845216608682,0.0163722325524412,
0.00111537528026272));
#34956=CARTESIAN_POINT('Ctrl Pts',(-0.227150244243996,0.0165470707859482,
-9.63426955345028E-15));
#34957=CARTESIAN_POINT('Ctrl Pts',(-0.237845216608682,0.0163753111262956,
-3.20734770353177E-16));
#34958=CARTESIAN_POINT('Ctrl Pts',(-0.227150244243997,0.0165287121322335,
-0.00114598487798004));
#34959=CARTESIAN_POINT('Ctrl Pts',(-0.237845216608682,0.0163722325524407,
-0.00111537528026388));
#34960=CARTESIAN_POINT('Ctrl Pts',(-0.227150244243996,0.0164948323843552,
-0.00192393728847136));
#34961=CARTESIAN_POINT('Ctrl Pts',(-0.237845216608682,0.0163665512368254,
-0.00188927901278524));
#34962=CARTESIAN_POINT('Ctrl Pts',(-0.227150244243996,0.0164156764744566,
-0.00344935006783133));
#34963=CARTESIAN_POINT('Ctrl Pts',(-0.237845216608682,0.0163532775339462,
-0.0034371522067016));
#34964=CARTESIAN_POINT('Ctrl Pts',(-0.227150244243997,0.0158708078188047,
-0.00568348814190198));
#34965=CARTESIAN_POINT('Ctrl Pts',(-0.237845216608683,0.0158878089324482,
-0.00572426400319885));
#34966=CARTESIAN_POINT('Ctrl Pts',(-0.227150244243996,0.0138592003117079,
-0.00851222286772063));
#34967=CARTESIAN_POINT('Ctrl Pts',(-0.237845216608682,0.0139254525795067,
-0.00865325189315152));
#34968=CARTESIAN_POINT('Ctrl Pts',(-0.227150244243997,0.0109293641084061,
-0.0103996324725637));
#34969=CARTESIAN_POINT('Ctrl Pts',(-0.237845216608683,0.0109812780384655,
-0.0106210180177305));
#34970=CARTESIAN_POINT('Ctrl Pts',(-0.227150244243996,0.0074999999998714,
-0.0110623240930123));
#34971=CARTESIAN_POINT('Ctrl Pts',(-0.237845216608682,0.00749999999987136,
-0.01131420416039));
#34972=CARTESIAN_POINT('Ctrl Pts',(-0.227150244243997,0.00407063589135525,
-0.0103996324724683));
#34973=CARTESIAN_POINT('Ctrl Pts',(-0.237845216608683,0.00401872196129691,
-0.0106210180176321));
#34974=CARTESIAN_POINT('Ctrl Pts',(-0.227150244243996,0.00114079968810594,
-0.00851222286754358));
#34975=CARTESIAN_POINT('Ctrl Pts',(-0.237845216608682,0.00107454742031117,
-0.00865325189296982));
#34976=CARTESIAN_POINT('Ctrl Pts',(-0.227150244243997,-0.000870807818911773,
-0.00568348814166902));
#34977=CARTESIAN_POINT('Ctrl Pts',(-0.237845216608682,-0.00088780893254747,
-0.00572426400296157));
#34978=CARTESIAN_POINT('Ctrl Pts',(-0.227150244243996,-0.00141567647450146,
-0.00344935006758328));
#34979=CARTESIAN_POINT('Ctrl Pts',(-0.237845216608682,-0.00135327753398082,
-0.00343715220645101));
#34980=CARTESIAN_POINT('Ctrl Pts',(-0.227150244243996,-0.00149483238436559,
-0.00192393728824214));
#34981=CARTESIAN_POINT('Ctrl Pts',(-0.237845216608682,-0.00136655123682709,
-0.00188927901255543));
#34982=CARTESIAN_POINT('Ctrl Pts',(-0.227150244243996,-0.0015287121322383,
-0.00114598487779204));
#34983=CARTESIAN_POINT('Ctrl Pts',(-0.237845216608682,-0.00137223255244152,
-0.0011153752800763));
#34984=CARTESIAN_POINT('Ctrl Pts',(-0.227150244243997,-0.00154707078594764,
1.16062262795529E-13));
#34985=CARTESIAN_POINT('Ctrl Pts',(-0.237845216608682,-0.00137531112629545,
1.24505090562086E-13));
#34986=CARTESIAN_POINT('Ctrl Pts',(-0.227150244243996,-0.00152871213223388,
0.00114598487802365));
#34987=CARTESIAN_POINT('Ctrl Pts',(-0.237845216608682,-0.00137223255244077,
0.00111537528032471));
#34988=CARTESIAN_POINT('Ctrl Pts',(-0.227150244243996,-0.0014948323843583,
0.00192393728847254));
#34989=CARTESIAN_POINT('Ctrl Pts',(-0.237845216608682,-0.00136655123682587,
0.00188927901280252));
#34990=CARTESIAN_POINT('Ctrl Pts',(-0.227150244243996,-0.00141567647446389,
0.00344935006836688));
#34991=CARTESIAN_POINT('Ctrl Pts',(-0.237845216608682,-0.00135327753394768,
0.00343715220737864));
#34992=CARTESIAN_POINT('Ctrl Pts',(-0.227150244243997,-0.000870821762961343,
0.00568349039573915));
#34993=CARTESIAN_POINT('Ctrl Pts',(-0.237845216608682,-0.000887826039510656,
0.00572426676828764));
#34994=CARTESIAN_POINT('Ctrl Pts',(-0.227150244243997,0.00114085439618864,
0.00851222287679413));
#34995=CARTESIAN_POINT('Ctrl Pts',(-0.237845216608682,0.0010746145376654,
0.00865325190429854));
#34996=CARTESIAN_POINT('Ctrl Pts',(-0.227150244243996,0.00407062011024736,
0.0103996408584618));
#34997=CARTESIAN_POINT('Ctrl Pts',(-0.237845216608682,0.00401870260056976,
0.0106210283057897));
#34998=CARTESIAN_POINT('Ctrl Pts',(-0.227150244243997,0.00750000000000013,
0.0110623211795783));
#34999=CARTESIAN_POINT('Ctrl Pts',(-0.237845216608683,0.00749999999999948,
0.0113142005861093));
#35000=CARTESIAN_POINT('Ctrl Pts',(-0.227150244243996,0.0109293798897529,
0.0103996408584618));
#35001=CARTESIAN_POINT('Ctrl Pts',(-0.237845216608681,0.0109812973994292,
0.0106210283057901));
#35002=CARTESIAN_POINT('Ctrl Pts',(-0.227150244243997,0.0138591456038116,
0.00851222287679417));
#35003=CARTESIAN_POINT('Ctrl Pts',(-0.237845216608683,0.0139253854623337,
0.00865325190429944));
#35004=CARTESIAN_POINT('Ctrl Pts',(-0.227150244243997,0.0158708217629616,
0.00568349039573924));
#35005=CARTESIAN_POINT('Ctrl Pts',(-0.237845216608682,0.0158878260395101,
0.00572426676828895));
#35006=CARTESIAN_POINT('Ctrl Pts',(-0.227150244243996,0.0164156764744642,
0.00344935006836702));
#35007=CARTESIAN_POINT('Ctrl Pts',(-0.237845216608682,0.0163532775339475,
0.00343715220738017));
#35008=CARTESIAN_POINT('Ctrl Pts',(-0.227150244243996,0.0164740029315869,
0.00232534147293065));
#35009=CARTESIAN_POINT('Ctrl Pts',(-0.237845216608682,0.0163630583331681,
0.0022965935348158));
#35010=CARTESIAN_POINT('Ctrl Pts',(-0.228219847986792,0.016461711610013,
0.00232234304728456));
#35011=CARTESIAN_POINT('Ctrl Pts',(-0.228197323008168,0.016464402919773,
0.00228169207879242));
#35012=CARTESIAN_POINT('Ctrl Pts',(-0.228079010729088,0.0164779108194991,
0.00206553236692686));
#35013=CARTESIAN_POINT('Ctrl Pts',(-0.227880678619148,0.0164952290445269,
0.00167731055896527));
#35014=CARTESIAN_POINT('Ctrl Pts',(-0.227674259713159,0.0165145714831501,
0.00121095180943624));
#35015=CARTESIAN_POINT('Ctrl Pts',(-0.227539125616474,0.0165251767327821,
0.000875323514963339));
#35016=CARTESIAN_POINT('Ctrl Pts',(-0.227433352259856,0.0165318672222558,
0.000599149205354619));
#35017=CARTESIAN_POINT('Ctrl Pts',(-0.227387103565297,0.0165342612366672,
0.000474629663494434));
#35018=CARTESIAN_POINT('Ctrl Pts',(-0.227320232205383,0.0165373421710725,
0.000293417962783554));
#35019=CARTESIAN_POINT('Ctrl Pts',(-0.227259872684817,0.0165392417731146,
0.00012778562427802));
#35020=CARTESIAN_POINT('Ctrl Pts',(-0.22721365317106,0.0165399630933673,
2.96878969900656E-7));
#35021=CARTESIAN_POINT('Ctrl Pts',(-0.230613689225592,0.0164370167296803,
0.00231666183293795));
#35022=CARTESIAN_POINT('Ctrl Pts',(-0.230153199896009,0.0164750623910427,
0.00163855477769135));
#35023=CARTESIAN_POINT('Ctrl Pts',(-0.229898110941495,0.0164961381222382,
0.000819433299928898));
#35024=CARTESIAN_POINT('Ctrl Pts',(-0.22989804971791,0.016496143666697,
2.94875754180074E-7));
#35025=CARTESIAN_POINT('Ctrl Pts',(-0.228031317757249,0.0074842289792918,
0.0108613267143847));
#35026=CARTESIAN_POINT('Ctrl Pts',(-0.227896128234583,0.00732271517640735,
0.0108579839540074));
#35027=CARTESIAN_POINT('Ctrl Pts',(-0.227765076018135,0.00716310491063475,
0.010850325819301));
#35028=CARTESIAN_POINT('Ctrl Pts',(-0.227510609193765,0.00684731467260396,
0.0108270338085957));
#35029=CARTESIAN_POINT('Ctrl Pts',(-0.227389668743883,0.00669440562499774,
0.010811585495654));
#35030=CARTESIAN_POINT('Ctrl Pts',(-0.227162362130326,0.00640136431994779,
0.0107751132274823));
#35031=CARTESIAN_POINT('Ctrl Pts',(-0.227055775511969,0.00626093688400325,
0.0107540679242784));
#35032=CARTESIAN_POINT('Ctrl Pts',(-0.226906495617072,0.0060594832359516,
0.010719534205083));
#35033=CARTESIAN_POINT('Ctrl Pts',(-0.226858502324212,0.00599386222138074,
0.0107075273154425));
#35034=CARTESIAN_POINT('Ctrl Pts',(-0.226766049082705,0.00586567726531639,
0.0106827143943246));
#35035=CARTESIAN_POINT('Ctrl Pts',(-0.226722124661603,0.00580387778100626,
0.010670098269507));
#35036=CARTESIAN_POINT('Ctrl Pts',(-0.226585218374531,0.00560808410484936,
0.0106279534125427));
#35037=CARTESIAN_POINT('Ctrl Pts',(-0.22649022366447,0.00546820172234809,
0.0105949410804036));
#35038=CARTESIAN_POINT('Ctrl Pts',(-0.226366825461877,0.00528228167215783,
0.010545833840231));
#35039=CARTESIAN_POINT('Ctrl Pts',(-0.226342874294171,0.00524602651289862,
0.0105360458953431));
#35040=CARTESIAN_POINT('Ctrl Pts',(-0.226286724768651,0.0051604222146116,
0.0105122439934791));
#35041=CARTESIAN_POINT('Ctrl Pts',(-0.226255147092778,0.00511204014714452,
0.0104984660406559));
#35042=CARTESIAN_POINT('Ctrl Pts',(-0.22614990532583,0.00495042207797637,
0.0104506682428966));
#35043=CARTESIAN_POINT('Ctrl Pts',(-0.226065736316993,0.00482068030019097,
0.0104102462744603));
#35044=CARTESIAN_POINT('Ctrl Pts',(-0.22596754801256,0.00467004487225661,
0.0103583034518151));
#35045=CARTESIAN_POINT('Ctrl Pts',(-0.228033577259197,0.00748440686309183,
0.0107613524026377));
#35046=CARTESIAN_POINT('Ctrl Pts',(-0.227898387621481,0.00732471444696238,
0.0107580128797965));
#35047=CARTESIAN_POINT('Ctrl Pts',(-0.227767333526622,0.00716689330363822,
0.0107504075964718));
#35048=CARTESIAN_POINT('Ctrl Pts',(-0.227512859749499,0.00685462755823802,
0.0107273112564122));
#35049=CARTESIAN_POINT('Ctrl Pts',(-0.227391914277135,0.00670341734486022,
0.0107120043085084));
#35050=CARTESIAN_POINT('Ctrl Pts',(-0.227164595337582,0.00641362330544489,
0.0106758791788512));
#35051=CARTESIAN_POINT('Ctrl Pts',(-0.227058001408668,0.0062747475907083,
0.0106550398501494));
#35052=CARTESIAN_POINT('Ctrl Pts',(-0.226908709318108,0.00607551732420086,
0.0106208500119865));
#35053=CARTESIAN_POINT('Ctrl Pts',(-0.226860711754346,0.00601062006567001,
0.0106089635890604));
#35054=CARTESIAN_POINT('Ctrl Pts',(-0.226768249633801,0.00588384843464617,
0.0105844012148158));
#35055=CARTESIAN_POINT('Ctrl Pts',(-0.226724320673869,0.00582273009633135,
0.0105719132109536));
#35056=CARTESIAN_POINT('Ctrl Pts',(-0.226587399145727,0.00562909428433601,
0.01053019877818));
#35057=CARTESIAN_POINT('Ctrl Pts',(-0.226492392400433,0.00549075322107965,
0.0104975265728443));
#35058=CARTESIAN_POINT('Ctrl Pts',(-0.226368976136859,0.00530688423445996,
0.0104489304488435));
#35059=CARTESIAN_POINT('Ctrl Pts',(-0.226345021363545,0.00527102914326667,
0.0104392445660052));
#35060=CARTESIAN_POINT('Ctrl Pts',(-0.226288863050377,0.00518636992476106,
0.0104156915057688));
#35061=CARTESIAN_POINT('Ctrl Pts',(-0.226257280279058,0.00513852220521404,
0.0104020578835452));
#35062=CARTESIAN_POINT('Ctrl Pts',(-0.22615202079073,0.00497869053802895,
0.0103547623018));
#35063=CARTESIAN_POINT('Ctrl Pts',(-0.226067836783359,0.00485038433404092,
0.0103147666318135));
#35064=CARTESIAN_POINT('Ctrl Pts',(-0.225969628990936,0.00470142166790477,
0.0102633762890857));
#35065=CARTESIAN_POINT('Ctrl Pts',(-0.228033588556707,0.00748440775251083,
0.010760852531079));
#35066=CARTESIAN_POINT('Ctrl Pts',(-0.227898398918416,0.00732472444331515,
0.0107575130244254));
#35067=CARTESIAN_POINT('Ctrl Pts',(-0.227767344814165,0.00716691224560324,
0.0107499080053577));
#35068=CARTESIAN_POINT('Ctrl Pts',(-0.227512871002277,0.00685466412266619,
0.0107268126436513));
#35069=CARTESIAN_POINT('Ctrl Pts',(-0.227391925504801,0.00670346240345954,
0.0107115064025727));
#35070=CARTESIAN_POINT('Ctrl Pts',(-0.227164606503619,0.00641368460037238,
0.010675383008608));
#35071=CARTESIAN_POINT('Ctrl Pts',(-0.227058012538152,0.00627481664424182,
0.0106545447097788));
#35072=CARTESIAN_POINT('Ctrl Pts',(-0.226908720386613,0.00607559749464211,
0.010620356591021));
#35073=CARTESIAN_POINT('Ctrl Pts',(-0.226860722801496,0.00601070385489146,
0.0106084707704285));
#35074=CARTESIAN_POINT('Ctrl Pts',(-0.226768260636557,0.00588393929049282,
0.0105839096489183));
#35075=CARTESIAN_POINT('Ctrl Pts',(-0.226724331653931,0.00582282435790797,
0.0105714222856609));
#35076=CARTESIAN_POINT('Ctrl Pts',(-0.226587410049583,0.00562919933523344,
0.0105297100050082));
#35077=CARTESIAN_POINT('Ctrl Pts',(-0.226492403244113,0.00549086597857331,
0.0104970395003065));
#35078=CARTESIAN_POINT('Ctrl Pts',(-0.226368986890234,0.00530700724727147,
0.0104484459318865));
#35079=CARTESIAN_POINT('Ctrl Pts',(-0.226345032098891,0.00527115415641851,
0.0104387605593585));
#35080=CARTESIAN_POINT('Ctrl Pts',(-0.226288873741786,0.00518649966331181,
0.0104152087433303));
#35081=CARTESIAN_POINT('Ctrl Pts',(-0.22625729094499,0.00513865461550439,
0.0104015758427596));
#35082=CARTESIAN_POINT('Ctrl Pts',(-0.226152031368055,0.00497883188032922,
0.0103542827720945));
#35083=CARTESIAN_POINT('Ctrl Pts',(-0.226067847285692,0.00485053285421017,
0.0103142892336002));
#35084=CARTESIAN_POINT('Ctrl Pts',(-0.225969639395827,0.00470157855188301,
0.0102629016532721));
#35085=CARTESIAN_POINT('',(-0.228033577259201,0.00748440686309334,0.0107613524025277));
#35086=CARTESIAN_POINT('',(-0.225967548079419,0.0046700458803542,0.0103583004019229));
#35087=CARTESIAN_POINT('Ctrl Pts',(-0.228074264635775,0.00750982551816477,
-0.0108453770253309));
#35088=CARTESIAN_POINT('Ctrl Pts',(-0.228010676434541,0.00740838976828053,
-0.0105824436407257));
#35089=CARTESIAN_POINT('Ctrl Pts',(-0.2279824250062,0.00743349469607835,
-0.0102960204663357));
#35090=CARTESIAN_POINT('Ctrl Pts',(-0.227032943648517,0.00632417137993069,
-0.0115546191985225));
#35091=CARTESIAN_POINT('Ctrl Pts',(-0.226887473210818,0.00609211727794893,
-0.0109531076947852));
#35092=CARTESIAN_POINT('Ctrl Pts',(-0.226822842547162,0.0061495497066744,
-0.0102978587061822));
#35093=CARTESIAN_POINT('Ctrl Pts',(-0.226297317381162,0.00493120265784604,
-0.0122699105575636));
#35094=CARTESIAN_POINT('Ctrl Pts',(-0.226063698082153,0.00455853369847132,
-0.0113039088181618));
#35095=CARTESIAN_POINT('Ctrl Pts',(-0.225959904001537,0.00465076772176458,
-0.0102516069772177));
#35096=CARTESIAN_POINT('',(-0.228051045268546,0.00748331776699234,-0.0108612187236825));
#35097=CARTESIAN_POINT('Ctrl Pts',(-0.228054819889729,0.00748068141629659,
-0.0107604444270582));
#35098=CARTESIAN_POINT('Ctrl Pts',(-0.228053849738522,0.00748110294260517,
-0.0107931625663296));
#35099=CARTESIAN_POINT('Ctrl Pts',(-0.228052595462817,0.00748196696929443,
-0.0108267367625979));
#35100=CARTESIAN_POINT('Ctrl Pts',(-0.228051045268536,0.00748331776753071,
-0.0108612187236609));
#35101=CARTESIAN_POINT('',(-0.225969776335003,0.0046444390782959,-0.010349214474902));
#35102=CARTESIAN_POINT('Ctrl Pts',(-0.225970412829803,0.00464426457540287,
-0.010349129960529));
#35103=CARTESIAN_POINT('Ctrl Pts',(-0.22636217413668,0.00527485403368463,
-0.0105691174221872));
#35104=CARTESIAN_POINT('Ctrl Pts',(-0.226793102923008,0.00589537795378531,
-0.0107098724323669));
#35105=CARTESIAN_POINT('Ctrl Pts',(-0.227558354882916,0.00688782458229315,
-0.0108376974244079));
#35106=CARTESIAN_POINT('Ctrl Pts',(-0.227831875264664,0.00721793479916253,
-0.0108558255878856));
#35107=CARTESIAN_POINT('Ctrl Pts',(-0.228051045268268,0.007483317767219,
-0.0108612187237897));
#35108=CARTESIAN_POINT('Ctrl Pts',(-0.225969808834085,0.00464327366247554,
-0.0103488652066219));
#35109=CARTESIAN_POINT('Ctrl Pts',(-0.225970621228311,0.00465291285345407,
-0.0103160414183464));
#35110=CARTESIAN_POINT('Ctrl Pts',(-0.225971427024039,0.00466253501940138,
-0.0102838463488178));
#35111=CARTESIAN_POINT('Ctrl Pts',(-0.225972227593275,0.00467213421594552,
-0.0102522642048503));
#35112=CARTESIAN_POINT('Origin',(-0.226575103310132,0.00449228442477202,
-0.00733395845215797));
#35113=CARTESIAN_POINT('',(-0.226088434634005,0.00750609353843923,-0.010817348945422));
#35114=CARTESIAN_POINT('Ctrl Pts',(-0.226088397422881,0.00750571596719848,
-0.0108173527010167));
#35115=CARTESIAN_POINT('Ctrl Pts',(-0.226046795568232,0.00707975121101806,
-0.0108166967955858));
#35116=CARTESIAN_POINT('Ctrl Pts',(-0.226012355211352,0.00663228020961852,
-0.0107848740755647));
#35117=CARTESIAN_POINT('Ctrl Pts',(-0.225963781900347,0.00565398292249233,
-0.0106396516049241));
#35118=CARTESIAN_POINT('Ctrl Pts',(-0.225955904863431,0.00512512163672698,
-0.0105097994417222));
#35119=CARTESIAN_POINT('Ctrl Pts',(-0.225969743835921,0.00464560449411625,
-0.0103495637431821));
#35120=CARTESIAN_POINT('Ctrl Pts',(-0.226088471845129,0.00750647110967997,
-0.0108173451898272));
#35121=CARTESIAN_POINT('Ctrl Pts',(-0.226091014474231,0.00750607256368142,
-0.010783628416141));
#35122=CARTESIAN_POINT('Ctrl Pts',(-0.226093586961953,0.00750568099604601,
-0.0107499136549416));
#35123=CARTESIAN_POINT('Ctrl Pts',(-0.226096189362409,0.00750529647355148,
-0.0107162198524223));
#35124=CARTESIAN_POINT('Origin',(-0.215,-0.00247776328493882,0.0055));
#35125=CARTESIAN_POINT('',(-0.215000000652701,-0.000412667879180649,0.0055002646485004));
#35126=CARTESIAN_POINT('',(-0.192200819587666,-0.000325482083450908,0.0055001426619674));
#35127=CARTESIAN_POINT('Ctrl Pts',(-0.215000000137371,-0.000412703772444445,
0.00550080483265447));
#35128=CARTESIAN_POINT('Ctrl Pts',(-0.207400273519179,-0.000383662849035535,
0.00550259700144263));
#35129=CARTESIAN_POINT('Ctrl Pts',(-0.199800545652181,-0.000354576027343994,
0.005502376420274));
#35130=CARTESIAN_POINT('Ctrl Pts',(-0.192200819587666,-0.000325482083450908,
0.0055001426619674));
#35131=CARTESIAN_POINT('',(-0.192768810477056,-0.000446740227034733,0.00549999916447762));
#35132=CARTESIAN_POINT('Origin',(-0.194168411395185,0.0075,0.0055));
#35133=CARTESIAN_POINT('',(-0.203737790159114,-0.000488441743501772,0.00550001369129769));
#35134=CARTESIAN_POINT('Ctrl Pts',(-0.192768810477182,-0.000446740193101186,
0.00549999665791052));
#35135=CARTESIAN_POINT('Ctrl Pts',(-0.196360853593688,-0.000461346127092089,
0.00549997224869372));
#35136=CARTESIAN_POINT('Ctrl Pts',(-0.200017180154384,-0.000475246610178321,
0.00550000407222806));
#35137=CARTESIAN_POINT('Ctrl Pts',(-0.203737790159114,-0.000488441743501772,
0.00550001369129769));
#35138=CARTESIAN_POINT('',(-0.214999999997124,-0.000525629251200218,0.0055000000000044));
#35139=CARTESIAN_POINT('Ctrl Pts',(-0.203737790159114,-0.000488441743501772,
0.00550001369129769));
#35140=CARTESIAN_POINT('Ctrl Pts',(-0.207428602217097,-0.000501531198487641,
0.00550002323332928));
#35141=CARTESIAN_POINT('Ctrl Pts',(-0.211182672164629,-0.000513926566459491,
0.00550001115861136));
#35142=CARTESIAN_POINT('Ctrl Pts',(-0.214999999996537,-0.000525629250696233,
0.00550005330994453));
#35143=CARTESIAN_POINT('',(-0.215,-0.00247776328493882,0.0055));
#35144=CARTESIAN_POINT('Origin',(-0.215,-0.00247776328493882,0.0055));
#35145=CARTESIAN_POINT('',(-0.215000000652833,0.0154126678792567,0.00550026464927285));
#35146=CARTESIAN_POINT('',(-0.214999999997124,0.0155256292511986,0.0055000000000044));
#35147=CARTESIAN_POINT('',(-0.215,-0.00247776328493882,0.0055));
#35148=CARTESIAN_POINT('',(-0.20373779012803,0.015488441743392,0.00550001369129815));
#35149=CARTESIAN_POINT('Ctrl Pts',(-0.214999999996537,0.0155256292506966,
0.0055000533099388));
#35150=CARTESIAN_POINT('Ctrl Pts',(-0.211182672153911,0.0155139265664271,
0.00550001115860741));
#35151=CARTESIAN_POINT('Ctrl Pts',(-0.207428602197274,0.0155015308720983,
0.00549998488159998));
#35152=CARTESIAN_POINT('Ctrl Pts',(-0.20373779012803,0.015488441743392,
0.00550001369129815));
#35153=CARTESIAN_POINT('',(-0.192768810477057,0.0154467402270351,0.00549999916447917));
#35154=CARTESIAN_POINT('Ctrl Pts',(-0.20373779012803,0.015488441743392,
0.00550001369129815));
#35155=CARTESIAN_POINT('Ctrl Pts',(-0.200017180135304,0.0154752462761579,
0.00549996529271644));
#35156=CARTESIAN_POINT('Ctrl Pts',(-0.196360853583685,0.0154613461270517,
0.00549997224869849));
#35157=CARTESIAN_POINT('Ctrl Pts',(-0.192768810477184,0.0154467401931016,
0.00549999665791672));
#35158=CARTESIAN_POINT('',(-0.192200819587632,0.0153254820834438,0.00550014266023027));
#35159=CARTESIAN_POINT('Origin',(-0.194168411395185,0.0075,0.0055));
#35160=CARTESIAN_POINT('Ctrl Pts',(-0.192200819587632,0.0153254820834438,
0.00550014266023027));
#35161=CARTESIAN_POINT('Ctrl Pts',(-0.199800545652162,0.0153545760275143,
0.00550237641958232));
#35162=CARTESIAN_POINT('Ctrl Pts',(-0.207400273519175,0.0153836628489491,
0.00550259700179216));
#35163=CARTESIAN_POINT('Ctrl Pts',(-0.215000000137363,0.0154127037724312,
0.00550080483406418));
#35164=CARTESIAN_POINT('Origin',(-0.215,-0.00247776328493882,-0.0055));
#35165=CARTESIAN_POINT('',(-0.21499999999666,-0.00052563024928965,-0.00550000000000594));
#35166=CARTESIAN_POINT('',(-0.215000000652509,-0.000412669026508687,-0.00550026458441123));
#35167=CARTESIAN_POINT('',(-0.215,-0.00247776328493882,-0.0055));
#35168=CARTESIAN_POINT('',(-0.203436374848878,-0.000487371363831537,-0.00550001526954719));
#35169=CARTESIAN_POINT('Ctrl Pts',(-0.214999999995963,-0.000525630248646836,
-0.0055000585798767));
#35170=CARTESIAN_POINT('Ctrl Pts',(-0.211078734069006,-0.000513608696396548,
-0.00550001184318302));
#35171=CARTESIAN_POINT('Ctrl Pts',(-0.207224192351256,-0.000500856290275313,
-0.00550002560630164));
#35172=CARTESIAN_POINT('Ctrl Pts',(-0.203436374848878,-0.000487371363831537,
-0.00550001526954719));
#35173=CARTESIAN_POINT('',(-0.192317997805077,-0.000444941992647508,-0.0054999973805848));
#35174=CARTESIAN_POINT('Ctrl Pts',(-0.203436374848878,-0.000487371363831537,
-0.00550001526954719));
#35175=CARTESIAN_POINT('Ctrl Pts',(-0.19966407605156,-0.000473941685191043,
-0.00550000497514246));
#35176=CARTESIAN_POINT('Ctrl Pts',(-0.19595795585078,-0.000459785480996097,
-0.00549997085736725));
#35177=CARTESIAN_POINT('Ctrl Pts',(-0.192318014246932,-0.000444902576975657,
-0.00549999627590324));
#35178=CARTESIAN_POINT('',(-0.192182752978689,-0.00032540324872727,-0.00550013765774565));
#35179=CARTESIAN_POINT('Ctrl Pts',(-0.192317958818237,-0.000445035454884037,
-0.00549999999999998));
#35180=CARTESIAN_POINT('Ctrl Pts',(-0.192281469524508,-0.000429789928121892,
-0.00549999999999998));
#35181=CARTESIAN_POINT('Ctrl Pts',(-0.192251227013467,-0.000413059060916608,
-0.00549999999897596));
#35182=CARTESIAN_POINT('Ctrl Pts',(-0.192217246193221,-0.000387604767502657,
-0.00549999999897596));
#35183=CARTESIAN_POINT('Ctrl Pts',(-0.192201562270466,-0.000374406090242385,
-0.00550000000001939));
#35184=CARTESIAN_POINT('Ctrl Pts',(-0.192187769696388,-0.000353338816389856,
-0.00550000000001939));
#35185=CARTESIAN_POINT('Ctrl Pts',(-0.192184706735899,-0.000347322586940135,
-0.00549999999999998));
#35186=CARTESIAN_POINT('Ctrl Pts',(-0.192182140916727,-0.0003382625628242,
-0.00549999999999998));
#35187=CARTESIAN_POINT('Ctrl Pts',(-0.192181602954142,-0.000335449050862324,
-0.00549999999999998));
#35188=CARTESIAN_POINT('Ctrl Pts',(-0.192181177992225,-0.000330149245389187,
-0.00549999999999998));
#35189=CARTESIAN_POINT('Ctrl Pts',(-0.192181212347043,-0.00032770017804238,
-0.00549999999999998));
#35190=CARTESIAN_POINT('Ctrl Pts',(-0.192181505015942,-0.000325264067446612,
-0.00549999999999998));
#35191=CARTESIAN_POINT('Ctrl Pts',(-0.192182752978689,-0.00032540324872727,
-0.00550013765774565));
#35192=CARTESIAN_POINT('Ctrl Pts',(-0.199788501242498,-0.00035452409238897,
-0.00550237637378411));
#35193=CARTESIAN_POINT('Ctrl Pts',(-0.207394251315731,-0.000383637427213978,
-0.0055025986106267));
#35194=CARTESIAN_POINT('Ctrl Pts',(-0.215000000137357,-0.000412704938748334,
-0.00550080479377357));
#35195=CARTESIAN_POINT('Origin',(-0.215,-0.00247776328493882,-0.0055));
#35196=CARTESIAN_POINT('',(-0.215000000653156,0.0154126690265686,-0.00550026455391182));
#35197=CARTESIAN_POINT('',(-0.192200822396014,0.0153254827916868,-0.00550014285674479));
#35198=CARTESIAN_POINT('Ctrl Pts',(-0.215000000137355,0.0154127049387179,
-0.005500804798221));
#35199=CARTESIAN_POINT('Ctrl Pts',(-0.207400274455338,0.0153836638777327,
-0.0055025971330885));
#35200=CARTESIAN_POINT('Ctrl Pts',(-0.199800547524418,0.0153545768886244,
-0.00550237662849891));
#35201=CARTESIAN_POINT('Ctrl Pts',(-0.192200822396014,0.0153254827916868,
-0.00550014285674479));
#35202=CARTESIAN_POINT('',(-0.192768813717413,0.0154467407873535,-0.00549999832876385));
#35203=CARTESIAN_POINT('Origin',(-0.194168411395185,0.0075,-0.0055));
#35204=CARTESIAN_POINT('',(-0.203737786417006,0.0154884425231616,-0.00550001369217832));
#35205=CARTESIAN_POINT('Ctrl Pts',(-0.1927688137175,0.0154467407637849,
-0.0054999966575277));
#35206=CARTESIAN_POINT('Ctrl Pts',(-0.196360852334629,0.0154613467899902,
-0.00549997224670963));
#35207=CARTESIAN_POINT('Ctrl Pts',(-0.200017176569134,0.0154752470087536,
-0.00549996529032058));
#35208=CARTESIAN_POINT('Ctrl Pts',(-0.203737786417006,0.0154884425231616,
-0.00550001369217832));
#35209=CARTESIAN_POINT('',(-0.214999999997124,0.0155256300978718,-0.0055000000000044));
#35210=CARTESIAN_POINT('Ctrl Pts',(-0.203737786417006,0.0154884425231616,
-0.00550001369217832));
#35211=CARTESIAN_POINT('Ctrl Pts',(-0.207428597610741,0.0155015316960027,
-0.00549998488064372));
#35212=CARTESIAN_POINT('Ctrl Pts',(-0.211182668804386,0.0155139274126174,
-0.00550001115947315));
#35213=CARTESIAN_POINT('Ctrl Pts',(-0.214999999996537,0.0155256300973698,
-0.0055000533136723));
#35214=CARTESIAN_POINT('',(-0.215,-0.00247776328493882,-0.0055));
#35215=CARTESIAN_POINT('Origin',(-0.227003760671838,0.00749996257915086,
-0.00184311590365041));
#35216=CARTESIAN_POINT('',(-0.225965850681397,0.0102943062435013,-0.0103692862560009));
#35217=CARTESIAN_POINT('Ctrl Pts',(-0.228051045268804,0.00748331776721652,
-0.0108612187238017));
#35218=CARTESIAN_POINT('Ctrl Pts',(-0.228046268562556,0.0074888841515757,
-0.0108611222719965));
#35219=CARTESIAN_POINT('Ctrl Pts',(-0.228041495105673,0.00749445191188697,
-0.0108610207252172));
#35220=CARTESIAN_POINT('Ctrl Pts',(-0.227530170041864,0.0080914144788298,
-0.0108495888326834));
#35221=CARTESIAN_POINT('Ctrl Pts',(-0.227035276032252,0.00872930600873977,
-0.0107790866609926));
#35222=CARTESIAN_POINT('Ctrl Pts',(-0.226365419755937,0.0096839489506607,
-0.0105596857066268));
#35223=CARTESIAN_POINT('Ctrl Pts',(-0.226161417598064,0.00998868739612624,
-0.0104735785805751));
#35224=CARTESIAN_POINT('Ctrl Pts',(-0.225966633299167,0.0102930893843531,
-0.0103697246588685));
#35225=CARTESIAN_POINT('Ctrl Pts',(-0.225965034805744,0.0102941399146425,
-0.0103693454509162));
#35226=CARTESIAN_POINT('Ctrl Pts',(-0.225943934273099,0.00937798607974839,
-0.010668449685717));
#35227=CARTESIAN_POINT('Ctrl Pts',(-0.225999253113111,0.00841521474472878,
-0.0108147357619121));
#35228=CARTESIAN_POINT('Ctrl Pts',(-0.226088508031683,0.00750609596646259,
-0.0108173549212978));
#35229=CARTESIAN_POINT('Ctrl Pts',(-0.185819463593633,0.0166104930553049,
0.00236863820262676));
#35230=CARTESIAN_POINT('Ctrl Pts',(-0.203223508587672,0.0164247592890707,
0.00234416866113263));
#35231=CARTESIAN_POINT('Ctrl Pts',(-0.220627582451438,0.0162418056983084,
0.00231971009381821));
#35232=CARTESIAN_POINT('Ctrl Pts',(-0.238031675744303,0.0160611171225611,
0.00229373846137714));
#35233=CARTESIAN_POINT('Ctrl Pts',(-0.18581926440362,0.0166461165277183,
0.00221607060080922));
#35234=CARTESIAN_POINT('Ctrl Pts',(-0.203223313044138,0.0164497831264032,
0.00218726310900855));
#35235=CARTESIAN_POINT('Ctrl Pts',(-0.220627389279833,0.0162559154123599,
0.00215868502272393));
#35236=CARTESIAN_POINT('Ctrl Pts',(-0.238031485810861,0.0160641905057161,
0.0021289558365353));
#35237=CARTESIAN_POINT('Ctrl Pts',(-0.185818880874426,0.0167106984888996,
0.00190682671781972));
#35238=CARTESIAN_POINT('Ctrl Pts',(-0.203222934036142,0.0164938099422013,
0.00186885154579339));
#35239=CARTESIAN_POINT('Ctrl Pts',(-0.220627006269502,0.016278128585195,
0.00183193650018925));
#35240=CARTESIAN_POINT('Ctrl Pts',(-0.238031099947329,0.0160640878015832,
0.00179531454904686));
#35241=CARTESIAN_POINT('Ctrl Pts',(-0.185818335405062,0.0168157482814852,
0.00126613919744405));
#35242=CARTESIAN_POINT('Ctrl Pts',(-0.203222383696577,0.0165663597906042,
0.00122992539721983));
#35243=CARTESIAN_POINT('Ctrl Pts',(-0.220626440719063,0.016317358802535,
0.00119476376827596));
#35244=CARTESIAN_POINT('Ctrl Pts',(-0.238030512988197,0.0160691276034975,
0.00116079870997399));
#35245=CARTESIAN_POINT('Ctrl Pts',(-0.185817827209109,0.0169242355148058,
9.8641936611403E-5));
#35246=CARTESIAN_POINT('Ctrl Pts',(-0.203221858920215,0.0166409437466787,
9.11218039920294E-5));
#35247=CARTESIAN_POINT('Ctrl Pts',(-0.220625885580743,0.0163575362327447,
8.39196676156386E-5));
#35248=CARTESIAN_POINT('Ctrl Pts',(-0.238029902001653,0.0160736640759679,
7.73368998092213E-5));
#35249=CARTESIAN_POINT('Ctrl Pts',(-0.185818130580629,0.0168405937503755,
-0.00127155898818726));
#35250=CARTESIAN_POINT('Ctrl Pts',(-0.20322218710562,0.0165814424082619,
-0.00122048351610829));
#35251=CARTESIAN_POINT('Ctrl Pts',(-0.220626248932598,0.0163217805675101,
-0.0011714081373514));
#35252=CARTESIAN_POINT('Ctrl Pts',(-0.238030331796423,0.0160627645050436,
-0.00112492380137579));
#35253=CARTESIAN_POINT('Ctrl Pts',(-0.185819629874682,0.0165908497836556,
-0.00251327778772927));
#35254=CARTESIAN_POINT('Ctrl Pts',(-0.203223673996629,0.0164148787644927,
-0.00249147144795656));
#35255=CARTESIAN_POINT('Ctrl Pts',(-0.220627751907747,0.0162423115134214,
-0.00246930645840148));
#35256=CARTESIAN_POINT('Ctrl Pts',(-0.238031849291733,0.0160723190230807,
-0.00244485415145052));
#35257=CARTESIAN_POINT('Ctrl Pts',(-0.185821321884765,0.016234179304769,
-0.00369798898814236));
#35258=CARTESIAN_POINT('Ctrl Pts',(-0.203225319480993,0.0161450945583953,
-0.00371151425360031));
#35259=CARTESIAN_POINT('Ctrl Pts',(-0.220629323053567,0.0160579626760164,
-0.0037253545768972));
#35260=CARTESIAN_POINT('Ctrl Pts',(-0.238033334942443,0.0159726607261184,
-0.00373864195256771));
#35261=CARTESIAN_POINT('Ctrl Pts',(-0.185823245401148,0.0155679236134438,
-0.00510694903431088));
#35262=CARTESIAN_POINT('Ctrl Pts',(-0.203227224653483,0.0155630775790093,
-0.00518221799309441));
#35263=CARTESIAN_POINT('Ctrl Pts',(-0.220631203569159,0.0155602580016752,
-0.00525755181874107));
#35264=CARTESIAN_POINT('Ctrl Pts',(-0.238035184380882,0.0155591988240479,
-0.00533210507472633));
#35265=CARTESIAN_POINT('Ctrl Pts',(-0.185825309557818,0.0144549166529026,
-0.00659829769408909));
#35266=CARTESIAN_POINT('Ctrl Pts',(-0.203229286524981,0.0145155596341981,
-0.00676015088892623));
#35267=CARTESIAN_POINT('Ctrl Pts',(-0.22063325576454,0.0145775956365756,
-0.00692214625038456));
#35268=CARTESIAN_POINT('Ctrl Pts',(-0.238037222353744,0.0146408934228599,
-0.00708388886226514));
#35269=CARTESIAN_POINT('Ctrl Pts',(-0.185827024933535,0.0130736100782548,
-0.00784141832828519));
#35270=CARTESIAN_POINT('Ctrl Pts',(-0.203231018325486,0.0131627927804585,
-0.00809004931086922));
#35271=CARTESIAN_POINT('Ctrl Pts',(-0.220635004750871,0.0132529981228345,
-0.00833876091410667));
#35272=CARTESIAN_POINT('Ctrl Pts',(-0.238038987871232,0.0133440928006999,
-0.00858734922546909));
#35273=CARTESIAN_POINT('Ctrl Pts',(-0.18582832438757,0.0114765605098063,
-0.00878674958056091));
#35274=CARTESIAN_POINT('Ctrl Pts',(-0.203232338232321,0.0115609317972438,
-0.00910975493295771));
#35275=CARTESIAN_POINT('Ctrl Pts',(-0.220636347717917,0.011645972461393,
-0.00943280869850027));
#35276=CARTESIAN_POINT('Ctrl Pts',(-0.238040354954934,0.011731574352546,
-0.00975583575545302));
#35277=CARTESIAN_POINT('Ctrl Pts',(-0.185829453345315,0.0091451966229997,
-0.0096057242773119));
#35278=CARTESIAN_POINT('Ctrl Pts',(-0.203233491880005,0.00919013323193661,
-0.00999827176177371));
#35279=CARTESIAN_POINT('Ctrl Pts',(-0.220637530309762,0.00923531471374497,
-0.010390817424762));
#35280=CARTESIAN_POINT('Ctrl Pts',(-0.23804156864792,0.00928068353228921,
-0.0107833654056958));
#35281=CARTESIAN_POINT('Ctrl Pts',(-0.185829632293992,0.00601552622584051,
-0.00973743542872093));
#35282=CARTESIAN_POINT('Ctrl Pts',(-0.203233675322875,0.00597352188698778,
-0.0101422781507738));
#35283=CARTESIAN_POINT('Ctrl Pts',(-0.220637719137517,0.00593129183613322,
-0.0105471134497117));
#35284=CARTESIAN_POINT('Ctrl Pts',(-0.238041763362071,0.00588889329790392,
-0.0109519477983446));
#35285=CARTESIAN_POINT('Ctrl Pts',(-0.185828144842012,0.0030739290209801,
-0.00865481883805552));
#35286=CARTESIAN_POINT('Ctrl Pts',(-0.203232153522101,0.0029784477533647,
-0.00896475560878426));
#35287=CARTESIAN_POINT('Ctrl Pts',(-0.22063615670017,0.00288224573504626,
-0.00927474912637149));
#35288=CARTESIAN_POINT('Ctrl Pts',(-0.23804015699596,0.00278543581335185,
-0.00958473005637672));
#35289=CARTESIAN_POINT('Ctrl Pts',(-0.185826082022641,0.00110130832095057,
-0.00715935834428723));
#35290=CARTESIAN_POINT('Ctrl Pts',(-0.203230064435315,0.00102431113527,
-0.00735889669894074));
#35291=CARTESIAN_POINT('Ctrl Pts',(-0.220634039193033,0.000946044449726581,
-0.00755853937500263));
#35292=CARTESIAN_POINT('Ctrl Pts',(-0.238038010705833,0.000866655562235164,
-0.00775795997137017));
#35293=CARTESIAN_POINT('Ctrl Pts',(-0.185824164055499,-0.00013244480670859,
-0.0057658502018965));
#35294=CARTESIAN_POINT('Ctrl Pts',(-0.20322813912978,-0.000160334959886128,
-0.00587671276434198));
#35295=CARTESIAN_POINT('Ctrl Pts',(-0.220632108537853,-0.000189837833944718,
-0.0059877445582653));
#35296=CARTESIAN_POINT('Ctrl Pts',(-0.238036077190852,-0.000220820008254192,
-0.00609839080888522));
#35297=CARTESIAN_POINT('Ctrl Pts',(-0.185822299173595,-0.000912009378582172,
-0.00442360049681092));
#35298=CARTESIAN_POINT('Ctrl Pts',(-0.203226287658242,-0.000866786568362782,
-0.00446783414154759));
#35299=CARTESIAN_POINT('Ctrl Pts',(-0.220630281624252,-0.00082387334949089,
-0.00451207377872994));
#35300=CARTESIAN_POINT('Ctrl Pts',(-0.23803428087264,-0.000782904229550054,
-0.00455527877134414));
#35301=CARTESIAN_POINT('Ctrl Pts',(-0.185820718130017,-0.00137009218103609,
-0.00326760896710645));
#35302=CARTESIAN_POINT('Ctrl Pts',(-0.203224730158278,-0.00125053240292857,
-0.00326719962044019));
#35303=CARTESIAN_POINT('Ctrl Pts',(-0.220628754805288,-0.00113312156821255,
-0.00326706607813972));
#35304=CARTESIAN_POINT('Ctrl Pts',(-0.23803279135031,-0.00101767765869665,
-0.00326612878115765));
#35305=CARTESIAN_POINT('Ctrl Pts',(-0.185819647933685,-0.00158153457958364,
-0.00252531449976026));
#35306=CARTESIAN_POINT('Ctrl Pts',(-0.203223692052988,-0.00140575636354931,
-0.00250567473614365));
#35307=CARTESIAN_POINT('Ctrl Pts',(-0.220627772291069,-0.00123370234183487,
-0.00248543365897305));
#35308=CARTESIAN_POINT('Ctrl Pts',(-0.238031871675392,-0.001064293369006,
-0.00246259728183289));
#35309=CARTESIAN_POINT('Ctrl Pts',(-0.185818880874262,-0.00171069848643351,
-0.00190682671492207));
#35310=CARTESIAN_POINT('Ctrl Pts',(-0.203222934035982,-0.0014938099322336,
-0.00186885153402852));
#35311=CARTESIAN_POINT('Ctrl Pts',(-0.220627006269333,-0.00127812856598612,
-0.00183193647922556));
#35312=CARTESIAN_POINT('Ctrl Pts',(-0.238031099947143,-0.00106408777175675,
-0.00179531451994465));
#35313=CARTESIAN_POINT('Ctrl Pts',(-0.185818335405171,-0.0018157482831674,
-0.00126613919912989));
#35314=CARTESIAN_POINT('Ctrl Pts',(-0.203222383696684,-0.00156635979742609,
-0.00122992540382135));
#35315=CARTESIAN_POINT('Ctrl Pts',(-0.220626440719173,-0.00131735881546124,
-0.00119476377996408));
#35316=CARTESIAN_POINT('Ctrl Pts',(-0.238030512988314,-0.00106912762331005,
-0.00116079872610497));
#35317=CARTESIAN_POINT('Ctrl Pts',(-0.185817827208834,-0.00192423551004945,
-9.86419358357781E-5));
#35318=CARTESIAN_POINT('Ctrl Pts',(-0.203221858919953,-0.00164094372766557,
-9.11218007194661E-5));
#35319=CARTESIAN_POINT('Ctrl Pts',(-0.220625885580502,-0.00135753619911081,
-8.39196619480522E-5));
#35320=CARTESIAN_POINT('Ctrl Pts',(-0.238029902001436,-0.00107366402718548,
-7.73368926939811E-5));
#35321=CARTESIAN_POINT('Ctrl Pts',(-0.185818130581901,-0.00184059377323484,
0.00127155899038818));
#35322=CARTESIAN_POINT('Ctrl Pts',(-0.20322218710682,-0.00158144249928501,
0.00122048352511737));
#35323=CARTESIAN_POINT('Ctrl Pts',(-0.220626248933645,-0.00132178072462663,
0.0011714081546043));
#35324=CARTESIAN_POINT('Ctrl Pts',(-0.238030331797288,-0.00106276472807202,
0.00112492383001885));
#35325=CARTESIAN_POINT('Ctrl Pts',(-0.185819629872525,-0.00159084974486086,
0.00251327778358106));
#35326=CARTESIAN_POINT('Ctrl Pts',(-0.203223673994595,-0.00141487860996912,
0.00249147143135548));
#35327=CARTESIAN_POINT('Ctrl Pts',(-0.220627751905974,-0.00124231124688325,
0.00246930642685937));
#35328=CARTESIAN_POINT('Ctrl Pts',(-0.238031849290273,-0.00107231864497727,
0.00244485409969644));
#35329=CARTESIAN_POINT('Ctrl Pts',(-0.185821321898498,-0.00123417951568875,
0.00369798917224086));
#35330=CARTESIAN_POINT('Ctrl Pts',(-0.203225319494204,-0.00114509540859564,
0.003711514992569));
#35331=CARTESIAN_POINT('Ctrl Pts',(-0.22062932306665,-0.00105796426044417,
0.00372535589828007));
#35332=CARTESIAN_POINT('Ctrl Pts',(-0.238033334955726,-0.000972663126262614,
0.00373864380762799));
#35333=CARTESIAN_POINT('Ctrl Pts',(-0.185823245436368,-0.000567924396732498,
0.00510694905821607));
#35334=CARTESIAN_POINT('Ctrl Pts',(-0.203227224690427,-0.000563080693363035,
0.00518221807967137));
#35335=CARTESIAN_POINT('Ctrl Pts',(-0.220631203607128,-0.000560263335972913,
0.00525755189961067));
#35336=CARTESIAN_POINT('Ctrl Pts',(-0.238035184419129,-0.000559206262722732,
0.00533210518716677));
#35337=CARTESIAN_POINT('Ctrl Pts',(-0.185825309451763,0.000545085685742881,
0.00659829745055551));
#35338=CARTESIAN_POINT('Ctrl Pts',(-0.203229286420574,0.000484449699432902,
0.00676014989093362));
#35339=CARTESIAN_POINT('Ctrl Pts',(-0.220633255665466,0.000422420785569872,
0.00692214425104443));
#35340=CARTESIAN_POINT('Ctrl Pts',(-0.238037222262465,0.000359130275923251,
0.00708388576133197));
#35341=CARTESIAN_POINT('Ctrl Pts',(-0.18582702479622,0.00192639486310074,
0.00784141870119505));
#35342=CARTESIAN_POINT('Ctrl Pts',(-0.203231018176613,0.00183722692142162,
0.00809005081566443));
#35343=CARTESIAN_POINT('Ctrl Pts',(-0.22063500458984,0.00174703627304292,
0.00833876365528797));
#35344=CARTESIAN_POINT('Ctrl Pts',(-0.238038987697963,0.00165595618969436,
0.00858735323957588));
#35345=CARTESIAN_POINT('Ctrl Pts',(-0.185828324413572,0.00352344076961579,
0.00878675040966002));
#35346=CARTESIAN_POINT('Ctrl Pts',(-0.203232338254504,0.00343907331273139,
0.00910975824932868));
#35347=CARTESIAN_POINT('Ctrl Pts',(-0.220636347734676,0.00335403651878359,
0.00943281459138894));
#35348=CARTESIAN_POINT('Ctrl Pts',(-0.238040354964937,0.00326843848901562,
0.00975584429234039));
#35349=CARTESIAN_POINT('Ctrl Pts',(-0.185829453384424,0.00585480099283502,
0.00960572462550227));
#35350=CARTESIAN_POINT('Ctrl Pts',(-0.203233491922009,0.00580985725942693,
0.00999827314311295));
#35351=CARTESIAN_POINT('Ctrl Pts',(-0.220637530355488,0.00576466867020715,
0.0103908197967745));
#35352=CARTESIAN_POINT('Ctrl Pts',(-0.238041568698001,0.00571929278241239,
0.01078336873748));
#35353=CARTESIAN_POINT('Ctrl Pts',(-0.185829632324535,0.00898447703279034,
0.00973743551044517));
#35354=CARTESIAN_POINT('Ctrl Pts',(-0.20323367535712,0.00902649110858287,
0.0101422784667701));
#35355=CARTESIAN_POINT('Ctrl Pts',(-0.220637719176512,0.00906873086433049,
0.0105471139309657));
#35356=CARTESIAN_POINT('Ctrl Pts',(-0.238041763406542,0.00911113903768637,
0.0109519484055942));
#35357=CARTESIAN_POINT('Ctrl Pts',(-0.185828144821879,0.0119260676124901,
0.00865481978154805));
#35358=CARTESIAN_POINT('Ctrl Pts',(-0.203232153491178,0.0120215388163693,
0.00896475940006844));
#35359=CARTESIAN_POINT('Ctrl Pts',(-0.220636156655006,0.0121177307814799,
0.00927475599174944));
#35360=CARTESIAN_POINT('Ctrl Pts',(-0.238040156934043,0.0122145307595023,
0.00958474013175701));
#35361=CARTESIAN_POINT('Ctrl Pts',(-0.185826081864447,0.0138986875060143,
0.0071593582727713));
#35362=CARTESIAN_POINT('Ctrl Pts',(-0.203230064272376,0.0139756722252048,
0.00735889640414339));
#35363=CARTESIAN_POINT('Ctrl Pts',(-0.22063403902823,0.0140539264607635,
0.00755853873522353));
#35364=CARTESIAN_POINT('Ctrl Pts',(-0.238038010541502,0.0141333028562059,
0.00775795890451245));
#35365=CARTESIAN_POINT('Ctrl Pts',(-0.185824164045733,0.0151324448001649,
0.00576585000582876));
#35366=CARTESIAN_POINT('Ctrl Pts',(-0.203228139124408,0.0151603349181088,
0.00587671195695743));
#35367=CARTESIAN_POINT('Ctrl Pts',(-0.220632108538343,0.0151898375748212,
0.00598774292639455));
#35368=CARTESIAN_POINT('Ctrl Pts',(-0.238036077197705,0.0152208192897305,
0.00609838833446442));
#35369=CARTESIAN_POINT('Ctrl Pts',(-0.185822299200829,0.01591200987427,
0.00442360064358258));
#35370=CARTESIAN_POINT('Ctrl Pts',(-0.203226287685109,0.0158667885469009,
0.00446783472845091));
#35371=CARTESIAN_POINT('Ctrl Pts',(-0.220630281650178,0.0158238768216512,
0.00451207481602829));
#35372=CARTESIAN_POINT('Ctrl Pts',(-0.238034280897302,0.0157829092105071,
0.00455528026393975));
#35373=CARTESIAN_POINT('Ctrl Pts',(-0.185820718137045,0.0163700922862437,
0.00326760909611432));
#35374=CARTESIAN_POINT('Ctrl Pts',(-0.203224730165169,0.0162505328296095,
0.00326720013800919));
#35375=CARTESIAN_POINT('Ctrl Pts',(-0.220628754812585,0.0161331223929292,
0.00326706699899929));
#35376=CARTESIAN_POINT('Ctrl Pts',(-0.238032791358368,0.016017678941859,
0.00326613005920909));
#35377=CARTESIAN_POINT('Ctrl Pts',(-0.18581986197366,0.0165392461104783,
0.00267377340626184));
#35378=CARTESIAN_POINT('Ctrl Pts',(-0.203223899674741,0.0163747116144059,
0.00265797976538081));
#35379=CARTESIAN_POINT('Ctrl Pts',(-0.220627968794648,0.0162135862702056,
0.00264176023600675));
#35380=CARTESIAN_POINT('Ctrl Pts',(-0.238032055611188,0.016054970356251,
0.00262330371106081));
#35381=CARTESIAN_POINT('Ctrl Pts',(-0.185819463593633,0.0166104930553049,
0.00236863820262676));
#35382=CARTESIAN_POINT('Ctrl Pts',(-0.203223508587672,0.0164247592890707,
0.00234416866113263));
#35383=CARTESIAN_POINT('Ctrl Pts',(-0.220627582451438,0.0162418056983084,
0.00231971009381821));
#35384=CARTESIAN_POINT('Ctrl Pts',(-0.238031675744303,0.0160611171225611,
0.00229373846137714));
#35385=CARTESIAN_POINT('',(-0.230843542066567,0.0161181286545946,-0.00261043832732274));
#35386=CARTESIAN_POINT('Origin',(-0.233966934007412,0.0158592789729621,
3.09238363249698E-10));
#35387=CARTESIAN_POINT('',(-0.237700712870106,0.0075106460066284,-0.0107797928880335));
#35388=CARTESIAN_POINT('Ctrl Pts',(-0.230843549406418,0.0161191164318998,
-0.00261050690091829));
#35389=CARTESIAN_POINT('Ctrl Pts',(-0.231651983552228,0.0160415721496965,
-0.00357365221582349));
#35390=CARTESIAN_POINT('Ctrl Pts',(-0.232444275696972,0.0158161744526218,
-0.00451766730635352));
#35391=CARTESIAN_POINT('Ctrl Pts',(-0.233207651413396,0.0154317497833547,
-0.00542716549495472));
#35392=CARTESIAN_POINT('Ctrl Pts',(-0.233971028171898,0.015047324589313,
-0.00633666492510352));
#35393=CARTESIAN_POINT('Ctrl Pts',(-0.234705524570036,0.0145039610841376,
-0.00721168853739024));
#35394=CARTESIAN_POINT('Ctrl Pts',(-0.235365783247194,0.0137804475678366,
-0.00799824442316078));
#35395=CARTESIAN_POINT('Ctrl Pts',(-0.235367844562095,0.0137781887725434,
-0.00800070003551994));
#35396=CARTESIAN_POINT('Ctrl Pts',(-0.235369905152796,0.0137759282229903,
-0.00800315478243444));
#35397=CARTESIAN_POINT('Ctrl Pts',(-0.235371965017888,0.0137736659185172,
-0.0080056086622658));
#35398=CARTESIAN_POINT('Ctrl Pts',(-0.235699802297696,0.013413609453079,
-0.00839615525278972));
#35399=CARTESIAN_POINT('Ctrl Pts',(-0.236009265872864,0.0130091028997178,
-0.00876475090758743));
#35400=CARTESIAN_POINT('Ctrl Pts',(-0.236288883258456,0.012561367000027,
-0.00909784263196301));
#35401=CARTESIAN_POINT('Ctrl Pts',(-0.236570257534211,0.0121108178890046,
-0.00943302723612366));
#35402=CARTESIAN_POINT('Ctrl Pts',(-0.236821407837358,0.011616490160412,
-0.00973226987547397));
#35403=CARTESIAN_POINT('Ctrl Pts',(-0.237030704738135,0.0110795136094463,
-0.00998162692863499));
#35404=CARTESIAN_POINT('Ctrl Pts',(-0.237240001638912,0.0105425370584806,
-0.010230983981796));
#35405=CARTESIAN_POINT('Ctrl Pts',(-0.237407392556333,0.00996285229092137,
-0.0104303849821952));
#35406=CARTESIAN_POINT('Ctrl Pts',(-0.237522490752224,0.00936122795465865,
-0.0105674930798237));
#35407=CARTESIAN_POINT('Ctrl Pts',(-0.237637588948116,0.00875960361839593,
-0.0107046011774521));
#35408=CARTESIAN_POINT('Ctrl Pts',(-0.237700401438083,0.00813606422858096,
-0.0107794203282436));
#35409=CARTESIAN_POINT('Ctrl Pts',(-0.237700712551084,0.00751133792318635,
-0.0107797925062651));
#35410=CARTESIAN_POINT('',(-0.230843542079837,-0.00111813185800299,-0.00261043853789162));
#35411=CARTESIAN_POINT('Ctrl Pts',(-0.237700712870106,0.0075106460066284,
-0.0107797928880335));
#35412=CARTESIAN_POINT('Ctrl Pts',(-0.237700977736204,0.00688614944423556,
-0.0107801099748839));
#35413=CARTESIAN_POINT('Ctrl Pts',(-0.237638789092914,0.006260444451203,
-0.0107060307146087));
#35414=CARTESIAN_POINT('Ctrl Pts',(-0.237524351321969,0.0056561909426634,
-0.0105697092990888));
#35415=CARTESIAN_POINT('Ctrl Pts',(-0.237409871286876,0.0050517142712691,
-0.0104333375373553));
#35416=CARTESIAN_POINT('Ctrl Pts',(-0.237243099478524,0.00446872868422436,
-0.0102346738447992));
#35417=CARTESIAN_POINT('Ctrl Pts',(-0.23703442323106,0.00392995420914097,
-0.00998606057911376));
#35418=CARTESIAN_POINT('Ctrl Pts',(-0.236825746983597,0.00339117973405756,
-0.0097374473134283));
#35419=CARTESIAN_POINT('Ctrl Pts',(-0.236575219550393,0.00289655692010007,
-0.00943895248021973));
#35420=CARTESIAN_POINT('Ctrl Pts',(-0.236294506432514,0.00244619039703509,
-0.00910455462484356));
#35421=CARTESIAN_POINT('Ctrl Pts',(-0.236015370943784,0.00199835496820744,
-0.0087720361109401));
#35422=CARTESIAN_POINT('Ctrl Pts',(-0.235706389506389,0.00159427631684454,
-0.00840400801450611));
#35423=CARTESIAN_POINT('Ctrl Pts',(-0.235379088265152,0.00123416570953253,
-0.00801409801864759));
#35424=CARTESIAN_POINT('Ctrl Pts',(-0.23537723841087,0.00123213042195969,
-0.00801189430969545));
#35425=CARTESIAN_POINT('Ctrl Pts',(-0.2353753879712,0.00123009653891891,
-0.0080096899013831));
#35426=CARTESIAN_POINT('Ctrl Pts',(-0.235373536947083,0.0012280640599786,
-0.00800748479480728));
#35427=CARTESIAN_POINT('Ctrl Pts',(-0.234714818450409,0.000504771769989926,
-0.00722276001697017));
#35428=CARTESIAN_POINT('Ctrl Pts',(-0.233982182394368,-4.06098583481195E-5,
-0.00634993382838675));
#35429=CARTESIAN_POINT('Ctrl Pts',(-0.233216597089855,-0.00042724483431046,
-0.00543781234703487));
#35430=CARTESIAN_POINT('Ctrl Pts',(-0.232451012812611,-0.00081387929148324,
-0.00452569208957409));
#35431=CARTESIAN_POINT('Ctrl Pts',(-0.231652435772805,-0.0010415287758554,
-0.00357419097857274));
#35432=CARTESIAN_POINT('Ctrl Pts',(-0.230843549351773,-0.00111911643714708,
-0.00261050683581516));
#35433=CARTESIAN_POINT('',(-0.230843542065975,-0.00111812869478135,0.00261043842873682));
#35434=CARTESIAN_POINT('Origin',(-0.23396693400794,-0.000859278972356703,
-2.03117108132922E-10));
#35435=CARTESIAN_POINT('Ctrl Pts',(-0.230843549407105,-0.0011191166041277,
0.0026105070108692));
#35436=CARTESIAN_POINT('Ctrl Pts',(-0.231651983097731,-0.00104157341320291,
0.00357365206993173));
#35437=CARTESIAN_POINT('Ctrl Pts',(-0.232444276388805,-0.000816181869474475,
0.0045176677295523));
#35438=CARTESIAN_POINT('Ctrl Pts',(-0.233207649052068,-0.000431751373454661,
0.00542716208151464));
#35439=CARTESIAN_POINT('Ctrl Pts',(-0.233971022757487,-4.73203526106414E-5,
0.00633665767511794));
#35440=CARTESIAN_POINT('Ctrl Pts',(-0.23470551192207,0.00049606094558371,
0.0072116730703037));
#35441=CARTESIAN_POINT('Ctrl Pts',(-0.235365772451735,0.00121957511810953,
0.00799823141159865));
#35442=CARTESIAN_POINT('Ctrl Pts',(-0.23536783372932,0.00122183386822287,
0.00800068698027997));
#35443=CARTESIAN_POINT('Ctrl Pts',(-0.235369894282823,0.00122409437235532,
0.00800314168365631));
#35444=CARTESIAN_POINT('Ctrl Pts',(-0.235371954110837,0.00122635663116605,
0.00800559552008976));
#35445=CARTESIAN_POINT('Ctrl Pts',(-0.235699792387272,0.00158641340486399,
0.00839614342080721));
#35446=CARTESIAN_POINT('Ctrl Pts',(-0.236009259211335,0.00199091601206364,
0.0087647430201395));
#35447=CARTESIAN_POINT('Ctrl Pts',(-0.236288879915149,0.00243864717211577,
0.00909783876953468));
#35448=CARTESIAN_POINT('Ctrl Pts',(-0.236570257493009,0.00288919145452985,
0.00943302737996994));
#35449=CARTESIAN_POINT('Ctrl Pts',(-0.236821411175091,0.00338351354138113,
0.00973227411776468));
#35450=CARTESIAN_POINT('Ctrl Pts',(-0.237030709359485,0.00392048719339499,
0.00998163270096488));
#35451=CARTESIAN_POINT('Ctrl Pts',(-0.237240007543878,0.00445746084540883,
0.0102309912841651));
#35452=CARTESIAN_POINT('Ctrl Pts',(-0.237407397613687,0.00503714549261125,
0.0104303912055088));
#35453=CARTESIAN_POINT('Ctrl Pts',(-0.237522494588081,0.00563877088560149,
0.0105674977840015));
#35454=CARTESIAN_POINT('Ctrl Pts',(-0.237637591562474,0.00624039627859174,
0.0107046043624942));
#35455=CARTESIAN_POINT('Ctrl Pts',(-0.237700402455248,0.00686393789297539,
0.0107794215577471));
#35456=CARTESIAN_POINT('Ctrl Pts',(-0.237700713436944,0.00748866602213257,
0.010779793575244));
#35457=CARTESIAN_POINT('Ctrl Pts',(-0.237700864903606,0.00779294593887606,
0.0107799747699873));
#35458=CARTESIAN_POINT('Ctrl Pts',(-0.237686190487506,0.00809751515955963,
0.0107624949752251));
#35459=CARTESIAN_POINT('Ctrl Pts',(-0.237657867810474,0.00839975141101414,
0.0107287568273012));
#35460=CARTESIAN_POINT('',(-0.186146181811502,0.00666198522174072,0.00957679076397076));
#35461=CARTESIAN_POINT('Origin',(-0.187938685420677,0.00749971564796731,
0.000572374571681731));
#35462=CARTESIAN_POINT('',(-0.192201188841356,-0.000241557430167074,0.00554550626187204));
#35463=CARTESIAN_POINT('Ctrl Pts',(-0.186146181811502,0.00666198522174072,
0.00957679076397076));
#35464=CARTESIAN_POINT('Ctrl Pts',(-0.186240918660984,0.00577359340919673,
0.00949869141429598));
#35465=CARTESIAN_POINT('Ctrl Pts',(-0.186729216300464,0.00408141660355003,
0.00909746875116488));
#35466=CARTESIAN_POINT('Ctrl Pts',(-0.188122925906735,0.00204059109517293,
0.00799351103237768));
#35467=CARTESIAN_POINT('Ctrl Pts',(-0.189934445945795,0.000579265164406154,
0.00668849997305698));
#35468=CARTESIAN_POINT('Ctrl Pts',(-0.191383442893151,-3.83064418099935E-5,
0.00585331050437291));
#35469=CARTESIAN_POINT('Ctrl Pts',(-0.192201188668274,-0.000241594090485781,
0.00554556725774743));
#35470=CARTESIAN_POINT('',(-0.215000291561739,-0.000324149940950663,0.00555319305328791));
#35471=CARTESIAN_POINT('Ctrl Pts',(-0.215000291205181,-0.0003242242949523,
0.00555305246006235));
#35472=CARTESIAN_POINT('Ctrl Pts',(-0.213932608980925,-0.000320905181478583,
0.00555269239176458));
#35473=CARTESIAN_POINT('Ctrl Pts',(-0.212894399737908,-0.000317606952698171,
0.00555234073581887));
#35474=CARTESIAN_POINT('Ctrl Pts',(-0.211885533644697,-0.000314338717420239,
0.00555199786657978));
#35475=CARTESIAN_POINT('Ctrl Pts',(-0.210876667461984,-0.000311070481852365,
0.00555165499731028));
#35476=CARTESIAN_POINT('Ctrl Pts',(-0.209897144434309,-0.000307832227897103,
0.00555132091066889));
#35477=CARTESIAN_POINT('Ctrl Pts',(-0.208947353979719,-0.000304634161730677,
0.00555099707706335));
#35478=CARTESIAN_POINT('Ctrl Pts',(-0.208472458752424,-0.000303035128647463,
0.00555083516026057));
#35479=CARTESIAN_POINT('Ctrl Pts',(-0.208004996668339,-0.000301446149282922,
0.00555067581488556));
#35480=CARTESIAN_POINT('Ctrl Pts',(-0.207544480927504,-0.000299866555274974,
0.00555051916679648));
#35481=CARTESIAN_POINT('Ctrl Pts',(-0.207083965186669,-0.000298286961267027,
0.00555036251870738));
#35482=CARTESIAN_POINT('Ctrl Pts',(-0.206630395789221,-0.000296716714222072,
0.0055502085465108));
#35483=CARTESIAN_POINT('Ctrl Pts',(-0.206185752375027,-0.000295163842050715,
0.00555005809144));
#35484=CARTESIAN_POINT('Ctrl Pts',(-0.205741108960833,-0.000293610969879358,
0.0055499076363692));
#35485=CARTESIAN_POINT('Ctrl Pts',(-0.205305391529366,-0.000292075614881537,
0.00554976078032587));
#35486=CARTESIAN_POINT('Ctrl Pts',(-0.204871168306577,-0.000290532039648846,
0.00554961555720526));
#35487=CARTESIAN_POINT('Ctrl Pts',(-0.204654056695182,-0.0002897602520325,
0.00554954294564495));
#35488=CARTESIAN_POINT('Ctrl Pts',(-0.204437318636325,-0.000288986311853899,
0.00554947068530159));
#35489=CARTESIAN_POINT('Ctrl Pts',(-0.20423043044895,-0.000288244541876076,
0.00554940183661774));
#35490=CARTESIAN_POINT('Ctrl Pts',(-0.204023542261574,-0.000287502771898252,
0.00554933298793389));
#35491=CARTESIAN_POINT('Ctrl Pts',(-0.203826503944328,-0.000286793520252714,
0.00554926775793827));
#35492=CARTESIAN_POINT('Ctrl Pts',(-0.203600728706342,-0.00028597691500919,
0.00554919348805181));
#35493=CARTESIAN_POINT('Ctrl Pts',(-0.203374953468356,-0.000285160309765666,
0.00554911921816535));
#35494=CARTESIAN_POINT('Ctrl Pts',(-0.20312044131193,-0.00028423576377125,
0.00554903555688988));
#35495=CARTESIAN_POINT('Ctrl Pts',(-0.202874057457924,-0.000283336172872535,
0.00554895461009971));
#35496=CARTESIAN_POINT('Ctrl Pts',(-0.202627673603918,-0.000282436581973819,
0.00554887366330954));
#35497=CARTESIAN_POINT('Ctrl Pts',(-0.202389418050814,-0.000281562329560916,
0.00554879566253169));
#35498=CARTESIAN_POINT('Ctrl Pts',(-0.202150286345955,-0.000280680803074264,
0.0055487175181587));
#35499=CARTESIAN_POINT('Ctrl Pts',(-0.201672022936239,-0.000278917750100961,
0.00554856122941273));
#35500=CARTESIAN_POINT('Ctrl Pts',(-0.201190254921159,-0.000277125193128902,
0.00554840411650478));
#35501=CARTESIAN_POINT('Ctrl Pts',(-0.200711444532909,-0.000275326860415499,
0.00554824832785496));
#35502=CARTESIAN_POINT('Ctrl Pts',(-0.199753823756409,-0.00027173019498869,
0.00554793675055534));
#35503=CARTESIAN_POINT('Ctrl Pts',(-0.198808033484689,-0.000268111032540832,
0.00554763085059868));
#35504=CARTESIAN_POINT('Ctrl Pts',(-0.197868562559789,-0.000264450677025733,
0.00554732800782794));
#35505=CARTESIAN_POINT('Ctrl Pts',(-0.196929091634889,-0.000260790321510633,
0.00554702516505721));
#35506=CARTESIAN_POINT('Ctrl Pts',(-0.195995940054903,-0.0002570891780411,
0.00554672565571742));
#35507=CARTESIAN_POINT('Ctrl Pts',(-0.195051666862503,-0.000253275770992353,
0.00554642287911516));
#35508=CARTESIAN_POINT('Ctrl Pts',(-0.194107393750835,-0.000249462364269639,
0.00554612010253878));
#35509=CARTESIAN_POINT('Ctrl Pts',(-0.193151999033877,-0.000245535583896571,
0.00554581330127274));
#35510=CARTESIAN_POINT('Ctrl Pts',(-0.192201188841356,-0.000241557430167074,
0.00554550626187204));
#35511=CARTESIAN_POINT('',(-0.21500029174882,-0.000324094014707694,-0.00555316364009558));
#35512=CARTESIAN_POINT('Ctrl Pts',(-0.215000291561739,-0.000324149940950663,
0.00555319305328791));
#35513=CARTESIAN_POINT('Ctrl Pts',(-0.215668740091759,-0.000326228214530295,
0.00555341885793155));
#35514=CARTESIAN_POINT('Ctrl Pts',(-0.216324728842753,-0.000393731830372502,
0.00543467425660531));
#35515=CARTESIAN_POINT('Ctrl Pts',(-0.216937359547008,-0.000498389548785778,
0.00521197222380067));
#35516=CARTESIAN_POINT('Ctrl Pts',(-0.217007385782656,-0.000510352360967931,
0.00518651645588009));
#35517=CARTESIAN_POINT('Ctrl Pts',(-0.217076845515466,-0.000522776977352358,
0.00515969404947732));
#35518=CARTESIAN_POINT('Ctrl Pts',(-0.217145692593967,-0.000535604694262252,
0.00513152356702724));
#35519=CARTESIAN_POINT('Ctrl Pts',(-0.217816854468214,-0.000660656834613602,
0.00485690111083667));
#35520=CARTESIAN_POINT('Ctrl Pts',(-0.218429805272727,-0.000824611483592641,
0.00445372704704561));
#35521=CARTESIAN_POINT('Ctrl Pts',(-0.218946402817707,-0.000965073719826547,
0.00394589026024182));
#35522=CARTESIAN_POINT('Ctrl Pts',(-0.21911757141393,-0.00101161425032699,
0.00377762443948319));
#35523=CARTESIAN_POINT('Ctrl Pts',(-0.219278158884941,-0.00105556042755966,
0.00359780043100863));
#35524=CARTESIAN_POINT('Ctrl Pts',(-0.219426704704914,-0.00109449434193882,
0.00340810662225617));
#35525=CARTESIAN_POINT('Ctrl Pts',(-0.219502319179551,-0.00111431292371979,
0.00331154653262599));
#35526=CARTESIAN_POINT('Ctrl Pts',(-0.219574813505332,-0.00113283089738519,
0.00321243800056172));
#35527=CARTESIAN_POINT('Ctrl Pts',(-0.219643995497907,-0.00114993043982612,
0.00311087728876615));
#35528=CARTESIAN_POINT('Ctrl Pts',(-0.219784412586894,-0.0011846369853185,
0.00290474186284185));
#35529=CARTESIAN_POINT('Ctrl Pts',(-0.219911192740882,-0.00121336031308103,
0.00268891197041315));
#35530=CARTESIAN_POINT('Ctrl Pts',(-0.220022736935838,-0.00123594984514704,
0.00246439654593185));
#35531=CARTESIAN_POINT('Ctrl Pts',(-0.220074112524313,-0.00124635424587568,
0.00236098809819431));
#35532=CARTESIAN_POINT('Ctrl Pts',(-0.220122255964863,-0.00125547047269016,
0.00225573024477926));
#35533=CARTESIAN_POINT('Ctrl Pts',(-0.220167013742202,-0.00126354003322303,
0.00214910011923536));
#35534=CARTESIAN_POINT('Ctrl Pts',(-0.220255304274326,-0.00127945829002233,
0.00193875833989861));
#35535=CARTESIAN_POINT('Ctrl Pts',(-0.220330419857194,-0.00129139212065717,
0.00172100899924843));
#35536=CARTESIAN_POINT('Ctrl Pts',(-0.220392020117299,-0.00130178661929758,
0.00150014969597866));
#35537=CARTESIAN_POINT('Ctrl Pts',(-0.220528474000989,-0.00132481200435377,
0.00101091296826799));
#35538=CARTESIAN_POINT('Ctrl Pts',(-0.220598617810777,-0.001340773537683,
0.000507277145745172));
#35539=CARTESIAN_POINT('Ctrl Pts',(-0.220598427190772,-0.00134207975133048,
-7.52537007378193E-7));
#35540=CARTESIAN_POINT('Ctrl Pts',(-0.220598376879732,-0.00134242450511075,
-0.000134838682836322));
#35541=CARTESIAN_POINT('Ctrl Pts',(-0.22059342260227,-0.00134174640947658,
-0.000268914120462707));
#35542=CARTESIAN_POINT('Ctrl Pts',(-0.220583640920972,-0.00133993652035355,
-0.000402703728332918));
#35543=CARTESIAN_POINT('Ctrl Pts',(-0.220560148143331,-0.0013355896886151,
-0.000724027784246587));
#35544=CARTESIAN_POINT('Ctrl Pts',(-0.22050881067424,-0.00132468740862665,
-0.00104372328931524));
#35545=CARTESIAN_POINT('Ctrl Pts',(-0.22043068209847,-0.00130920789017929,
-0.00135493667140239));
#35546=CARTESIAN_POINT('Ctrl Pts',(-0.220390026640352,-0.00130115287435809,
-0.00151688154875802));
#35547=CARTESIAN_POINT('Ctrl Pts',(-0.220342116549357,-0.00129187744466456,
-0.00167656205544119));
#35548=CARTESIAN_POINT('Ctrl Pts',(-0.220287103460061,-0.00128219907898819,
-0.00183469943029004));
#35549=CARTESIAN_POINT('Ctrl Pts',(-0.220249785986982,-0.00127563387504865,
-0.00194197003268941));
#35550=CARTESIAN_POINT('Ctrl Pts',(-0.220209199956055,-0.00126886559305341,
-0.00204849177962379));
#35551=CARTESIAN_POINT('Ctrl Pts',(-0.220165384850271,-0.00126128757747624,
-0.00215277905196633));
#35552=CARTESIAN_POINT('Ctrl Pts',(-0.220141806611008,-0.0012572096171193,
-0.00220889920083847));
#35553=CARTESIAN_POINT('Ctrl Pts',(-0.22011729288104,-0.00125287335201092,
-0.00226472495715461));
#35554=CARTESIAN_POINT('Ctrl Pts',(-0.22009186434136,-0.0012481906745658,
-0.0023200354792529));
#35555=CARTESIAN_POINT('Ctrl Pts',(-0.219964032067859,-0.00122465030176397,
-0.00259808800909705));
#35556=CARTESIAN_POINT('Ctrl Pts',(-0.219813080791229,-0.00119207341516924,
-0.00286323534620003));
#35557=CARTESIAN_POINT('Ctrl Pts',(-0.219641753502741,-0.00114977266145016,
-0.00311424190666308));
#35558=CARTESIAN_POINT('Ctrl Pts',(-0.219606803653757,-0.00114114353431307,
-0.00316544590025774));
#35559=CARTESIAN_POINT('Ctrl Pts',(-0.219571005532134,-0.00113213027555365,
-0.00321601272097191));
#35560=CARTESIAN_POINT('Ctrl Pts',(-0.21953438720127,-0.0011227418846443,
-0.00326596039771834));
#35561=CARTESIAN_POINT('Ctrl Pts',(-0.219355791593764,-0.00107695264907934,
-0.00350956614001746));
#35562=CARTESIAN_POINT('Ctrl Pts',(-0.219157685440798,-0.00102227590413239,
-0.00373830700747762));
#35563=CARTESIAN_POINT('Ctrl Pts',(-0.218943331186757,-0.000963766372682074,
-0.00394877174088596));
#35564=CARTESIAN_POINT('Ctrl Pts',(-0.218858026839138,-0.000940481939012855,
-0.00403252821616926));
#35565=CARTESIAN_POINT('Ctrl Pts',(-0.218770149734348,-0.000916567399260997,
-0.00411347430382928));
#35566=CARTESIAN_POINT('Ctrl Pts',(-0.218679855692286,-0.000892327992985571,
-0.00419142830140832));
#35567=CARTESIAN_POINT('Ctrl Pts',(-0.218223323108185,-0.000769771969006836,
-0.00458556881326656));
#35568=CARTESIAN_POINT('Ctrl Pts',(-0.217705003690594,-0.000639141842020944,
-0.00490281622798988));
#35569=CARTESIAN_POINT('Ctrl Pts',(-0.21714503543376,-0.000535117611044864,
-0.00513162917727141));
#35570=CARTESIAN_POINT('Ctrl Pts',(-0.216474315446649,-0.00041051924317671,
-0.00540569724545193));
#35571=CARTESIAN_POINT('Ctrl Pts',(-0.215743833588139,-0.000326403425118811,
-0.00555341379930925));
#35572=CARTESIAN_POINT('Ctrl Pts',(-0.21500029174882,-0.000324094014707694,
-0.00555316364009558));
#35573=CARTESIAN_POINT('',(-0.192201191756381,-0.000241534711908781,-0.00554549092202007));
#35574=CARTESIAN_POINT('Ctrl Pts',(-0.192201191756381,-0.000241534711908781,
-0.00554549092202007));
#35575=CARTESIAN_POINT('Ctrl Pts',(-0.192678594805748,-0.000243532238599143,
-0.00554564514895133));
#35576=CARTESIAN_POINT('Ctrl Pts',(-0.193156777591037,-0.000245515257083601,
-0.00554579917339835));
#35577=CARTESIAN_POINT('Ctrl Pts',(-0.193630540727713,-0.000247462867484684,
-0.00554595129683631));
#35578=CARTESIAN_POINT('Ctrl Pts',(-0.194104303945115,-0.000249410478217631,
-0.0055461034203002));
#35579=CARTESIAN_POINT('Ctrl Pts',(-0.194573647510702,-0.000251323030553919,
-0.00554625388646444));
#35580=CARTESIAN_POINT('Ctrl Pts',(-0.195054169579703,-0.000253263283285137,
-0.00554640817237499));
#35581=CARTESIAN_POINT('Ctrl Pts',(-0.195294430614203,-0.000254233409650747,
-0.00554648531533026));
#35582=CARTESIAN_POINT('Ctrl Pts',(-0.195537486275633,-0.000255210231968368,
-0.00554656325712504));
#35583=CARTESIAN_POINT('Ctrl Pts',(-0.195763838864246,-0.000256116093067966,
-0.00554663583769404));
#35584=CARTESIAN_POINT('Ctrl Pts',(-0.195990191452859,-0.000257021954167565,
-0.00554670841826303));
#35585=CARTESIAN_POINT('Ctrl Pts',(-0.19619984096725,-0.000257857156228515,
-0.0055467758417085));
#35586=CARTESIAN_POINT('Ctrl Pts',(-0.196410720680054,-0.000258693884580058,
-0.00554684397646886));
#35587=CARTESIAN_POINT('Ctrl Pts',(-0.196832480105662,-0.000260367341283143,
-0.00554698024598957));
#35588=CARTESIAN_POINT('Ctrl Pts',(-0.197259160327546,-0.00026204633453472,
-0.00554711897819944));
#35589=CARTESIAN_POINT('Ctrl Pts',(-0.197689895515706,-0.000263726856300013,
-0.00554725977781399));
#35590=CARTESIAN_POINT('Ctrl Pts',(-0.198551365892026,-0.000267087899830605,
-0.00554754137704308));
#35591=CARTESIAN_POINT('Ctrl Pts',(-0.199429056133176,-0.00027045513768323,
-0.00554783128850645));
#35592=CARTESIAN_POINT('Ctrl Pts',(-0.200323641208812,-0.000273827273659161,
-0.00554812814068451));
#35593=CARTESIAN_POINT('Ctrl Pts',(-0.201218226284448,-0.000277199409635091,
-0.00554842499286257));
#35594=CARTESIAN_POINT('Ctrl Pts',(-0.202129706194687,-0.000280576415406435,
-0.00554872876800488));
#35595=CARTESIAN_POINT('Ctrl Pts',(-0.203057914973526,-0.000283953370692891,
-0.00554903828929629));
#35596=CARTESIAN_POINT('Ctrl Pts',(-0.204914332531203,-0.0002907072812658,
-0.00554965733187913));
#35597=CARTESIAN_POINT('Ctrl Pts',(-0.206837665564307,-0.000297461032084291,
-0.00555029923894105));
#35598=CARTESIAN_POINT('Ctrl Pts',(-0.208828046911259,-0.000304177112489735,
-0.00555096192484518));
#35599=CARTESIAN_POINT('Ctrl Pts',(-0.210818428167034,-0.000310893192587523,
-0.00555162461071896));
#35600=CARTESIAN_POINT('Ctrl Pts',(-0.212875857730999,-0.000317571487539541,
-0.00555230799325907));
#35601=CARTESIAN_POINT('Ctrl Pts',(-0.215000291390742,-0.000324168998365841,
-0.0055530216284886));
#35602=CARTESIAN_POINT('',(-0.186146181862621,0.00666198473330996,-0.00957679047534686));
#35603=CARTESIAN_POINT('Ctrl Pts',(-0.192201191480734,-0.000241594683462822,
-0.00554556743215708));
#35604=CARTESIAN_POINT('Ctrl Pts',(-0.191385432420279,-3.88012107838058E-5,
-0.005852563916371));
#35605=CARTESIAN_POINT('Ctrl Pts',(-0.18992436359119,0.000584077259331637,
-0.00669447323493867));
#35606=CARTESIAN_POINT('Ctrl Pts',(-0.188118589959122,0.00204642926269473,
-0.00799717565551262));
#35607=CARTESIAN_POINT('Ctrl Pts',(-0.186728499584069,0.00408398932516683,
-0.0090979910428183));
#35608=CARTESIAN_POINT('Ctrl Pts',(-0.186240928632579,0.00577350042675652,
-0.00949868268458664));
#35609=CARTESIAN_POINT('Ctrl Pts',(-0.186146181862621,0.00666198473330996,
-0.00957679047534686));
#35610=CARTESIAN_POINT('',(-0.186146181862621,0.0083380152666897,-0.00957679047534678));
#35611=CARTESIAN_POINT('Origin',(-0.187904819949368,0.00750020158743468,
-0.000565738065293699));
#35612=CARTESIAN_POINT('',(-0.192201191653566,0.0152415580820476,-0.00554550644721905));
#35613=CARTESIAN_POINT('Ctrl Pts',(-0.186146181862621,0.0083380152666897,
-0.00957679047534678));
#35614=CARTESIAN_POINT('Ctrl Pts',(-0.186240918786417,0.00922640724122356,
-0.00949869080161241));
#35615=CARTESIAN_POINT('Ctrl Pts',(-0.186729216417846,0.0109185839275611,
-0.00909746664888909));
#35616=CARTESIAN_POINT('Ctrl Pts',(-0.18812292744858,0.0129594111220647,
-0.00799351337395886));
#35617=CARTESIAN_POINT('Ctrl Pts',(-0.189934449608939,0.014420736841963,
-0.006688503795585));
#35618=CARTESIAN_POINT('Ctrl Pts',(-0.191383445765099,0.0150383073386066,
-0.00585331155888567));
#35619=CARTESIAN_POINT('Ctrl Pts',(-0.192201191480731,0.0152415946834622,
-0.00554556743215712));
#35620=CARTESIAN_POINT('',(-0.215000291562328,0.0153241509688053,-0.00555319360107524));
#35621=CARTESIAN_POINT('Ctrl Pts',(-0.215000291205702,0.0153242253442285,
-0.00555305296541064));
#35622=CARTESIAN_POINT('Ctrl Pts',(-0.213932597704458,0.0153209061962902,
-0.00555269287857503));
#35623=CARTESIAN_POINT('Ctrl Pts',(-0.212894379313026,0.0153176079358162,
-0.00555234120479523));
#35624=CARTESIAN_POINT('Ctrl Pts',(-0.211885508359842,0.0153143396802069,
-0.00555199831893506));
#35625=CARTESIAN_POINT('Ctrl Pts',(-0.210876637317151,0.0153110714243076,
-0.00555165543304446));
#35626=CARTESIAN_POINT('Ctrl Pts',(-0.209897113717939,0.0153078331616761,
-0.00555132133114625));
#35627=CARTESIAN_POINT('Ctrl Pts',(-0.208947320500622,0.0153046350773028,
-0.00555099748235955));
#35628=CARTESIAN_POINT('Ctrl Pts',(-0.208472423891963,0.0153030360351161,
-0.0055508355579662));
#35629=CARTESIAN_POINT('Ctrl Pts',(-0.208004959878718,0.0153014470440823,
-0.00555067620492078));
#35630=CARTESIAN_POINT('Ctrl Pts',(-0.207544449760479,0.0152998674643782,
-0.00555051955126661));
#35631=CARTESIAN_POINT('Ctrl Pts',(-0.207083939642239,0.0152982878846741,
-0.00555036289761244));
#35632=CARTESIAN_POINT('Ctrl Pts',(-0.206630383419139,0.0152967176785448,
-0.00555020892231339));
#35633=CARTESIAN_POINT('Ctrl Pts',(-0.206185727792834,0.0152951647572964,
-0.00555005845722071));
#35634=CARTESIAN_POINT('Ctrl Pts',(-0.20574107216653,0.0152936118360481,
-0.00554990799212803));
#35635=CARTESIAN_POINT('Ctrl Pts',(-0.205305317136504,0.0152920763396207,
-0.0055497611177857));
#35636=CARTESIAN_POINT('Ctrl Pts',(-0.204871154582032,0.0152905329744749,
-0.00554961590672052));
#35637=CARTESIAN_POINT('Ctrl Pts',(-0.204654073304796,0.015289761291902,
-0.00554954330118793));
#35638=CARTESIAN_POINT('Ctrl Pts',(-0.204437390146812,0.0152889875462586,
-0.00554947105540806));
#35639=CARTESIAN_POINT('Ctrl Pts',(-0.204230423755464,0.0152882454917763,
-0.00554940217900394));
#35640=CARTESIAN_POINT('Ctrl Pts',(-0.204023457364116,0.0152875034372941,
-0.00554933330259982));
#35641=CARTESIAN_POINT('Ctrl Pts',(-0.203826207738076,0.0152867934163249,
-0.00554926799916205));
#35642=CARTESIAN_POINT('Ctrl Pts',(-0.203600730112181,0.0152859778836302,
-0.00554919382403213));
#35643=CARTESIAN_POINT('Ctrl Pts',(-0.203375252486286,0.0152851623509355,
-0.00554911964890221));
#35644=CARTESIAN_POINT('Ctrl Pts',(-0.203121546862791,0.0152842407307248,
-0.00554903625738765));
#35645=CARTESIAN_POINT('Ctrl Pts',(-0.202875762064915,0.0152833433310473,
-0.00554895552284241));
#35646=CARTESIAN_POINT('Ctrl Pts',(-0.202629977267039,0.0152824459313697,
-0.00554887478829716));
#35647=CARTESIAN_POINT('Ctrl Pts',(-0.202392113293296,0.015281573127183,
-0.0055487969371522));
#35648=CARTESIAN_POINT('Ctrl Pts',(-0.202153351523362,0.0152806929783707,
-0.00554871893697691));
#35649=CARTESIAN_POINT('Ctrl Pts',(-0.201675827983494,0.015278932680746,
-0.00554856293662631));
#35650=CARTESIAN_POINT('Ctrl Pts',(-0.201194713260464,0.0152771426083813,
-0.00554840609743424));
#35651=CARTESIAN_POINT('Ctrl Pts',(-0.200716202959138,0.0152753454496153,
-0.00554825048440849));
#35652=CARTESIAN_POINT('Ctrl Pts',(-0.199759182356486,0.0152717511320833,
-0.005547939258357));
#35653=CARTESIAN_POINT('Ctrl Pts',(-0.198812579438422,0.0152681289979275,
-0.00554763326914996));
#35654=CARTESIAN_POINT('Ctrl Pts',(-0.197872595918786,0.0152644669040492,
-0.005547330085655));
#35655=CARTESIAN_POINT('Ctrl Pts',(-0.19693261239915,0.0152608048101709,
-0.00554702690216004));
#35656=CARTESIAN_POINT('Ctrl Pts',(-0.195999248275822,0.015257103211607,
-0.00554672683230568));
#35657=CARTESIAN_POINT('Ctrl Pts',(-0.195055360270019,0.0152532915881122,
-0.0055464240380698));
#35658=CARTESIAN_POINT('Ctrl Pts',(-0.194111472344545,0.0152494799649418,
-0.00554612124385969));
#35659=CARTESIAN_POINT('Ctrl Pts',(-0.193157060542462,0.0152455574395132,
-0.00554581513217478));
#35660=CARTESIAN_POINT('Ctrl Pts',(-0.192201191653566,0.0152415580820476,
-0.00554550644721905));
#35661=CARTESIAN_POINT('Ctrl Pts',(-0.215000291562328,0.0153241509688053,
-0.00555319360107524));
#35662=CARTESIAN_POINT('Ctrl Pts',(-0.215668740328172,0.0153262292429902,
-0.00555341941485916));
#35663=CARTESIAN_POINT('Ctrl Pts',(-0.216324729447901,0.0153937319339566,
-0.00543467464259903));
#35664=CARTESIAN_POINT('Ctrl Pts',(-0.216937360421232,0.0154983886920181,
-0.00521197223979806));
#35665=CARTESIAN_POINT('Ctrl Pts',(-0.217007386432887,0.0155103513509086,
-0.00518651652219178));
#35666=CARTESIAN_POINT('Ctrl Pts',(-0.217076845944537,0.0155227758123586,
-0.00515969417359937));
#35667=CARTESIAN_POINT('Ctrl Pts',(-0.217145692804874,0.0155356033754558,
-0.00513152375635335));
#35668=CARTESIAN_POINT('Ctrl Pts',(-0.217816854743512,0.015660654424613,
-0.00485690103923239));
#35669=CARTESIAN_POINT('Ctrl Pts',(-0.21842980551494,0.0158246085287311,
-0.00445372675993447));
#35670=CARTESIAN_POINT('Ctrl Pts',(-0.218946402952426,0.0159650714808781,
-0.00394588998612724));
#35671=CARTESIAN_POINT('Ctrl Pts',(-0.219117571675436,0.0160116122927455,
-0.00377762401002606));
#35672=CARTESIAN_POINT('Ctrl Pts',(-0.2192781592448,0.0160555588565627,
-0.00359779983207659));
#35673=CARTESIAN_POINT('Ctrl Pts',(-0.219426705149579,0.0160944931464038,
-0.00340810586555922));
#35674=CARTESIAN_POINT('Ctrl Pts',(-0.219502319454705,0.0161143118635625,
-0.00331154596721636));
#35675=CARTESIAN_POINT('Ctrl Pts',(-0.219574813625008,0.0161328299754327,
-0.00321243764433068));
#35676=CARTESIAN_POINT('Ctrl Pts',(-0.219643995479742,0.0161499296503641,
-0.00311087714745257));
#35677=CARTESIAN_POINT('Ctrl Pts',(-0.219784412581996,0.0161846365371998,
-0.00290474172755338));
#35678=CARTESIAN_POINT('Ctrl Pts',(-0.219911192765131,0.0162133601522874,
-0.00268891185321829));
#35679=CARTESIAN_POINT('Ctrl Pts',(-0.220022736985533,0.0162359498238763,
-0.0024643964070149));
#35680=CARTESIAN_POINT('Ctrl Pts',(-0.220074112549396,0.0162463542815091,
-0.00236098802240206));
#35681=CARTESIAN_POINT('Ctrl Pts',(-0.220122255969117,0.0162554705354734,
-0.00225573022547248));
#35682=CARTESIAN_POINT('Ctrl Pts',(-0.220167013727973,0.0162635401033155,
-0.00214910016136067));
#35683=CARTESIAN_POINT('Ctrl Pts',(-0.220255304272581,0.0162794583833577,
-0.00193875838660007));
#35684=CARTESIAN_POINT('Ctrl Pts',(-0.220330419862705,0.0162913921573094,
-0.00172100901754344));
#35685=CARTESIAN_POINT('Ctrl Pts',(-0.220392020126769,0.0163017866191688,
-0.00150014969593761));
#35686=CARTESIAN_POINT('Ctrl Pts',(-0.220528474005327,0.0163248119204041,
-0.00101091297744705));
#35687=CARTESIAN_POINT('Ctrl Pts',(-0.22059861780742,0.0163407734893559,
-0.000507277223307716));
#35688=CARTESIAN_POINT('Ctrl Pts',(-0.220598427190516,0.0163420797339417,
7.52423205390498E-7));
#35689=CARTESIAN_POINT('Ctrl Pts',(-0.220598376880276,0.0163424244960112,
0.000134838607512327));
#35690=CARTESIAN_POINT('Ctrl Pts',(-0.220593422600694,0.0163417464071427,
0.000268914083012791));
#35691=CARTESIAN_POINT('Ctrl Pts',(-0.220583640914636,0.016339936520452,
0.000402703728358851));
#35692=CARTESIAN_POINT('Ctrl Pts',(-0.220560148132489,0.0163355896958366,
0.000724027779571594));
#35693=CARTESIAN_POINT('Ctrl Pts',(-0.220508810660082,0.0163246874026146,
0.0010437232789448));
#35694=CARTESIAN_POINT('Ctrl Pts',(-0.220430682085685,0.0163092078903576,
0.00135493667144938));
#35695=CARTESIAN_POINT('Ctrl Pts',(-0.220390026628729,0.0163011528778462,
0.00151688155244445));
#35696=CARTESIAN_POINT('Ctrl Pts',(-0.220342116540319,0.0162918774559878,
0.00167656206656788));
#35697=CARTESIAN_POINT('Ctrl Pts',(-0.220287103455273,0.016282199079049,
0.00183469943034553));
#35698=CARTESIAN_POINT('Ctrl Pts',(-0.220249786004752,0.0162756338709311,
0.00194196996868066));
#35699=CARTESIAN_POINT('Ctrl Pts',(-0.220209200000601,0.0162688655768999,
0.00204849164457503));
#35700=CARTESIAN_POINT('Ctrl Pts',(-0.220165384926114,0.0162612875677296,
0.0021527788685016));
#35701=CARTESIAN_POINT('Ctrl Pts',(-0.220141806666224,0.01625720960434,
0.00220889908050186));
#35702=CARTESIAN_POINT('Ctrl Pts',(-0.22011729291399,0.0162528733413081,
0.00226472489623903));
#35703=CARTESIAN_POINT('Ctrl Pts',(-0.220091864350141,0.0162481906744713,
0.00232003547938548));
#35704=CARTESIAN_POINT('Origin',(-0.206561433685686,0.00750002637574172,
0.0135355039474176));
#35705=CARTESIAN_POINT('',(-0.186019881459752,0.00692134436047904,0.00979684421662477));
#35706=CARTESIAN_POINT('Ctrl Pts',(-0.185999364351512,0.00749999962802277,
0.00991138348445803));
#35707=CARTESIAN_POINT('Ctrl Pts',(-0.185999376571189,0.00730961846353397,
0.00991131415321303));
#35708=CARTESIAN_POINT('Ctrl Pts',(-0.186006003246306,0.00711673337435274,
0.00987309615363802));
#35709=CARTESIAN_POINT('Ctrl Pts',(-0.186019881459752,0.00692134436047904,
0.00979684421662477));
#35710=CARTESIAN_POINT('',(-0.186041755315114,0.0066688778475149,0.00967860489999109));
#35711=CARTESIAN_POINT('Ctrl Pts',(-0.186019884049452,0.00692131183731184,
0.00979683157756966));
#35712=CARTESIAN_POINT('Ctrl Pts',(-0.186026050535138,0.00683448131744766,
0.00976295078830858));
#35713=CARTESIAN_POINT('Ctrl Pts',(-0.186033396723478,0.00675056489938151,
0.0097230652955223));
#35714=CARTESIAN_POINT('Ctrl Pts',(-0.186041751476459,0.00666887311730628,
0.00967861576317704));
#35715=CARTESIAN_POINT('',(-0.186045756633599,0.00664877182750347,0.00965739225385244));
#35716=CARTESIAN_POINT('Ctrl Pts',(-0.186045750694262,0.00664885008080394,
0.00965739927776235));
#35717=CARTESIAN_POINT('Ctrl Pts',(-0.186045567569101,0.0066487514075171,
0.00965836803390889));
#35718=CARTESIAN_POINT('Ctrl Pts',(-0.186045385816378,0.00664882388039244,
0.00965932990672161));
#35719=CARTESIAN_POINT('Ctrl Pts',(-0.18604500765403,0.00664928351164828,
0.00966133197577962));
#35720=CARTESIAN_POINT('Ctrl Pts',(-0.186044817391655,0.0066496963288531,
0.00966233970967473));
#35721=CARTESIAN_POINT('Ctrl Pts',(-0.18604420014009,0.00665147479437923,
0.00966561019654977));
#35722=CARTESIAN_POINT('Ctrl Pts',(-0.186043801299601,0.00665343241809817,
0.00966772565168096));
#35723=CARTESIAN_POINT('Ctrl Pts',(-0.186042813488648,0.00665927890134443,
0.00967296823442883));
#35724=CARTESIAN_POINT('Ctrl Pts',(-0.186042225851779,0.00666431391360417,
0.0096760919773268));
#35725=CARTESIAN_POINT('Ctrl Pts',(-0.186041756611168,0.00666888632110605,
0.00967858844524271));
#35726=CARTESIAN_POINT('',(-0.18604575186606,0.00835120658339954,0.0096573930787881));
#35727=CARTESIAN_POINT('Ctrl Pts',(-0.186045752236316,0.00664877185494917,
0.00965739112009325));
#35728=CARTESIAN_POINT('Ctrl Pts',(-0.18603600739274,0.00721625009776599,
0.00970894240247701));
#35729=CARTESIAN_POINT('Ctrl Pts',(-0.186036007269321,0.00778372834058278,
0.00970894305537529));
#35730=CARTESIAN_POINT('Ctrl Pts',(-0.18604575186606,0.00835120658339954,
0.0096573930787881));
#35731=CARTESIAN_POINT('',(-0.186041751490874,0.00833112702364014,0.00967861612727941));
#35732=CARTESIAN_POINT('Ctrl Pts',(-0.186045750325906,0.00835112529557688,
0.0096574012264128));
#35733=CARTESIAN_POINT('Ctrl Pts',(-0.186045605429111,0.00835120318317337,
0.00965816774988358));
#35734=CARTESIAN_POINT('Ctrl Pts',(-0.186045460789224,0.00835117430982953,
0.00965893315000607));
#35735=CARTESIAN_POINT('Ctrl Pts',(-0.186045151109668,0.00835090412616134,
0.00966057240088015));
#35736=CARTESIAN_POINT('Ctrl Pts',(-0.186044990615733,0.0083506354811343,
0.00966142226520882));
#35737=CARTESIAN_POINT('Ctrl Pts',(-0.186044474171132,0.00834944013196887,
0.00966415786011833));
#35738=CARTESIAN_POINT('Ctrl Pts',(-0.18604414023323,0.00834809736249489,
0.00966592822660773));
#35739=CARTESIAN_POINT('Ctrl Pts',(-0.186043057962283,0.0083427181772925,
0.00967166900991584));
#35740=CARTESIAN_POINT('Ctrl Pts',(-0.186042338516759,0.00833676576308223,
0.00967549257825685));
#35741=CARTESIAN_POINT('Ctrl Pts',(-0.186041757634892,0.00833110922485847,
0.00967858299879916));
#35742=CARTESIAN_POINT('',(-0.186019881459749,0.0080786556394931,0.00979684421664208));
#35743=CARTESIAN_POINT('Ctrl Pts',(-0.186041751450861,0.00833112702364026,
0.00967861611975897));
#35744=CARTESIAN_POINT('Ctrl Pts',(-0.186033396707417,0.00824943534841117,
0.00972306560553079));
#35745=CARTESIAN_POINT('Ctrl Pts',(-0.186026050708484,0.00816551734876726,
0.00976294827134343));
#35746=CARTESIAN_POINT('Ctrl Pts',(-0.186019884249235,0.00807868703243332,
0.00979682889022281));
#35747=CARTESIAN_POINT('Ctrl Pts',(-0.186019881459749,0.0080786556394931,
0.00979684421664208));
#35748=CARTESIAN_POINT('Ctrl Pts',(-0.18600600325118,0.00788326669427363,
0.00987309612685917));
#35749=CARTESIAN_POINT('Ctrl Pts',(-0.185999376576045,0.00769038148190397,
0.00991131412647235));
#35750=CARTESIAN_POINT('Ctrl Pts',(-0.185999364351488,0.00750000000238413,
0.00991138348459431));
#35751=CARTESIAN_POINT('Origin',(-0.215,-0.00247776328493882,0.));
#35752=CARTESIAN_POINT('',(-0.217717620464915,-0.000864182492545611,-0.00478156822519172));
#35753=CARTESIAN_POINT('Ctrl Pts',(-0.215000000001386,-0.000525628313080397,
0.0055));
#35754=CARTESIAN_POINT('Ctrl Pts',(-0.215733657093434,-0.000527918025936895,
0.0055));
#35755=CARTESIAN_POINT('Ctrl Pts',(-0.216453796216893,-0.000613506209613022,
0.00535197579258614));
#35756=CARTESIAN_POINT('Ctrl Pts',(-0.217113615428784,-0.000737496304503929,
0.00507765997808475));
#35757=CARTESIAN_POINT('Ctrl Pts',(-0.217773434640674,-0.000861486399394835,
0.00480334416358336));
#35758=CARTESIAN_POINT('Ctrl Pts',(-0.218372957928401,-0.00102387445685327,
0.00440280379788875));
#35759=CARTESIAN_POINT('Ctrl Pts',(-0.218878851239864,-0.00116524793995074,
0.00389929670329421));
#35760=CARTESIAN_POINT('Ctrl Pts',(-0.219131797895595,-0.00123593468149947,
0.00364754315599693));
#35761=CARTESIAN_POINT('Ctrl Pts',(-0.219361326626901,-0.0013013686722475,
0.00337004060674126));
#35762=CARTESIAN_POINT('Ctrl Pts',(-0.219562216703885,-0.00135080819197357,
0.00307183602795968));
#35763=CARTESIAN_POINT('Ctrl Pts',(-0.219763106780869,-0.00140024771169963,
0.0027736314491781));
#35764=CARTESIAN_POINT('Ctrl Pts',(-0.219935355158733,-0.00143367458564157,
0.00245471925505583));
#35765=CARTESIAN_POINT('Ctrl Pts',(-0.220074649373074,-0.00146068274866806,
0.00212083446913069));
#35766=CARTESIAN_POINT('Ctrl Pts',(-0.220353237801756,-0.00151469907472103,
0.00145306489728042));
#35767=CARTESIAN_POINT('Ctrl Pts',(-0.220499995520898,-0.00154301300909184,
0.000725393689757325));
#35768=CARTESIAN_POINT('Ctrl Pts',(-0.220499999832106,-0.00154301573465214,
-1.2615307860019E-6));
#35769=CARTESIAN_POINT('Ctrl Pts',(-0.220500004143313,-0.00154301846021245,
-0.000727916751329329));
#35770=CARTESIAN_POINT('Ctrl Pts',(-0.220353266885017,-0.00151470914363584,
-0.00145355702203918));
#35771=CARTESIAN_POINT('Ctrl Pts',(-0.220074654242848,-0.00146068379631778,
-0.00212082205575858));
#35772=CARTESIAN_POINT('Ctrl Pts',(-0.219935347921764,-0.00143367112265876,
-0.00245445457261828));
#35773=CARTESIAN_POINT('Ctrl Pts',(-0.219763071420699,-0.00140023460347288,
-0.0027734933586571));
#35774=CARTESIAN_POINT('Ctrl Pts',(-0.219562410856384,-0.00135085625104822,
-0.00307154800594128));
#35775=CARTESIAN_POINT('Ctrl Pts',(-0.219361750292068,-0.00130147789862356,
-0.00336960265322547));
#35776=CARTESIAN_POINT('Ctrl Pts',(-0.219132710242754,-0.00123617309737434,
-0.00364667970707124));
#35777=CARTESIAN_POINT('Ctrl Pts',(-0.218879812273829,-0.0011655117256891,
-0.00389834020393884));
#35778=CARTESIAN_POINT('Ctrl Pts',(-0.218533262901617,-0.00106868353010786,
-0.00424319385211476));
#35779=CARTESIAN_POINT('Ctrl Pts',(-0.21814193096314,-0.000961794536041287,
-0.00454033265003914));
#35780=CARTESIAN_POINT('Ctrl Pts',(-0.217717620464915,-0.000864182492545611,
-0.00478156822519172));
#35781=CARTESIAN_POINT('Ctrl Pts',(-0.217717620464915,-0.000864182492545611,
-0.00478156822519172));
#35782=CARTESIAN_POINT('Ctrl Pts',(-0.217522646165287,-0.000819325948101552,
-0.00489243010568115));
#35783=CARTESIAN_POINT('Ctrl Pts',(-0.217320705382708,-0.000776429290875688,
-0.00499148255206137));
#35784=CARTESIAN_POINT('Ctrl Pts',(-0.217112947318933,-0.000737367546107008,
-0.00507793792370663));
#35785=CARTESIAN_POINT('Ctrl Pts',(-0.216453070075793,-0.000613300369209368,
-0.00535253584428553));
#35786=CARTESIAN_POINT('Ctrl Pts',(-0.215734488701503,-0.000527921467098434,
-0.0055));
#35787=CARTESIAN_POINT('Ctrl Pts',(-0.215000000001605,-0.000525629159658772,
-0.0055));
#35788=CARTESIAN_POINT('',(-0.217113535264296,-0.000627890658473149,-0.00507769324464509));
#35789=CARTESIAN_POINT('Ctrl Pts',(-0.215000000458298,-0.000412691216678721,
-0.00549999999999998));
#35790=CARTESIAN_POINT('Ctrl Pts',(-0.215733763662974,-0.000415150006623741,
-0.00549999993833047));
#35791=CARTESIAN_POINT('Ctrl Pts',(-0.216453895571815,-0.000502156767438298,
-0.00535189476124435));
#35792=CARTESIAN_POINT('Ctrl Pts',(-0.217113535264296,-0.000627890658473149,
-0.00507769324464509));
#35793=CARTESIAN_POINT('Ctrl Pts',(-0.217113736162319,-0.00062792895318973,
-0.00507760972992005));
#35794=CARTESIAN_POINT('Ctrl Pts',(-0.21777343067469,-0.000753683498393302,
-0.00480335471430899));
#35795=CARTESIAN_POINT('Ctrl Pts',(-0.218372640661352,-0.000918161231759694,
-0.00440304836193869));
#35796=CARTESIAN_POINT('Ctrl Pts',(-0.218878461318587,-0.00106131402982561,
-0.00389968457354958));
#35797=CARTESIAN_POINT('Ctrl Pts',(-0.219131371647205,-0.00113289042885856,
-0.00364800267935503));
#35798=CARTESIAN_POINT('Ctrl Pts',(-0.219360923803304,-0.00119913785768892,
-0.00337054897752257));
#35799=CARTESIAN_POINT('Ctrl Pts',(-0.219561841261719,-0.00124918487971837,
-0.00307239351550298));
#35800=CARTESIAN_POINT('Ctrl Pts',(-0.219762758720135,-0.00129923190174783,
-0.00277423805348339));
#35801=CARTESIAN_POINT('Ctrl Pts',(-0.219935037411276,-0.00133307753813197,
-0.00245537690118891));
#35802=CARTESIAN_POINT('Ctrl Pts',(-0.220074378299315,-0.00136032636734795,
-0.00212148304035139));
#35803=CARTESIAN_POINT('Ctrl Pts',(-0.220353060075392,-0.0014148240257799,
-0.00145369531867635));
#35804=CARTESIAN_POINT('Ctrl Pts',(-0.220499972439958,-0.00144299794853512,
-0.000725772738476444));
#35805=CARTESIAN_POINT('Ctrl Pts',(-0.220499999860936,-0.00144300315744521,
1.12053422684619E-6));
#35806=CARTESIAN_POINT('Ctrl Pts',(-0.220500027281913,-0.0014430083663553,
0.000728013806930138));
#35807=CARTESIAN_POINT('Ctrl Pts',(-0.220353181889183,-0.00141484823386804,
0.00145387666412653));
#35808=CARTESIAN_POINT('Ctrl Pts',(-0.220074498824012,-0.00136034902137536,
0.00212119392664514));
#35809=CARTESIAN_POINT('Ctrl Pts',(-0.219935157291427,-0.00133309941512902,
0.00245485255790444));
#35810=CARTESIAN_POINT('Ctrl Pts',(-0.219762855704549,-0.00129925229730477,
0.00277387333358092));
#35811=CARTESIAN_POINT('Ctrl Pts',(-0.219562168120678,-0.00124926997129964,
0.00307190851276041));
#35812=CARTESIAN_POINT('Ctrl Pts',(-0.219361480536807,-0.00119928764529451,
0.0033699436919399));
#35813=CARTESIAN_POINT('Ctrl Pts',(-0.219132412388149,-0.00113317179309311,
0.00364699857065988));
#35814=CARTESIAN_POINT('Ctrl Pts',(-0.218879539633775,-0.00106161857632371,
0.00389861154566044));
#35815=CARTESIAN_POINT('Ctrl Pts',(-0.218373794125028,-0.000918512142784899,
0.00440183749566157));
#35816=CARTESIAN_POINT('Ctrl Pts',(-0.217772867004196,-0.000753649502850171,
0.00480332063947502));
#35817=CARTESIAN_POINT('Ctrl Pts',(-0.217113099314996,-0.000627808309406593,
0.00507787468216161));
#35818=CARTESIAN_POINT('Ctrl Pts',(-0.216453331762976,-0.000501967142128145,
0.00535242866776241));
#35819=CARTESIAN_POINT('Ctrl Pts',(-0.215734704272005,-0.000415151996213136,
0.00549999993863343));
#35820=CARTESIAN_POINT('Ctrl Pts',(-0.215000000458283,-0.000412690055633917,
0.00549999999999998));
#35821=CARTESIAN_POINT('Origin',(-0.215,-0.00247776328493882,0.));
#35822=CARTESIAN_POINT('',(-0.21771763199541,0.0158641872473072,0.0047815616735964));
#35823=CARTESIAN_POINT('Ctrl Pts',(-0.215000000001386,0.0155256291596571,
-0.0055));
#35824=CARTESIAN_POINT('Ctrl Pts',(-0.2157336570704,0.0155279188704998,
-0.0055));
#35825=CARTESIAN_POINT('Ctrl Pts',(-0.216453796318392,0.0156135057925174,
-0.00535197578874485));
#35826=CARTESIAN_POINT('Ctrl Pts',(-0.217113615626837,0.0157374949853798,
-0.00507765989564486));
#35827=CARTESIAN_POINT('Ctrl Pts',(-0.217773434935281,0.0158614841782422,
-0.00480334400254486));
#35828=CARTESIAN_POINT('Ctrl Pts',(-0.218372958291692,0.0160238716929941,
-0.00440280348312629));
#35829=CARTESIAN_POINT('Ctrl Pts',(-0.218878851501825,0.0161652458161567,
-0.00389929644268416));
#35830=CARTESIAN_POINT('Ctrl Pts',(-0.219131798106892,0.016235932877738,
-0.0036475429224631));
#35831=CARTESIAN_POINT('Ctrl Pts',(-0.219361326745382,0.0163013674845095,
-0.00337004045270962));
#35832=CARTESIAN_POINT('Ctrl Pts',(-0.219562216772735,0.0163508074239199,
-0.0030718359257235));
#35833=CARTESIAN_POINT('Ctrl Pts',(-0.219763106800088,0.0164002473633304,
-0.00277363139873738));
#35834=CARTESIAN_POINT('Ctrl Pts',(-0.219935355171308,0.0164336744598742,
-0.00245471922851232));
#35835=CARTESIAN_POINT('Ctrl Pts',(-0.220074649381718,0.016460682750153,
-0.0021208344484449));
#35836=CARTESIAN_POINT('Ctrl Pts',(-0.220353237802539,0.0165146993307108,
-0.00145306488831005));
#35837=CARTESIAN_POINT('Ctrl Pts',(-0.220499995524514,0.0165430131365752,
-0.000725393619809854));
#35838=CARTESIAN_POINT('Ctrl Pts',(-0.220499999832085,0.0165430157347685,
1.26162095524048E-6));
#35839=CARTESIAN_POINT('Ctrl Pts',(-0.220500004139655,0.0165430183329617,
0.000727916861720345));
#35840=CARTESIAN_POINT('Ctrl Pts',(-0.22035326687219,0.0165147088896741,
0.00145355711184016));
#35841=CARTESIAN_POINT('Ctrl Pts',(-0.220074654185537,0.0164606837862868,
0.00212082219289029));
#35842=CARTESIAN_POINT('Ctrl Pts',(-0.219935347842211,0.0164336712345932,
0.00245445473341535));
#35843=CARTESIAN_POINT('Ctrl Pts',(-0.219763071310037,0.0164002349297366,
0.00277349355999628));
#35844=CARTESIAN_POINT('Ctrl Pts',(-0.219562410692062,0.0163508569943117,
0.00307154825001662));
#35845=CARTESIAN_POINT('Ctrl Pts',(-0.219361750074086,0.0163014790588868,
0.00336960294003696));
#35846=CARTESIAN_POINT('Ctrl Pts',(-0.219132709948445,0.0162361748768451,
0.00364668003869167));
#35847=CARTESIAN_POINT('Ctrl Pts',(-0.21887981193522,0.0161655138270336,
0.00389834054094438));
#35848=CARTESIAN_POINT('Ctrl Pts',(-0.218533265738991,0.0160686869768679,
0.00424319097564957));
#35849=CARTESIAN_POINT('Ctrl Pts',(-0.218141937873558,0.0159617989582928,
0.00454032737798169));
#35850=CARTESIAN_POINT('Ctrl Pts',(-0.21771763199541,0.0158641872473072,
0.0047815616735964));
#35851=CARTESIAN_POINT('Ctrl Pts',(-0.21771763199541,0.0158641872473072,
0.0047815616735964));
#35852=CARTESIAN_POINT('Ctrl Pts',(-0.217522654035082,0.0158193295250965,
0.00489242625492518));
#35853=CARTESIAN_POINT('Ctrl Pts',(-0.21732070929407,0.0157764316704963,
0.00499148093737223));
#35854=CARTESIAN_POINT('Ctrl Pts',(-0.217112947042309,0.0157373688492824,
0.005077938038811));
#35855=CARTESIAN_POINT('Ctrl Pts',(-0.216453069909373,0.0156133007750843,
0.00535253587232454));
#35856=CARTESIAN_POINT('Ctrl Pts',(-0.215734488715537,0.0155279206225147,
0.0055));
#35857=CARTESIAN_POINT('Ctrl Pts',(-0.215000000001386,0.0155256283130808,
0.0055));
#35858=CARTESIAN_POINT('',(-0.217113535052694,0.0156278918245936,0.00507769333272214));
#35859=CARTESIAN_POINT('Ctrl Pts',(-0.215000000458283,0.0154126900556344,
0.00549999999999998));
#35860=CARTESIAN_POINT('Ctrl Pts',(-0.215733763690548,0.0154151488445598,
0.00549999993833244));
#35861=CARTESIAN_POINT('Ctrl Pts',(-0.216453895466079,0.0155021569505519,
0.00535189476437573));
#35862=CARTESIAN_POINT('Ctrl Pts',(-0.217113535052694,0.0156278918245936,
0.00507769333272214));
#35863=CARTESIAN_POINT('Ctrl Pts',(-0.217113735942853,0.0156279301181165,
0.00507760982127901));
#35864=CARTESIAN_POINT('Ctrl Pts',(-0.217773430347217,0.0157536856455482,
0.00480335489272425));
#35865=CARTESIAN_POINT('Ctrl Pts',(-0.218372640253876,0.0159181639994022,
0.00440304871061857));
#35866=CARTESIAN_POINT('Ctrl Pts',(-0.21887846101466,0.0160613161775311,
0.00389968487584725));
#35867=CARTESIAN_POINT('Ctrl Pts',(-0.219131371395052,0.0161328922665954,
0.00364800295846159));
#35868=CARTESIAN_POINT('Ctrl Pts',(-0.219360923648429,0.0161991390750316,
0.00337054917879593));
#35869=CARTESIAN_POINT('Ctrl Pts',(-0.219561841160825,0.0162491856697833,
0.00307239366528832));
#35870=CARTESIAN_POINT('Ctrl Pts',(-0.219762758673222,0.016299232264535,
0.00277423815178071));
#35871=CARTESIAN_POINT('Ctrl Pts',(-0.21993503737532,0.0163330776666233,
0.00245537697442852));
#35872=CARTESIAN_POINT('Ctrl Pts',(-0.220074378271048,0.0163603263626206,
0.00212148310796454));
#35873=CARTESIAN_POINT('Ctrl Pts',(-0.220353060062505,0.0164148237546151,
0.00145369537503657));
#35874=CARTESIAN_POINT('Ctrl Pts',(-0.220499972429734,0.0164429978133269,
0.00072577286152451));
#35875=CARTESIAN_POINT('Ctrl Pts',(-0.220499999860965,0.0164430031575457,
-1.12038921492091E-6));
#35876=CARTESIAN_POINT('Ctrl Pts',(-0.220500027292196,0.0164430085017644,
-0.000728013639954359));
#35877=CARTESIAN_POINT('Ctrl Pts',(-0.220353181916319,0.0164148485032365,
-0.00145387651991067));
#35878=CARTESIAN_POINT('Ctrl Pts',(-0.220074498903735,0.0163603490352413,
-0.00212119373592478));
#35879=CARTESIAN_POINT('Ctrl Pts',(-0.219935157397444,0.0163330993012436,
-0.00245485234393184));
#35880=CARTESIAN_POINT('Ctrl Pts',(-0.219762855845866,0.0162992519580117,
-0.0027738730790881));
#35881=CARTESIAN_POINT('Ctrl Pts',(-0.219562168320338,0.0162492692075871,
-0.00307190821624611));
#35882=CARTESIAN_POINT('Ctrl Pts',(-0.219361480794809,0.0161992864571625,
-0.00336994335340409));
#35883=CARTESIAN_POINT('Ctrl Pts',(-0.219132412727695,0.0161331699814419,
-0.00364699818864903));
#35884=CARTESIAN_POINT('Ctrl Pts',(-0.218879540019051,0.0160616164528147,
-0.00389861116226235));
#35885=CARTESIAN_POINT('Ctrl Pts',(-0.218373794601764,0.0159185093955602,
-0.00440183710948903));
#35886=CARTESIAN_POINT('Ctrl Pts',(-0.21777286742818,0.0157536473775453,
-0.00480332041750894));
#35887=CARTESIAN_POINT('Ctrl Pts',(-0.217113099616091,0.0156278071611984,
-0.00507787455686463));
#35888=CARTESIAN_POINT('Ctrl Pts',(-0.216453331941187,0.0155019669710174,
-0.00535242863913241));
#35889=CARTESIAN_POINT('Ctrl Pts',(-0.215734704256714,0.0154151531583194,
-0.00549999993863114));
#35890=CARTESIAN_POINT('Ctrl Pts',(-0.2150000004583,0.0154126912166778,
-0.00549999999999998));
#35891=CARTESIAN_POINT('Origin',(-0.206561432239279,0.00749997362422107,
-0.0135355036852295));
#35892=CARTESIAN_POINT('',(-0.186019881496892,0.0080786561625007,-0.00979684401252669));
#35893=CARTESIAN_POINT('Ctrl Pts',(-0.185999364351523,0.00750000038130581,
-0.00991138348445716));
#35894=CARTESIAN_POINT('Ctrl Pts',(-0.185999376571405,0.00769038170948611,
-0.00991131415203012));
#35895=CARTESIAN_POINT('Ctrl Pts',(-0.186006003258135,0.00788326696988442,
-0.00987309608428367));
#35896=CARTESIAN_POINT('Ctrl Pts',(-0.186019881496892,0.0080786561625007,
-0.00979684401252669));
#35897=CARTESIAN_POINT('',(-0.186041755776097,0.00833112667101796,-0.00967861197300846));
#35898=CARTESIAN_POINT('Ctrl Pts',(-0.186019884086589,0.00807868868559217,
-0.00979683137349002));
#35899=CARTESIAN_POINT('Ctrl Pts',(-0.186026050577798,0.0081655192043983,
-0.00976295055579292));
#35900=CARTESIAN_POINT('Ctrl Pts',(-0.186033396771404,0.0082494356206791,
-0.00972306503719262));
#35901=CARTESIAN_POINT('Ctrl Pts',(-0.186041751529428,0.00833112740062736,
-0.00967861548148799));
#35902=CARTESIAN_POINT('',(-0.186045753543968,0.00835130156890068,-0.00965738420265808));
#35903=CARTESIAN_POINT('Ctrl Pts',(-0.186045764689502,0.00835128455723845,
-0.00965738815309785));
#35904=CARTESIAN_POINT('Ctrl Pts',(-0.186043858668127,0.00835231500591592,
-0.00966747326300593));
#35905=CARTESIAN_POINT('Ctrl Pts',(-0.186042683533208,0.00834015517577814,
-0.00967370297361173));
#35906=CARTESIAN_POINT('Ctrl Pts',(-0.186041757888406,0.00833112619861691,
-0.00967861022784464));
#35907=CARTESIAN_POINT('',(-0.186045753664356,0.00664869142106229,-0.00965738356578759));
#35908=CARTESIAN_POINT('Ctrl Pts',(-0.186045753543968,0.00835130156890068,
-0.00965738420265809));
#35909=CARTESIAN_POINT('Ctrl Pts',(-0.186036006823495,0.00778376485295418,
-0.00970894540982141));
#35910=CARTESIAN_POINT('Ctrl Pts',(-0.186036006863625,0.00721622813700805,
-0.00970894519753124));
#35911=CARTESIAN_POINT('Ctrl Pts',(-0.186045753664356,0.00664869142106229,
-0.00965738356578759));
#35912=CARTESIAN_POINT('',(-0.186041751543844,0.00666887245842392,-0.00967861584559627));
#35913=CARTESIAN_POINT('Origin',(-0.185976327015533,0.0109621773062506,
-0.0100140390940224));
#35914=CARTESIAN_POINT('',(-0.186019881496891,0.00692134383750547,-0.00979684401253565));
#35915=CARTESIAN_POINT('Ctrl Pts',(-0.18604175150383,0.00666887245842397,
-0.00967861583807533));
#35916=CARTESIAN_POINT('Ctrl Pts',(-0.186033396755342,0.0067505641315426,
-0.00972306534721564));
#35917=CARTESIAN_POINT('Ctrl Pts',(-0.186026050751142,0.00683448212941961,
-0.00976294803884862));
#35918=CARTESIAN_POINT('Ctrl Pts',(-0.186019884286368,0.00692131244471435,
-0.00979682868616852));
#35919=CARTESIAN_POINT('Ctrl Pts',(-0.186019881496891,0.00692134383750547,
-0.00979684401253565));
#35920=CARTESIAN_POINT('Ctrl Pts',(-0.186006003262742,0.00711673296524612,
-0.00987309605897389));
#35921=CARTESIAN_POINT('Ctrl Pts',(-0.185999376576004,0.00730961835274437,
-0.00991131412676384));
#35922=CARTESIAN_POINT('Ctrl Pts',(-0.185999364351498,0.00750000000000023,
-0.00991138348459597));
#35923=CARTESIAN_POINT('Origin',(-0.238,-0.00203858085746875,-0.0110866403454819));
#35924=CARTESIAN_POINT('',(-0.230921436096816,0.0162188491197267,-0.00255390765181725));
#35925=CARTESIAN_POINT('',(-0.230921436098924,0.0163191149846998,-0.0025539076543603));
#35926=CARTESIAN_POINT('',(-0.2309214360969,-0.00203858085746875,-0.00255390765191895));
#35927=CARTESIAN_POINT('',(-0.235510405486502,0.0139139931904494,-0.0080856016051615));
#35928=CARTESIAN_POINT('Ctrl Pts',(-0.2309214360969,0.0163191144755479,
-0.00255390765191895));
#35929=CARTESIAN_POINT('Ctrl Pts',(-0.23174153328286,0.0162404099789032,
-0.00354247965131538));
#35930=CARTESIAN_POINT('Ctrl Pts',(-0.233359727310792,0.0157744006398884,
-0.00549310371513331));
#35931=CARTESIAN_POINT('Ctrl Pts',(-0.234843981104082,0.0146553646943324,
-0.0072822718346736));
#35932=CARTESIAN_POINT('Ctrl Pts',(-0.235510405486502,0.0139139931904494,
-0.00808560160516149));
#35933=CARTESIAN_POINT('',(-0.237188474496957,0.011147446881013,-0.0101084009333268));
#35934=CARTESIAN_POINT('Ctrl Pts',(-0.235510405486502,0.0139139931904494,
-0.00808560160516149));
#35935=CARTESIAN_POINT('Ctrl Pts',(-0.236176829868922,0.0131726216865665,
-0.00888893137564938));
#35936=CARTESIAN_POINT('Ctrl Pts',(-0.236767551737116,0.0122493966515786,
-0.00960100685685503));
#35937=CARTESIAN_POINT('Ctrl Pts',(-0.237188474496957,0.011147446881013,
-0.0101084009333268));
#35938=CARTESIAN_POINT('',(-0.237859980412293,0.00748903372880752,-0.0109178561499695));
#35939=CARTESIAN_POINT('Ctrl Pts',(-0.237188474496957,0.011147446881013,
-0.0101084009333268));
#35940=CARTESIAN_POINT('Ctrl Pts',(-0.237609397256798,0.0100454971104472,
-0.0106157950097985));
#35941=CARTESIAN_POINT('Ctrl Pts',(-0.237860520908286,0.00876482260430375,
-0.0109185076815363));
#35942=CARTESIAN_POINT('Ctrl Pts',(-0.237859980412293,0.00748903372880752,
-0.0109178561499695));
#35943=CARTESIAN_POINT('',(-0.230921436098932,-0.00131911498648589,-0.00255390765437028));
#35944=CARTESIAN_POINT('Ctrl Pts',(-0.237859980412293,0.00748903372880752,
-0.0109178561499695));
#35945=CARTESIAN_POINT('Ctrl Pts',(-0.2378594399163,0.00621324485331131,
-0.0109172046184027));
#35946=CARTESIAN_POINT('Ctrl Pts',(-0.237355030629353,0.00367143836361342,
-0.0103091731486599));
#35947=CARTESIAN_POINT('Ctrl Pts',(-0.235579072060058,0.000893727961130872,
-0.00816837454119071));
#35948=CARTESIAN_POINT('Ctrl Pts',(-0.233347520676672,-0.00077875050644683,
-0.00547838943869806));
#35949=CARTESIAN_POINT('Ctrl Pts',(-0.231741081373355,-0.00124045334853188,
-0.00354193490480122));
#35950=CARTESIAN_POINT('Ctrl Pts',(-0.2309214360969,-0.00131911447555364,
-0.00255390765191895));
#35951=CARTESIAN_POINT('',(-0.230921436096816,-0.00121884911973092,-0.00255390765181755));
#35952=CARTESIAN_POINT('',(-0.2309214360969,-0.00203858085746875,-0.00255390765191895));
#35953=CARTESIAN_POINT('Ctrl Pts',(-0.2309214360969,-0.00121884911929219,
-0.00255390765191893));
#35954=CARTESIAN_POINT('Ctrl Pts',(-0.231731717669817,-0.00114029951282499,
-0.00353064758997169));
#35955=CARTESIAN_POINT('Ctrl Pts',(-0.232531008931408,-0.000909424775714629,
-0.00449413944691078));
#35956=CARTESIAN_POINT('Ctrl Pts',(-0.233297221966274,-0.000517292730967896,
-0.00541775772631526));
#35957=CARTESIAN_POINT('Ctrl Pts',(-0.23406343500114,-0.000125160686221158,
-0.00634137600571974));
#35958=CARTESIAN_POINT('Ctrl Pts',(-0.23479656980928,0.000428228666161958,
-0.00722512070758961));
#35959=CARTESIAN_POINT('Ctrl Pts',(-0.235454855653561,0.00116121765859052,
-0.00801864001773443));
#35960=CARTESIAN_POINT('Ctrl Pts',(-0.236113141497842,0.00189420665101909,
-0.00881215932787925));
#35961=CARTESIAN_POINT('Ctrl Pts',(-0.236696578378263,0.0028067952834931,
-0.00951545324629902));
#35962=CARTESIAN_POINT('Ctrl Pts',(-0.237112279773004,0.00389578721949753,
-0.0100165533183223));
#35963=CARTESIAN_POINT('Ctrl Pts',(-0.237527981167745,0.00498477915550195,
-0.0105176533903456));
#35964=CARTESIAN_POINT('Ctrl Pts',(-0.237775947076806,0.0062501743950368,
-0.0108165596159724));
#35965=CARTESIAN_POINT('Ctrl Pts',(-0.237775416097689,0.00751077204058868,
-0.0108159195563599));
#35966=CARTESIAN_POINT('Ctrl Pts',(-0.237774885118572,0.00877136968614057,
-0.0108152794967474));
#35967=CARTESIAN_POINT('Ctrl Pts',(-0.237525857251278,0.0100271697377095,
-0.0105150931518957));
#35968=CARTESIAN_POINT('Ctrl Pts',(-0.237109005915905,0.011112676361498,
-0.0100126069037839));
#35969=CARTESIAN_POINT('Ctrl Pts',(-0.236692154580533,0.0121981829852864,
-0.00951012065567206));
#35970=CARTESIAN_POINT('Ctrl Pts',(-0.236107479777082,0.0131133961812944,
-0.00880533450430022));
#35971=CARTESIAN_POINT('Ctrl Pts',(-0.235447733272926,0.0138467040480916,
-0.00801005446691648));
#35972=CARTESIAN_POINT('Ctrl Pts',(-0.234787986768769,0.0145800119148888,
-0.00721477442953273));
#35973=CARTESIAN_POINT('Ctrl Pts',(-0.234053168563907,0.0151314144524751,
-0.00632900050613708));
#35974=CARTESIAN_POINT('Ctrl Pts',(-0.2332889897904,0.0155214971606677,
-0.00540783439198091));
#35975=CARTESIAN_POINT('Ctrl Pts',(-0.232524811016894,0.0159115798688603,
-0.00448666827782475));
#35976=CARTESIAN_POINT('Ctrl Pts',(-0.231731271674744,0.0161403427476591,
-0.00353010997290807));
#35977=CARTESIAN_POINT('Ctrl Pts',(-0.2309214360969,0.0162188491192864,
-0.00255390765191896));
#35978=CARTESIAN_POINT('Origin',(-0.234,-0.00203858085746875,0.));
#35979=CARTESIAN_POINT('',(-0.230644549324729,-0.00134174864052366,-0.00217737244536236));
#35980=CARTESIAN_POINT('Ctrl Pts',(-0.230921436078517,-0.00131911447736198,
-0.00255390762975915));
#35981=CARTESIAN_POINT('Ctrl Pts',(-0.230882799080788,-0.00132291515868807,
-0.00250733332704017));
#35982=CARTESIAN_POINT('Ctrl Pts',(-0.230847896563029,-0.00132621572305467,
-0.00246332967147474));
#35983=CARTESIAN_POINT('Ctrl Pts',(-0.23081093623588,-0.00132932875912759,
-0.00241451285115208));
#35984=CARTESIAN_POINT('Ctrl Pts',(-0.230773975902869,-0.00133244179569423,
-0.0023656960230872));
#35985=CARTESIAN_POINT('Ctrl Pts',(-0.230735375114978,-0.00133536730390772,
-0.00231172564600153));
#35986=CARTESIAN_POINT('Ctrl Pts',(-0.230710890470543,-0.00133716751732438,
-0.00227634762354863));
#35987=CARTESIAN_POINT('Ctrl Pts',(-0.230686405826108,-0.00133896773074104,
-0.00224096960109574));
#35988=CARTESIAN_POINT('Ctrl Pts',(-0.230675274796775,-0.00133964264936088,
-0.00222472208742556));
#35989=CARTESIAN_POINT('Ctrl Pts',(-0.230644549324729,-0.00134174864052366,
-0.00217737244536236));
#35990=CARTESIAN_POINT('',(-0.230177928184924,-0.00137996828035668,-0.00117973176629321));
#35991=CARTESIAN_POINT('Ctrl Pts',(-0.230644549324729,-0.00134174864052366,
-0.00217737244536236));
#35992=CARTESIAN_POINT('Ctrl Pts',(-0.230613823852683,-0.00134385463168645,
-0.00213002280329915));
#35993=CARTESIAN_POINT('Ctrl Pts',(-0.230564811227978,-0.00134739169539217,
-0.00205070191669902));
#35994=CARTESIAN_POINT('Ctrl Pts',(-0.230526711870365,-0.00135027334534756,
-0.00198400341948652));
#35995=CARTESIAN_POINT('Ctrl Pts',(-0.230488612512752,-0.00135315499530295,
-0.00191730492227402));
#35996=CARTESIAN_POINT('Ctrl Pts',(-0.230460264018485,-0.00135538123150799,
-0.00186386387206019));
#35997=CARTESIAN_POINT('Ctrl Pts',(-0.230432675646478,-0.00135759386813896,
-0.00180947422108362));
#35998=CARTESIAN_POINT('Ctrl Pts',(-0.23040508727447,-0.00135980650476992,
-0.00175508457010705));
#35999=CARTESIAN_POINT('Ctrl Pts',(-0.2303785700858,-0.00136200554182681,
-0.00169961760553389));
#36000=CARTESIAN_POINT('Ctrl Pts',(-0.23035438300816,-0.00136405859429202,
-0.00164604882941069));
#36001=CARTESIAN_POINT('Ctrl Pts',(-0.230330195930519,-0.00136611164675724,
-0.00159248005328749));
#36002=CARTESIAN_POINT('Ctrl Pts',(-0.230308335987054,-0.00136801871463078,
-0.0015407943852381));
#36003=CARTESIAN_POINT('Ctrl Pts',(-0.230289909162091,-0.00136966752380675,
-0.00149506721402873));
#36004=CARTESIAN_POINT('Ctrl Pts',(-0.230271482337128,-0.00137131633298271,
-0.00144934004281937));
#36005=CARTESIAN_POINT('Ctrl Pts',(-0.230256225289845,-0.00137270688346108,
-0.00140968640751628));
#36006=CARTESIAN_POINT('Ctrl Pts',(-0.230237435583795,-0.00137442065668314,
-0.00135761151067073));
#36007=CARTESIAN_POINT('Ctrl Pts',(-0.230218645877745,-0.00137613442990519,
-0.00130553661382518));
#36008=CARTESIAN_POINT('Ctrl Pts',(-0.230196798002912,-0.00137817142587091,
-0.00124086583214421));
#36009=CARTESIAN_POINT('Ctrl Pts',(-0.230177928184924,-0.00137996828035668,
-0.00117973176629321));
#36010=CARTESIAN_POINT('',(-0.230090092993501,-0.00138849741546914,0.000844172494537475));
#36011=CARTESIAN_POINT('Ctrl Pts',(-0.230177928184924,-0.00137996828035668,
-0.00117973176629321));
#36012=CARTESIAN_POINT('Ctrl Pts',(-0.230159058366936,-0.00138176513484245,
-0.00111859770044221));
#36013=CARTESIAN_POINT('Ctrl Pts',(-0.230142844554009,-0.00138332184784826,
-0.00106109506496594));
#36014=CARTESIAN_POINT('Ctrl Pts',(-0.230127856833695,-0.00138477612973666,
-0.00100324837385142));
#36015=CARTESIAN_POINT('Ctrl Pts',(-0.230097881393066,-0.00138768469351348,
-0.000887554991622391));
#36016=CARTESIAN_POINT('Ctrl Pts',(-0.230073193248961,-0.00139018353282069,
-0.000770398928202508));
#36017=CARTESIAN_POINT('Ctrl Pts',(-0.230054246319814,-0.00139217250561596,
-0.000656527147420392));
#36018=CARTESIAN_POINT('Ctrl Pts',(-0.230016352461521,-0.00139615045120648,
-0.000428783585856158));
#36019=CARTESIAN_POINT('Ctrl Pts',(-0.229999991480358,-0.00139808893074921,
-0.000214343200170112));
#36020=CARTESIAN_POINT('Ctrl Pts',(-0.230000000003157,-0.00139808796585182,
1.58931735004758E-7));
#36021=CARTESIAN_POINT('Ctrl Pts',(-0.230000008525956,-0.00139808700095444,
0.000214661063640121));
#36022=CARTESIAN_POINT('Ctrl Pts',(-0.230016386700035,-0.00139614659161695,
0.000429102397676562));
#36023=CARTESIAN_POINT('Ctrl Pts',(-0.230054299127194,-0.00139216694241518,
0.000656844443027331));
#36024=CARTESIAN_POINT('Ctrl Pts',(-0.230064575031583,-0.00139108828568537,
0.000718572368636326));
#36025=CARTESIAN_POINT('Ctrl Pts',(-0.230076537999235,-0.00138985981742396,
0.000781265223738882));
#36026=CARTESIAN_POINT('Ctrl Pts',(-0.230090092993501,-0.00138849741546914,
0.000844172494537474));
#36027=CARTESIAN_POINT('',(-0.230631851022661,-0.00134262389237757,0.00215767756313376));
#36028=CARTESIAN_POINT('Ctrl Pts',(-0.230090092993501,-0.00138849741546914,
0.000844172494537474));
#36029=CARTESIAN_POINT('Ctrl Pts',(-0.230101586445131,-0.00138734656102728,
0.000897305354721647));
#36030=CARTESIAN_POINT('Ctrl Pts',(-0.230114209192546,-0.0013861001369068,
0.000950592216182026));
#36031=CARTESIAN_POINT('Ctrl Pts',(-0.230127941497652,-0.0013847677136554,
0.00100357508657684));
#36032=CARTESIAN_POINT('Ctrl Pts',(-0.230142935923704,-0.00138331282885944,
0.00106142755387902));
#36033=CARTESIAN_POINT('Ctrl Pts',(-0.230159157926241,-0.00138175541030722,
0.00111893911964585));
#36034=CARTESIAN_POINT('Ctrl Pts',(-0.230178031105433,-0.00137995842001515,
0.00118006515453991));
#36035=CARTESIAN_POINT('Ctrl Pts',(-0.230196904284625,-0.00137816142972308,
0.00124119118943398));
#36036=CARTESIAN_POINT('Ctrl Pts',(-0.23021874909407,-0.00137612486769115,
0.00130583742520534));
#36037=CARTESIAN_POINT('Ctrl Pts',(-0.230237558682426,-0.00137440934020132,
0.0013579526250255));
#36038=CARTESIAN_POINT('Ctrl Pts',(-0.230256368270783,-0.0013726938127115,
0.00141006782484567));
#36039=CARTESIAN_POINT('Ctrl Pts',(-0.230271669717474,-0.00137129931976377,
0.00144982607665868));
#36040=CARTESIAN_POINT('Ctrl Pts',(-0.230290148658564,-0.00136964611118522,
0.00149566140033204));
#36041=CARTESIAN_POINT('Ctrl Pts',(-0.230308627599653,-0.00136799290260666,
0.0015414967240054));
#36042=CARTESIAN_POINT('Ctrl Pts',(-0.230330546798724,-0.00136608097839726,
0.00159329422029309));
#36043=CARTESIAN_POINT('Ctrl Pts',(-0.230354813070871,-0.00136402176524664,
0.00164700098715987));
#36044=CARTESIAN_POINT('Ctrl Pts',(-0.230379079343017,-0.00136196255209602,
0.00170070775402666));
#36045=CARTESIAN_POINT('Ctrl Pts',(-0.230405696697909,-0.00135975605000417,
0.00175633858822025));
#36046=CARTESIAN_POINT('Ctrl Pts',(-0.230433388432851,-0.0013575363023856,
0.0018108787726071));
#36047=CARTESIAN_POINT('Ctrl Pts',(-0.230461080167794,-0.00135531655476703,
0.00186541895699396));
#36048=CARTESIAN_POINT('Ctrl Pts',(-0.230489531299431,-0.00135308356162173,
0.00191899887599725));
#36049=CARTESIAN_POINT('Ctrl Pts',(-0.230527819237574,-0.00135018972260209,
0.00198594077279254));
#36050=CARTESIAN_POINT('Ctrl Pts',(-0.230560639448383,-0.00134770913964887,
0.00204332299997208));
#36051=CARTESIAN_POINT('Ctrl Pts',(-0.230601554664194,-0.00134474297874676,
0.00211004895575857));
#36052=CARTESIAN_POINT('Ctrl Pts',(-0.230631851022661,-0.00134262389237757,
0.00215767756313376));
#36053=CARTESIAN_POINT('',(-0.230921436098924,-0.00131911515712292,0.00255390765436055));
#36054=CARTESIAN_POINT('Ctrl Pts',(-0.230631851022661,-0.00134262389237757,
0.00215767756313376));
#36055=CARTESIAN_POINT('Ctrl Pts',(-0.230636938528349,-0.00134227086032266,
0.00216558622571961));
#36056=CARTESIAN_POINT('Ctrl Pts',(-0.230641697776003,-0.00134194133826565,
0.00217298659707199));
#36057=CARTESIAN_POINT('Ctrl Pts',(-0.230646076892515,-0.00134164148808831,
0.00217972470488308));
#36058=CARTESIAN_POINT('Ctrl Pts',(-0.230676741798038,-0.00133954177748817,
0.00222690852355222));
#36059=CARTESIAN_POINT('Ctrl Pts',(-0.230687445580514,-0.00133889704118191,
0.00224249809727657));
#36060=CARTESIAN_POINT('Ctrl Pts',(-0.230711699376962,-0.00133711083075126,
0.0022775159741538));
#36061=CARTESIAN_POINT('Ctrl Pts',(-0.230735953173409,-0.00133532462032062,
0.00231253385103102));
#36062=CARTESIAN_POINT('Ctrl Pts',(-0.230774523982444,-0.0013323969357656,
0.00236643847055));
#36063=CARTESIAN_POINT('Ctrl Pts',(-0.230811381856284,-0.00132929059247327,
0.00241510130917168));
#36064=CARTESIAN_POINT('Ctrl Pts',(-0.230848239724272,-0.00132618424967403,
0.00246376414006875));
#36065=CARTESIAN_POINT('Ctrl Pts',(-0.230882962056323,-0.0013228992481942,
0.00250752978309291));
#36066=CARTESIAN_POINT('Ctrl Pts',(-0.230921436078578,-0.00131911464972426,
0.00255390762983318));
#36067=CARTESIAN_POINT('',(-0.230921436096816,-0.00121884929995214,0.00255390765181725));
#36068=CARTESIAN_POINT('',(-0.2309214360969,-0.00203858085746875,0.00255390765191894));
#36069=CARTESIAN_POINT('',(-0.230686015102297,-0.00123880444284725,0.00223997859315595));
#36070=CARTESIAN_POINT('Ctrl Pts',(-0.230921436096798,-0.00121884929952187,
0.0025539076517962));
#36071=CARTESIAN_POINT('Ctrl Pts',(-0.230882799449418,-0.00122268836356969,
0.00250733377201141));
#36072=CARTESIAN_POINT('Ctrl Pts',(-0.230848935241631,-0.00122594473354211,
0.00246470149188065));
#36073=CARTESIAN_POINT('Ctrl Pts',(-0.230810937523616,-0.00122916575459618,
0.00241451455197912));
#36074=CARTESIAN_POINT('Ctrl Pts',(-0.2307729398056,-0.00123238677565026,
0.00236432761207759));
#36075=CARTESIAN_POINT('Ctrl Pts',(-0.230731466942441,-0.00123557244778599,
0.00230607861984655));
#36076=CARTESIAN_POINT('Ctrl Pts',(-0.230710893414538,-0.00123708073550189,
0.00227635187734016));
#36077=CARTESIAN_POINT('Ctrl Pts',(-0.230700606650587,-0.00123783487935984,
0.00226148850608696));
#36078=CARTESIAN_POINT('Ctrl Pts',(-0.230695395139944,-0.00123816967711283,
0.00225385609323441));
#36079=CARTESIAN_POINT('Ctrl Pts',(-0.230686015102297,-0.00123880444284725,
0.00223997859315595));
#36080=CARTESIAN_POINT('',(-0.230177916607466,-0.00127992933296153,0.00117969425721745));
#36081=CARTESIAN_POINT('Ctrl Pts',(-0.230686015102297,-0.00123880444284725,
0.00223997859315595));
#36082=CARTESIAN_POINT('Ctrl Pts',(-0.23067663506465,-0.00123943920858166,
0.00222610109307748));
#36083=CARTESIAN_POINT('Ctrl Pts',(-0.230663124603842,-0.0012403739422975,
0.00220595594828946));
#36084=CARTESIAN_POINT('Ctrl Pts',(-0.23064607382111,-0.00124156614273087,
0.00217971997893273));
#36085=CARTESIAN_POINT('Ctrl Pts',(-0.230611972255647,-0.0012439505435976,
0.00212724804021926));
#36086=CARTESIAN_POINT('Ctrl Pts',(-0.230564381867535,-0.00124736481133447,
0.00204995014329134));
#36087=CARTESIAN_POINT('Ctrl Pts',(-0.230526713362572,-0.00125020352011288,
0.00198400603181192));
#36088=CARTESIAN_POINT('Ctrl Pts',(-0.23048904485761,-0.00125304222889129,
0.00191806192033251));
#36089=CARTESIAN_POINT('Ctrl Pts',(-0.230460339630388,-0.00125530537871126,
0.00186401604814319));
#36090=CARTESIAN_POINT('Ctrl Pts',(-0.230432634059847,-0.00125753302523568,
0.00180939223194782));
#36091=CARTESIAN_POINT('Ctrl Pts',(-0.230404928489305,-0.0012597606717601,
0.00175476841575245));
#36092=CARTESIAN_POINT('Ctrl Pts',(-0.230378492299106,-0.00126195281498897,
0.00169944971928871));
#36093=CARTESIAN_POINT('Ctrl Pts',(-0.230354332272838,-0.00126400452606611,
0.00164593645780533));
#36094=CARTESIAN_POINT('Ctrl Pts',(-0.230330172246571,-0.00126605623714324,
0.00159242319632194));
#36095=CARTESIAN_POINT('Ctrl Pts',(-0.230308296038245,-0.00126796751606864,
0.00154069824975554));
#36096=CARTESIAN_POINT('Ctrl Pts',(-0.230289875122175,-0.00126961802260417,
0.00149498273934548));
#36097=CARTESIAN_POINT('Ctrl Pts',(-0.230271454206105,-0.00127126852913971,
0.00144926722893541));
#36098=CARTESIAN_POINT('Ctrl Pts',(-0.230256221881221,-0.0012726582632854,
0.00140967676806264));
#36099=CARTESIAN_POINT('Ctrl Pts',(-0.23023743718714,-0.00127437351484988,
0.00135761595426707));
#36100=CARTESIAN_POINT('Ctrl Pts',(-0.230218652493058,-0.00127608876641436,
0.00130555514047149));
#36101=CARTESIAN_POINT('Ctrl Pts',(-0.230196792075838,-0.00127812953539765,
0.00124084875869349));
#36102=CARTESIAN_POINT('Ctrl Pts',(-0.230177916607466,-0.00127992933296153,
0.00117969425721745));
#36103=CARTESIAN_POINT('',(-0.230089138316471,-0.00128856509794021,-0.00083973858569693));
#36104=CARTESIAN_POINT('Ctrl Pts',(-0.230177916607466,-0.00127992933296153,
0.00117969425721745));
#36105=CARTESIAN_POINT('Ctrl Pts',(-0.230159041139093,-0.00128172913052541,
0.00111853975574141));
#36106=CARTESIAN_POINT('Ctrl Pts',(-0.230142827170788,-0.00128328795666989,
0.00106103218438422));
#36107=CARTESIAN_POINT('Ctrl Pts',(-0.230127839090187,-0.00128474428551632,
0.00100317988841401));
#36108=CARTESIAN_POINT('Ctrl Pts',(-0.230097862928986,-0.00128765694320919,
0.000887475296473585));
#36109=CARTESIAN_POINT('Ctrl Pts',(-0.230073174819639,-0.00129015961170986,
0.000770305086855483));
#36110=CARTESIAN_POINT('Ctrl Pts',(-0.23005423052057,-0.00129215159395536,
0.000656432186292065));
#36111=CARTESIAN_POINT('Ctrl Pts',(-0.230016341922432,-0.00129613555844635,
0.000428686385165228));
#36112=CARTESIAN_POINT('Ctrl Pts',(-0.229999991618744,-0.00129807677791666,
0.000214296247717829));
#36113=CARTESIAN_POINT('Ctrl Pts',(-0.230000000003057,-0.0012980758241512,
-1.56385361932959E-7));
#36114=CARTESIAN_POINT('Ctrl Pts',(-0.23000000838737,-0.00129807487038574,
-0.000214609018441695));
#36115=CARTESIAN_POINT('Ctrl Pts',(-0.230016375665871,-0.00129613174338452,
-0.00042900110087048));
#36116=CARTESIAN_POINT('Ctrl Pts',(-0.2300542827742,-0.00129214607791548,
-0.000656746202139764));
#36117=CARTESIAN_POINT('Ctrl Pts',(-0.230064320562544,-0.00129109067516511,
-0.000717053021196674));
#36118=CARTESIAN_POINT('Ctrl Pts',(-0.230075969322042,-0.00128989205197605,
-0.000778284469665095));
#36119=CARTESIAN_POINT('Ctrl Pts',(-0.230089138316471,-0.00128856509794021,
-0.00083973858569693));
#36120=CARTESIAN_POINT('',(-0.230625302305309,-0.00124302410204978,-0.00214742065498236));
#36121=CARTESIAN_POINT('Ctrl Pts',(-0.230089138316471,-0.00128856509794021,
-0.00083973858569693));
#36122=CARTESIAN_POINT('Ctrl Pts',(-0.230100879996404,-0.00128738647063385,
-0.000894316709739802));
#36123=CARTESIAN_POINT('Ctrl Pts',(-0.230113816044822,-0.00128610659862752,
-0.000949071248456438));
#36124=CARTESIAN_POINT('Ctrl Pts',(-0.230127923152874,-0.00128473591577273,
-0.00100350430489781));
#36125=CARTESIAN_POINT('Ctrl Pts',(-0.230142917929652,-0.00128327898474434,
-0.00106136248020177));
#36126=CARTESIAN_POINT('Ctrl Pts',(-0.230159140066374,-0.00128171945503964,
-0.00111887904402635));
#36127=CARTESIAN_POINT('Ctrl Pts',(-0.230178018970065,-0.00127991951244512,
-0.0011800258500632));
#36128=CARTESIAN_POINT('Ctrl Pts',(-0.230196897873756,-0.0012781195698506,
-0.00124117265610004));
#36129=CARTESIAN_POINT('Ctrl Pts',(-0.230218755423235,-0.00127607921436627,
-0.00130585509784703));
#36130=CARTESIAN_POINT('Ctrl Pts',(-0.230237559819384,-0.00127436222761337,
-0.00135795577515773));
#36131=CARTESIAN_POINT('Ctrl Pts',(-0.230256364215533,-0.00127264524086048,
-0.00141005645246844));
#36132=CARTESIAN_POINT('Ctrl Pts',(-0.230271640302773,-0.00127125162283904,
-0.00144975005927987));
#36133=CARTESIAN_POINT('Ctrl Pts',(-0.230290114091531,-0.00126959663178466,
-0.00149557565711002));
#36134=CARTESIAN_POINT('Ctrl Pts',(-0.230308587880288,-0.00126794164073029,
-0.00154140125494016));
#36135=CARTESIAN_POINT('Ctrl Pts',(-0.23033052579338,-0.00126602527664298,
-0.00159324329923622));
#36136=CARTESIAN_POINT('Ctrl Pts',(-0.230354762074236,-0.00126396768010872,
-0.00164688811537833));
#36137=CARTESIAN_POINT('Ctrl Pts',(-0.230378998355092,-0.00126191008357446,
-0.00170053293152045));
#36138=CARTESIAN_POINT('Ctrl Pts',(-0.230405525206895,-0.00125971125459324,
-0.00175599774203875));
#36139=CARTESIAN_POINT('Ctrl Pts',(-0.230433347291843,-0.00125747537258556,
-0.00181079774116085));
#36140=CARTESIAN_POINT('Ctrl Pts',(-0.23046116937679,-0.00125523949057789,
-0.00186559774028295));
#36141=CARTESIAN_POINT('Ctrl Pts',(-0.230490017676975,-0.00125296655554375,
-0.00191984949807499));
#36142=CARTESIAN_POINT('Ctrl Pts',(-0.230527822460804,-0.00125011970921519,
-0.0019859464082148));
#36143=CARTESIAN_POINT('Ctrl Pts',(-0.230558007660088,-0.00124784664705071,
-0.00203872143302736));
#36144=CARTESIAN_POINT('Ctrl Pts',(-0.230594516023534,-0.0012452077043151,
-0.00209869927530583));
#36145=CARTESIAN_POINT('Ctrl Pts',(-0.230625302305309,-0.00124302410204978,
-0.00214742065498236));
#36146=CARTESIAN_POINT('Ctrl Pts',(-0.230625302305309,-0.00124302410204978,
-0.00214742065498236));
#36147=CARTESIAN_POINT('Ctrl Pts',(-0.230633137488449,-0.00124247290005448,
-0.00215967828816978));
#36148=CARTESIAN_POINT('Ctrl Pts',(-0.230640560315198,-0.0012419507122686,
-0.00217124931158208));
#36149=CARTESIAN_POINT('Ctrl Pts',(-0.230647428858057,-0.0012414707477488,
-0.00218180355170074));
#36150=CARTESIAN_POINT('Ctrl Pts',(-0.230664468092708,-0.00124028006899138,
-0.00220798613185289));
#36151=CARTESIAN_POINT('Ctrl Pts',(-0.230677927294496,-0.001239349240261,
-0.00222802755915694));
#36152=CARTESIAN_POINT('Ctrl Pts',(-0.230687201831431,-0.00123872188163988,
-0.00224173332364162));
#36153=CARTESIAN_POINT('Ctrl Pts',(-0.230696476368366,-0.00123809452301875,
-0.0022554390881263));
#36154=CARTESIAN_POINT('Ctrl Pts',(-0.230701528656117,-0.00123777063450688,
-0.00226283144073695));
#36155=CARTESIAN_POINT('Ctrl Pts',(-0.230711703464447,-0.00123702342528048,
-0.00227752187569489));
#36156=CARTESIAN_POINT('Ctrl Pts',(-0.230732053081106,-0.00123552900682768,
-0.00230690274561076));
#36157=CARTESIAN_POINT('Ctrl Pts',(-0.230773490719382,-0.00123234130551679,
-0.0023650743467824));
#36158=CARTESIAN_POINT('Ctrl Pts',(-0.230811383628898,-0.00122912706120165,
-0.00241510364952272));
#36159=CARTESIAN_POINT('Ctrl Pts',(-0.230849276538414,-0.00122591281688652,
-0.00246513295226304));
#36160=CARTESIAN_POINT('Ctrl Pts',(-0.230882962553088,-0.00122267202956712,
-0.00250753038251587));
#36161=CARTESIAN_POINT('Ctrl Pts',(-0.230921436096799,-0.00121884911930227,
-0.0025539076517966));
#36162=CARTESIAN_POINT('Origin',(-0.234,-0.00203858085746875,0.));
#36163=CARTESIAN_POINT('',(-0.230921436096816,0.0162188492999508,0.00255390765181756));
#36164=CARTESIAN_POINT('',(-0.230921436098932,0.0163191151589042,0.00255390765437054));
#36165=CARTESIAN_POINT('',(-0.2309214360969,-0.00203858085746875,0.00255390765191894));
#36166=CARTESIAN_POINT('',(-0.230644548883471,0.0163417486711327,0.00217737176535899));
#36167=CARTESIAN_POINT('Ctrl Pts',(-0.230921436078515,0.0163191146497307,
0.0025539076297574));
#36168=CARTESIAN_POINT('Ctrl Pts',(-0.230882799131686,0.0163229152747047,
0.00250733338839475));
#36169=CARTESIAN_POINT('Ctrl Pts',(-0.230847896612009,0.0163262157976892,
0.00246332973319459));
#36170=CARTESIAN_POINT('Ctrl Pts',(-0.230810936306616,0.0163293288041934,
0.00241451294457891));
#36171=CARTESIAN_POINT('Ctrl Pts',(-0.230773975995361,0.0163324418111914,
0.00236569614822039));
#36172=CARTESIAN_POINT('Ctrl Pts',(-0.230735375247888,0.0163353673016496,
0.00231172583822521));
#36173=CARTESIAN_POINT('Ctrl Pts',(-0.230710890465089,0.0163371675185938,
0.00227634761566747));
#36174=CARTESIAN_POINT('Ctrl Pts',(-0.230686405682289,0.016338967735538,
0.00224096939310972));
#36175=CARTESIAN_POINT('Ctrl Pts',(-0.23067527434207,0.0163396426789682,
0.00222472140771315));
#36176=CARTESIAN_POINT('Ctrl Pts',(-0.230644548883471,0.0163417486711327,
0.00217737176535899));
#36177=CARTESIAN_POINT('',(-0.23017792818303,0.0163799682805405,0.00117973176015849));
#36178=CARTESIAN_POINT('Ctrl Pts',(-0.230644548883471,0.0163417486711327,
0.00217737176535899));
#36179=CARTESIAN_POINT('Ctrl Pts',(-0.230613823424872,0.0163438546632971,
0.00213002212300482));
#36180=CARTESIAN_POINT('Ctrl Pts',(-0.230564811116794,0.016347391704196,
0.00205070172250556));
#36181=CARTESIAN_POINT('Ctrl Pts',(-0.230526711864591,0.0163502733457859,
0.00198400340937967));
#36182=CARTESIAN_POINT('Ctrl Pts',(-0.230488612612389,0.0163531549873758,
0.00191730509625378));
#36183=CARTESIAN_POINT('Ctrl Pts',(-0.230460264039213,0.0163553812296567,
0.00186386391325319));
#36184=CARTESIAN_POINT('Ctrl Pts',(-0.230432675642059,0.0163575938684977,
0.0018094742123716));
#36185=CARTESIAN_POINT('Ctrl Pts',(-0.230405087244905,0.0163598065073388,
0.00175508451149002));
#36186=CARTESIAN_POINT('Ctrl Pts',(-0.230378570075895,0.0163620055427398,
0.00169961758389459));
#36187=CARTESIAN_POINT('Ctrl Pts',(-0.230354383004713,0.0163640585945882,
0.00164604882177632));
#36188=CARTESIAN_POINT('Ctrl Pts',(-0.23033019593353,0.0163661116464366,
0.00159248005965805));
#36189=CARTESIAN_POINT('Ctrl Pts',(-0.230308335985599,0.0163680187147322,
0.00154079438187499));
#36190=CARTESIAN_POINT('Ctrl Pts',(-0.230289909159302,0.0163696675240572,
0.00149506720710742));
#36191=CARTESIAN_POINT('Ctrl Pts',(-0.230271482333005,0.0163713163333821,
0.00144934003233984));
#36192=CARTESIAN_POINT('Ctrl Pts',(-0.230256225286953,0.0163727068837364,
0.00140968639978936));
#36193=CARTESIAN_POINT('Ctrl Pts',(-0.23023743558141,0.0163744206569048,
0.00135761150406173));
#36194=CARTESIAN_POINT('Ctrl Pts',(-0.230218645875867,0.0163761344300732,
0.00130553660833409));
#36195=CARTESIAN_POINT('Ctrl Pts',(-0.230196798000944,0.0163781714260557,
0.0012408658261171));
#36196=CARTESIAN_POINT('Ctrl Pts',(-0.23017792818303,0.0163799682805405,
0.00117973176015849));
#36197=CARTESIAN_POINT('',(-0.230090093999453,0.0163884973145555,-0.000844177153733135));
#36198=CARTESIAN_POINT('Ctrl Pts',(-0.23017792818303,0.0163799682805405,
0.00117973176015849));
#36199=CARTESIAN_POINT('Ctrl Pts',(-0.230159058365117,0.0163817651350253,
0.00111859769419988));
#36200=CARTESIAN_POINT('Ctrl Pts',(-0.230142844552385,0.0163833218480123,
0.00106109505904679));
#36201=CARTESIAN_POINT('Ctrl Pts',(-0.230127856832223,0.0163847761298856,
0.00100324836817062));
#36202=CARTESIAN_POINT('Ctrl Pts',(-0.230097881391899,0.0163876846936321,
0.000887554986418291));
#36203=CARTESIAN_POINT('Ctrl Pts',(-0.230073193247974,0.0163901835329237,
0.000770398923136304));
#36204=CARTESIAN_POINT('Ctrl Pts',(-0.230054246319006,0.0163921725057037,
0.000656527142561015));
#36205=CARTESIAN_POINT('Ctrl Pts',(-0.230016352461069,0.0163961504512636,
0.000428783581410437));
#36206=CARTESIAN_POINT('Ctrl Pts',(-0.229999991480161,0.016398088930777,
0.000214343196413871));
#36207=CARTESIAN_POINT('Ctrl Pts',(-0.230000000003158,0.0163980879658518,
-1.58935424071983E-7));
#36208=CARTESIAN_POINT('Ctrl Pts',(-0.230000008526154,0.0163980870009266,
-0.000214661067262015));
#36209=CARTESIAN_POINT('Ctrl Pts',(-0.230016386700467,0.0163961465915627,
-0.000429102401853301));
#36210=CARTESIAN_POINT('Ctrl Pts',(-0.230054299127932,0.0163921669423355,
-0.000656844447461795));
#36211=CARTESIAN_POINT('Ctrl Pts',(-0.230064575285859,0.0163910882589937,
-0.000718573895662374));
#36212=CARTESIAN_POINT('Ctrl Pts',(-0.230076538590272,0.0163898597567301,
-0.000781268320935413));
#36213=CARTESIAN_POINT('Ctrl Pts',(-0.230090093999453,0.0163884973145555,
-0.000844177153733135));
#36214=CARTESIAN_POINT('',(-0.230631848315212,0.0163426240801819,-0.00215767333678148));
#36215=CARTESIAN_POINT('Ctrl Pts',(-0.230090093999453,0.0163884973145555,
-0.000844177153733135));
#36216=CARTESIAN_POINT('Ctrl Pts',(-0.230101587183355,0.016387346488129,
-0.00089730847127423));
#36217=CARTESIAN_POINT('Ctrl Pts',(-0.230114209594691,0.0163861000978827,
-0.000950593768044107));
#36218=CARTESIAN_POINT('Ctrl Pts',(-0.230127941498946,0.0163847677135248,
-0.00100357509156707));
#36219=CARTESIAN_POINT('Ctrl Pts',(-0.230142935925125,0.016383312828716,
-0.00106142755905526));
#36220=CARTESIAN_POINT('Ctrl Pts',(-0.230159157927828,0.0163817554101476,
-0.00111893912508747));
#36221=CARTESIAN_POINT('Ctrl Pts',(-0.23017803110707,0.0163799584198563,
-0.00118006515984195));
#36222=CARTESIAN_POINT('Ctrl Pts',(-0.230196904286312,0.0163781614295651,
-0.00124119119459644));
#36223=CARTESIAN_POINT('Ctrl Pts',(-0.230218749095649,0.016376124867551,
-0.00130583742982536));
#36224=CARTESIAN_POINT('Ctrl Pts',(-0.230237558684458,0.0163744093400124,
-0.00135795263065568));
#36225=CARTESIAN_POINT('Ctrl Pts',(-0.230256368273268,0.0163726938124738,
-0.001410067831486));
#36226=CARTESIAN_POINT('Ctrl Pts',(-0.230271669721095,0.0163712993194106,
-0.00144982608584323));
#36227=CARTESIAN_POINT('Ctrl Pts',(-0.23029014866085,0.0163696461109798,
-0.00149566140600394));
#36228=CARTESIAN_POINT('Ctrl Pts',(-0.230308627600605,0.0163679929025489,
-0.00154149672616465));
#36229=CARTESIAN_POINT('Ctrl Pts',(-0.23033054679533,0.0163660809787502,
-0.00159329421301259));
#36230=CARTESIAN_POINT('Ctrl Pts',(-0.230354813073543,0.0163640217650164,
-0.00164700099307509));
#36231=CARTESIAN_POINT('Ctrl Pts',(-0.230379079351757,0.0163619625512826,
-0.0017007077731376));
#36232=CARTESIAN_POINT('Ctrl Pts',(-0.23040569672531,0.0163597560476136,
-0.00175633864242895));
#36233=CARTESIAN_POINT('Ctrl Pts',(-0.230433388436071,0.0163575363021224,
-0.001810878778949));
#36234=CARTESIAN_POINT('Ctrl Pts',(-0.230461080146832,0.0163553165566312,
-0.00186541891546905));
#36235=CARTESIAN_POINT('Ctrl Pts',(-0.230489531202867,0.0163530835693178,
-0.00191899870747605));
#36236=CARTESIAN_POINT('Ctrl Pts',(-0.230527819241536,0.0163501897222977,
-0.00198594077971958));
#36237=CARTESIAN_POINT('Ctrl Pts',(-0.230560638422925,0.016347709216804,
-0.00204332120681471));
#36238=CARTESIAN_POINT('Ctrl Pts',(-0.230601552207351,0.0163447431562081,
-0.00211004493906512));
#36239=CARTESIAN_POINT('Ctrl Pts',(-0.230631848315212,0.0163426240801819,
-0.00215767333678148));
#36240=CARTESIAN_POINT('Ctrl Pts',(-0.230631848315212,0.0163426240801819,
-0.00215767333678148));
#36241=CARTESIAN_POINT('Ctrl Pts',(-0.230636936996691,0.0163422709658182,
-0.00216558384271426));
#36242=CARTESIAN_POINT('Ctrl Pts',(-0.23064169730074,0.0163419413701478,
-0.00217298586863137));
#36243=CARTESIAN_POINT('Ctrl Pts',(-0.230646077312613,0.0163416414589317,
-0.00217972535128352));
#36244=CARTESIAN_POINT('Ctrl Pts',(-0.230676742231324,0.0163395417493127,
-0.00222690917034205));
#36245=CARTESIAN_POINT('Ctrl Pts',(-0.230687445717667,0.0163388970368014,
-0.00224249829545137));
#36246=CARTESIAN_POINT('Ctrl Pts',(-0.230711699381587,0.0163371108294283,
-0.00227751598083233));
#36247=CARTESIAN_POINT('Ctrl Pts',(-0.230735953045507,0.0163353246220552,
-0.00231253366621329));
#36248=CARTESIAN_POINT('Ctrl Pts',(-0.230774523891339,0.0163323969198203,
-0.00236643834730859));
#36249=CARTESIAN_POINT('Ctrl Pts',(-0.230811381785659,0.0163292905470285,
-0.00241510121592747));
#36250=CARTESIAN_POINT('Ctrl Pts',(-0.230848239674129,0.0163261841747298,
-0.00246376407682237));
#36251=CARTESIAN_POINT('Ctrl Pts',(-0.230882962005671,0.016322899131931,
-0.00250752972203446));
#36252=CARTESIAN_POINT('Ctrl Pts',(-0.23092143607858,0.0163191144773501,
-0.00255390762983496));
#36253=CARTESIAN_POINT('',(-0.230686015407516,0.016238804421674,-0.00223997904471846));
#36254=CARTESIAN_POINT('Ctrl Pts',(-0.230921436096798,0.0162188491192965,
-0.0025539076517962));
#36255=CARTESIAN_POINT('Ctrl Pts',(-0.230882799397051,0.0162226882415039,
-0.00250733370888625));
#36256=CARTESIAN_POINT('Ctrl Pts',(-0.230848935196512,0.0162259446534774,
-0.00246470143542876));
#36257=CARTESIAN_POINT('Ctrl Pts',(-0.230810937450868,0.0162291657062486,
-0.00241451445589385));
#36258=CARTESIAN_POINT('Ctrl Pts',(-0.230772939705224,0.0162323867590198,
-0.00236432747635895));
#36259=CARTESIAN_POINT('Ctrl Pts',(-0.230731466785859,0.0162355724525887,
-0.00230607839344163));
#36260=CARTESIAN_POINT('Ctrl Pts',(-0.230710893420252,0.0162370807338301,
-0.00227635188559671));
#36261=CARTESIAN_POINT('Ctrl Pts',(-0.230700606737449,0.0162378348744508,
-0.00226148863167426));
#36262=CARTESIAN_POINT('Ctrl Pts',(-0.23069539536208,0.0162381696619895,
-0.00225385641780176));
#36263=CARTESIAN_POINT('Ctrl Pts',(-0.230686015407516,0.016238804421674,
-0.00223997904471846));
#36264=CARTESIAN_POINT('',(-0.230177916609458,0.0162799293327684,-0.00117969426367131));
#36265=CARTESIAN_POINT('Ctrl Pts',(-0.230686015407516,0.016238804421674,
-0.00223997904471846));
#36266=CARTESIAN_POINT('Ctrl Pts',(-0.230676635452952,0.0162394391813584,
-0.00222610167163516));
#36267=CARTESIAN_POINT('Ctrl Pts',(-0.230663125022571,0.0162403739131886,
-0.00220595658219773));
#36268=CARTESIAN_POINT('Ctrl Pts',(-0.230646074215495,0.0162415661152585,
-0.00217972058576994));
#36269=CARTESIAN_POINT('Ctrl Pts',(-0.230611972601341,0.0162439505193984,
-0.00212724859291435));
#36270=CARTESIAN_POINT('Ctrl Pts',(-0.230564381958858,0.0162473648044977,
-0.00204995030269808));
#36271=CARTESIAN_POINT('Ctrl Pts',(-0.230526713368632,0.0162502035196495,
-0.00198400604241944));
#36272=CARTESIAN_POINT('Ctrl Pts',(-0.230489044778405,0.0162530422348013,
-0.0019180617821408));
#36273=CARTESIAN_POINT('Ctrl Pts',(-0.230460339614821,0.0162553053800055,
-0.00186401601710155));
#36274=CARTESIAN_POINT('Ctrl Pts',(-0.230432634064514,0.0162575330248551,
-0.00180939224115048));
#36275=CARTESIAN_POINT('Ctrl Pts',(-0.230404928514207,0.0162597606697047,
-0.00175476846519941));
#36276=CARTESIAN_POINT('Ctrl Pts',(-0.230378492308048,0.0162619528141995,
-0.00169944973877708));
#36277=CARTESIAN_POINT('Ctrl Pts',(-0.230354332276493,0.0162640045257515,
-0.00164593646589942));
#36278=CARTESIAN_POINT('Ctrl Pts',(-0.230330172244938,0.0162660562373035,
-0.00159242319302175));
#36279=CARTESIAN_POINT('Ctrl Pts',(-0.230308296040165,0.0162679675159127,
-0.00154069825426019));
#36280=CARTESIAN_POINT('Ctrl Pts',(-0.230289875125128,0.0162696180223388,
-0.00149498274667557));
#36281=CARTESIAN_POINT('Ctrl Pts',(-0.230271454210092,0.016271268528765,
-0.00144926723909096));
#36282=CARTESIAN_POINT('Ctrl Pts',(-0.230256221884176,0.0162726582630083,
-0.00140967677595122));
#36283=CARTESIAN_POINT('Ctrl Pts',(-0.230237437189646,0.0162743735146171,
-0.00135761596121328));
#36284=CARTESIAN_POINT('Ctrl Pts',(-0.230218652495116,0.0162760887662258,
-0.00130555514647534));
#36285=CARTESIAN_POINT('Ctrl Pts',(-0.230196792077928,0.0162781295352002,
-0.00124084876509567));
#36286=CARTESIAN_POINT('Ctrl Pts',(-0.230177916609458,0.0162799293327684,
-0.00117969426367131));
#36287=CARTESIAN_POINT('',(-0.230089137337594,0.0162885651963867,0.000839734026817373));
#36288=CARTESIAN_POINT('Ctrl Pts',(-0.230177916609458,0.0162799293327684,
-0.00117969426367131));
#36289=CARTESIAN_POINT('Ctrl Pts',(-0.230159041140988,0.0162817291303366,
-0.00111853976224696));
#36290=CARTESIAN_POINT('Ctrl Pts',(-0.230142827172492,0.0162832879564987,
-0.00106103219059277));
#36291=CARTESIAN_POINT('Ctrl Pts',(-0.230127839091737,0.0162847442853598,
-0.00100317989439576));
#36292=CARTESIAN_POINT('Ctrl Pts',(-0.230097862930227,0.0162876569430821,
-0.000887475302001748));
#36293=CARTESIAN_POINT('Ctrl Pts',(-0.230073174820682,0.0162901596116007,
-0.000770305092210906));
#36294=CARTESIAN_POINT('Ctrl Pts',(-0.230054230521423,0.0162921515938631,
-0.000656432191416348));
#36295=CARTESIAN_POINT('Ctrl Pts',(-0.230016341922904,0.0162961355583879,
-0.000428686389827232));
#36296=CARTESIAN_POINT('Ctrl Pts',(-0.229999991618952,0.0162980767778882,
-0.000214296251682201));
#36297=CARTESIAN_POINT('Ctrl Pts',(-0.230000000003057,0.0162980758241512,
1.56381474666943E-7));
#36298=CARTESIAN_POINT('Ctrl Pts',(-0.230000008387162,0.0162980748704142,
0.000214609014631535));
#36299=CARTESIAN_POINT('Ctrl Pts',(-0.230016375665422,0.0162961317434399,
0.000429001096517139));
#36300=CARTESIAN_POINT('Ctrl Pts',(-0.230054282773425,0.0162921460779994,
0.000656746197485573));
#36301=CARTESIAN_POINT('Ctrl Pts',(-0.230064320313722,0.016291090701328,
0.000717051526717664));
#36302=CARTESIAN_POINT('Ctrl Pts',(-0.230075968745583,0.0162898921112937,
0.000778281439696839));
#36303=CARTESIAN_POINT('Ctrl Pts',(-0.230089137337594,0.0162885651963867,
0.000839734026817373));
#36304=CARTESIAN_POINT('',(-0.230625305120942,0.0162430239031887,0.00214742507977825));
#36305=CARTESIAN_POINT('Ctrl Pts',(-0.230089137337594,0.0162885651963867,
0.000839734026817373));
#36306=CARTESIAN_POINT('Ctrl Pts',(-0.230100879275725,0.0162873865419408,
0.000894313659151995));
#36307=CARTESIAN_POINT('Ctrl Pts',(-0.230113815651244,0.0162861066368743,
0.00094906972951125));
#36308=CARTESIAN_POINT('Ctrl Pts',(-0.230127923151515,0.0162847359159103,
0.00100350429965659));
#36309=CARTESIAN_POINT('Ctrl Pts',(-0.230142917928165,0.0162832789848943,
0.00106136247478748));
#36310=CARTESIAN_POINT('Ctrl Pts',(-0.230159140064727,0.0162817194552044,
0.00111887903837501));
#36311=CARTESIAN_POINT('Ctrl Pts',(-0.230178018968344,0.0162799195126125,
0.00118002584448998));
#36312=CARTESIAN_POINT('Ctrl Pts',(-0.230196897871962,0.0162781195700206,
0.00124117265060494));
#36313=CARTESIAN_POINT('Ctrl Pts',(-0.230218755421485,0.0162760792145265,
0.0013058550927437));
#36314=CARTESIAN_POINT('Ctrl Pts',(-0.230237559817246,0.0162743622278125,
0.00135795576923366));
#36315=CARTESIAN_POINT('Ctrl Pts',(-0.230256364213006,0.0162726452410985,
0.00141005644572361));
#36316=CARTESIAN_POINT('Ctrl Pts',(-0.230271640299325,0.0162712516231645,
0.00144975005051676));
#36317=CARTESIAN_POINT('Ctrl Pts',(-0.230290114089152,0.0162695966319987,
0.001495575651209));
#36318=CARTESIAN_POINT('Ctrl Pts',(-0.230308587878978,0.0162679416408329,
0.00154140125190124));
#36319=CARTESIAN_POINT('Ctrl Pts',(-0.230330525795565,0.0162660252764353,
0.00159324330383135));
#36320=CARTESIAN_POINT('Ctrl Pts',(-0.230354762071464,0.0162639676803474,
0.00164688810924254));
#36321=CARTESIAN_POINT('Ctrl Pts',(-0.230378998347364,0.0162619100842594,
0.00170053291465374));
#36322=CARTESIAN_POINT('Ctrl Pts',(-0.230405525183997,0.0162597112564811,
0.00175599769668587));
#36323=CARTESIAN_POINT('Ctrl Pts',(-0.230433347288488,0.0162574753728585,
0.00181079773455379));
#36324=CARTESIAN_POINT('Ctrl Pts',(-0.23046116939298,0.0162552394892359,
0.00186559777242172));
#36325=CARTESIAN_POINT('Ctrl Pts',(-0.230490017754343,0.0162529665497689,
0.00191984963302185));
#36326=CARTESIAN_POINT('Ctrl Pts',(-0.230527822456637,0.0162501197095321,
0.00198594640092935));
#36327=CARTESIAN_POINT('Ctrl Pts',(-0.230558008612418,0.0162478465753012,
0.00203872309831363));
#36328=CARTESIAN_POINT('Ctrl Pts',(-0.230594518257034,0.0162452075424427,
0.00209870295150882));
#36329=CARTESIAN_POINT('Ctrl Pts',(-0.230625305120942,0.0162430239031887,
0.00214742507977825));
#36330=CARTESIAN_POINT('Ctrl Pts',(-0.230625305120942,0.0162430239031887,
0.00214742507977825));
#36331=CARTESIAN_POINT('Ctrl Pts',(-0.230633139129668,0.0162424727844128,
0.00215968084725818));
#36332=CARTESIAN_POINT('Ctrl Pts',(-0.230640560869481,0.0162419506734878,
0.00217125015931671));
#36333=CARTESIAN_POINT('Ctrl Pts',(-0.230647428482022,0.0162414707739622,
0.00218180297388311));
#36334=CARTESIAN_POINT('Ctrl Pts',(-0.230664467693318,0.0162402800967991,
0.00220798552802012));
#36335=CARTESIAN_POINT('Ctrl Pts',(-0.230677926924196,0.0162393492663061,
0.00222802700809956));
#36336=CARTESIAN_POINT('Ctrl Pts',(-0.230687201540453,0.0162387219019087,
0.00224173289363862));
#36337=CARTESIAN_POINT('Ctrl Pts',(-0.23069647615671,0.0162380945375114,
0.00225543877917767));
#36338=CARTESIAN_POINT('Ctrl Pts',(-0.230701528573552,0.0162377706392097,
0.00226283132146126));
#36339=CARTESIAN_POINT('Ctrl Pts',(-0.230711703459589,0.0162370234270096,
0.00227752186868137));
#36340=CARTESIAN_POINT('Ctrl Pts',(-0.230732053231664,0.0162355290026094,
0.00230690296312161));
#36341=CARTESIAN_POINT('Ctrl Pts',(-0.230773490818101,0.0162323413226155,
0.00236507448024538));
#36342=CARTESIAN_POINT('Ctrl Pts',(-0.230811383701533,0.0162291271099321,
0.00241510374542183));
#36343=CARTESIAN_POINT('Ctrl Pts',(-0.230849276584965,0.0162259128972488,
0.00246513301059828));
#36344=CARTESIAN_POINT('Ctrl Pts',(-0.230882962605203,0.0162226721518758,
0.0025075304453366));
#36345=CARTESIAN_POINT('Ctrl Pts',(-0.230921436096799,0.0162188492995221,
0.0025539076517966));
#36346=CARTESIAN_POINT('Origin',(-0.238,-0.00203858085746875,0.0110866403454819));
#36347=CARTESIAN_POINT('',(-0.235510394140372,0.001086028911646,0.00808558792816448));
#36348=CARTESIAN_POINT('Ctrl Pts',(-0.2309214360969,-0.00131911464792199,
0.00255390765191894));
#36349=CARTESIAN_POINT('Ctrl Pts',(-0.23174153296916,-0.00124041124463224,
0.00354247927317125));
#36350=CARTESIAN_POINT('Ctrl Pts',(-0.233359728852528,-0.00077441369596115,
0.00549310557359274));
#36351=CARTESIAN_POINT('Ctrl Pts',(-0.234843968024857,0.000344657188193435,
0.00728225606854703));
#36352=CARTESIAN_POINT('Ctrl Pts',(-0.235510394140372,0.001086028911646,
0.00808558792816448));
#36353=CARTESIAN_POINT('',(-0.23718847822691,0.00385255096193961,0.0101084054295328));
#36354=CARTESIAN_POINT('Ctrl Pts',(-0.235510394140372,0.001086028911646,
0.00808558792816448));
#36355=CARTESIAN_POINT('Ctrl Pts',(-0.236176820255887,0.00182740063509858,
0.00888891978778193));
#36356=CARTESIAN_POINT('Ctrl Pts',(-0.236767552900753,0.00275060863992643,
0.00960100825953967));
#36357=CARTESIAN_POINT('Ctrl Pts',(-0.23718847822691,0.00385255096193961,
0.0101084054295328));
#36358=CARTESIAN_POINT('',(-0.237859981300301,0.00751096248998218,0.0109178572204036));
#36359=CARTESIAN_POINT('Ctrl Pts',(-0.23718847822691,0.00385255096193961,
0.0101084054295328));
#36360=CARTESIAN_POINT('Ctrl Pts',(-0.237609403553067,0.00495449328395277,
0.010615802599526));
#36361=CARTESIAN_POINT('Ctrl Pts',(-0.237860521560515,0.00623516992315125,
0.0109185084677545));
#36362=CARTESIAN_POINT('Ctrl Pts',(-0.237859981300301,0.00751096248998218,
0.0109178572204036));
#36363=CARTESIAN_POINT('Ctrl Pts',(-0.237859981300301,0.00751096248998218,
0.0109178572204036));
#36364=CARTESIAN_POINT('Ctrl Pts',(-0.237859441040087,0.00878675505681313,
0.0109172059730527));
#36365=CARTESIAN_POINT('Ctrl Pts',(-0.237355043984334,0.0113285720457399,
0.0103091892471919));
#36366=CARTESIAN_POINT('Ctrl Pts',(-0.2355790521135,0.0141062321617645,
0.00816835049695678));
#36367=CARTESIAN_POINT('Ctrl Pts',(-0.233347521760492,0.0157787640062935,
0.00547839074517056));
#36368=CARTESIAN_POINT('Ctrl Pts',(-0.23174108105572,0.0162404546140525,
0.00354193452191338));
#36369=CARTESIAN_POINT('Ctrl Pts',(-0.2309214360969,0.0163191146479222,
0.00255390765191895));
#36370=CARTESIAN_POINT('Ctrl Pts',(-0.2309214360969,0.016218849299512,0.00255390765191894));
#36371=CARTESIAN_POINT('Ctrl Pts',(-0.231731717357689,0.0161403008067932,
0.00353064721372319));
#36372=CARTESIAN_POINT('Ctrl Pts',(-0.23253100953097,0.0159094319151459,
0.00449414016964269));
#36373=CARTESIAN_POINT('Ctrl Pts',(-0.233297219375807,0.0155172940805772,
0.00541775460368186));
#36374=CARTESIAN_POINT('Ctrl Pts',(-0.234063429220644,0.0151251562460085,
0.00634136903772102));
#36375=CARTESIAN_POINT('Ctrl Pts',(-0.234796556737038,0.0145717494685186,
0.00722510494987985));
#36376=CARTESIAN_POINT('Ctrl Pts',(-0.235454844320089,0.0138387602641205,
0.00801862635599526));
#36377=CARTESIAN_POINT('Ctrl Pts',(-0.23611313190314,0.0131057710597224,
0.00881214776211065));
#36378=CARTESIAN_POINT('Ctrl Pts',(-0.236696579552848,0.0121931994284161,
0.00951545466218262));
#36379=CARTESIAN_POINT('Ctrl Pts',(-0.237112283509665,0.0111042149244282,
0.0100165578226166));
#36380=CARTESIAN_POINT('Ctrl Pts',(-0.237527987466483,0.0100152304204403,
0.0105176609830505));
#36381=CARTESIAN_POINT('Ctrl Pts',(-0.237775947730408,0.0087498330437706,
0.0108165604038465));
#36382=CARTESIAN_POINT('Ctrl Pts',(-0.237775416984309,0.0074892317112278,
0.0108159206251214));
#36383=CARTESIAN_POINT('Ctrl Pts',(-0.237774886238211,0.006228630378685,
0.0108152808463964));
#36384=CARTESIAN_POINT('Ctrl Pts',(-0.237525864482087,0.00497282509026909,
0.0105151018681504));
#36385=CARTESIAN_POINT('Ctrl Pts',(-0.237109010658239,0.00388732421957286,
0.0100126126203483));
#36386=CARTESIAN_POINT('Ctrl Pts',(-0.236692156834391,0.00280182334887665,
0.00951012337254628));
#36387=CARTESIAN_POINT('Ctrl Pts',(-0.236107470942817,0.00188662689590011,
0.00880532385518818));
#36388=CARTESIAN_POINT('Ctrl Pts',(-0.235447722393476,0.00115331852706932,
0.00801004135247146));
#36389=CARTESIAN_POINT('Ctrl Pts',(-0.234787973844134,0.000420010158238511,
0.00721475884975473));
#36390=CARTESIAN_POINT('Ctrl Pts',(-0.234053162637025,-0.000131410126446554,
0.00632899336167939));
#36391=CARTESIAN_POINT('Ctrl Pts',(-0.233288987015657,-0.000521498676355057,
0.00540783104721498));
#36392=CARTESIAN_POINT('Ctrl Pts',(-0.23252481139429,-0.000911587226263559,
0.00448666873275056));
#36393=CARTESIAN_POINT('Ctrl Pts',(-0.231731271358665,-0.0011403440413955,
0.00353010959189706));
#36394=CARTESIAN_POINT('Ctrl Pts',(-0.2309214360969,-0.00121884929951176,
0.00255390765191896));
#36395=CARTESIAN_POINT('Origin',(-0.194168411395185,0.0075,-0.0165));
#36396=CARTESIAN_POINT('',(-0.192751468456974,0.0155452250459276,-0.0056));
#36397=CARTESIAN_POINT('Ctrl Pts',(-0.186019885831704,0.00807870931483181,
-0.00979684103423184));
#36398=CARTESIAN_POINT('Ctrl Pts',(-0.186089762480249,0.00906260833433668,
-0.00973982032171833));
#36399=CARTESIAN_POINT('Ctrl Pts',(-0.186581784748698,0.0109343901050088,
-0.00933928969553343));
#36400=CARTESIAN_POINT('Ctrl Pts',(-0.188116978636712,0.0131929004294505,
-0.00813962307738));
#36401=CARTESIAN_POINT('Ctrl Pts',(-0.190152702745521,0.0147631592433591,
-0.00671673740186432));
#36402=CARTESIAN_POINT('Ctrl Pts',(-0.191807671769535,0.0153790014730954,
-0.0058522182261825));
#36403=CARTESIAN_POINT('Ctrl Pts',(-0.192751468456974,0.0155452250459276,
-0.0056));
#36404=CARTESIAN_POINT('',(-0.192176438048886,0.0154224627179558,-0.00559999999999961));
#36405=CARTESIAN_POINT('Origin',(-0.194168411395185,0.0075,-0.0056));
#36406=CARTESIAN_POINT('Ctrl Pts',(-0.192176438048885,0.0154224627179556,
-0.00559999999999953));
#36407=CARTESIAN_POINT('Ctrl Pts',(-0.191343963173299,0.0152131505605284,
-0.00591304953429593));
#36408=CARTESIAN_POINT('Ctrl Pts',(-0.190604005308188,0.0148933286596848,
-0.00633980824174457));
#36409=CARTESIAN_POINT('Ctrl Pts',(-0.189928056093887,0.0144823257548366,
-0.00677375538217563));
#36410=CARTESIAN_POINT('Ctrl Pts',(-0.189924240326155,0.0144800056225113,
-0.00677620503587909));
#36411=CARTESIAN_POINT('Ctrl Pts',(-0.189920426601425,0.0144776825774865,
-0.00677865492356244));
#36412=CARTESIAN_POINT('Ctrl Pts',(-0.189916614915206,0.0144753566233282,
-0.00678110502583209));
#36413=CARTESIAN_POINT('Ctrl Pts',(-0.189582813506844,0.0142716654669213,
-0.00699566822470287));
#36414=CARTESIAN_POINT('Ctrl Pts',(-0.189264648232927,0.014045660164331,
-0.00721187875958755));
#36415=CARTESIAN_POINT('Ctrl Pts',(-0.188963035346507,0.0137964688081976,
-0.00742469482413229));
#36416=CARTESIAN_POINT('Ctrl Pts',(-0.188657978335366,0.0135444319300434,
-0.00763994104037826));
#36417=CARTESIAN_POINT('Ctrl Pts',(-0.188369854070253,0.0132686788741525,
-0.00785171201844442));
#36418=CARTESIAN_POINT('Ctrl Pts',(-0.188099546793334,0.0129683186589328,
-0.00805477844807097));
#36419=CARTESIAN_POINT('Ctrl Pts',(-0.188093714462902,0.0129618378862222,
-0.00805915994504986));
#36420=CARTESIAN_POINT('Ctrl Pts',(-0.188087890440239,0.012955345674165,
-0.00806353734695464));
#36421=CARTESIAN_POINT('Ctrl Pts',(-0.188082074735716,0.0129488420160566,
-0.00806791060250755));
#36422=CARTESIAN_POINT('Ctrl Pts',(-0.187818353713641,0.0126539248040995,
-0.00826622181649803));
#36423=CARTESIAN_POINT('Ctrl Pts',(-0.187571750207195,0.0123354620106826,
-0.00845600236765789));
#36424=CARTESIAN_POINT('Ctrl Pts',(-0.187347312169252,0.0119951777506216,
-0.00863133901481845));
#36425=CARTESIAN_POINT('Ctrl Pts',(-0.187117924714299,0.0116473893761944,
-0.00881054227118578));
#36426=CARTESIAN_POINT('Ctrl Pts',(-0.186911700916772,0.0112768070043132,
-0.00897465664894075));
#36427=CARTESIAN_POINT('Ctrl Pts',(-0.186733851221639,0.0108854486190338,
-0.00911727516815564));
#36428=CARTESIAN_POINT('Ctrl Pts',(-0.186727815762721,0.0108721675872344,
-0.00912211503146282));
#36429=CARTESIAN_POINT('Ctrl Pts',(-0.186721813013436,0.0108588627757301,
-0.00912692993314436));
#36430=CARTESIAN_POINT('Ctrl Pts',(-0.186715843136615,0.0108455341927419,
-0.00913171966304142));
#36431=CARTESIAN_POINT('Ctrl Pts',(-0.18654589585667,0.0104661031772941,
-0.0092680711476793));
#36432=CARTESIAN_POINT('Ctrl Pts',(-0.18640252125758,0.0100674585344605,
-0.00938407744564779));
#36433=CARTESIAN_POINT('Ctrl Pts',(-0.186289553083222,0.00965454859173225,
-0.00947595892755243));
#36434=CARTESIAN_POINT('Ctrl Pts',(-0.186172616583594,0.00922713402441014,
-0.00957106800526971));
#36435=CARTESIAN_POINT('Ctrl Pts',(-0.18608819762884,0.0087843421088577,
-0.00964038068192425));
#36436=CARTESIAN_POINT('Ctrl Pts',(-0.186041757909902,0.00833112640840616,
-0.00967861021014855));
#36437=CARTESIAN_POINT('Origin',(-0.194168411395185,0.0075,-0.0165));
#36438=CARTESIAN_POINT('',(-0.192436879758486,-0.000483789065104605,-0.00550698406469574));
#36439=CARTESIAN_POINT('Ctrl Pts',(-0.186041751543844,0.00666887245842392,
-0.00967861584559627));
#36440=CARTESIAN_POINT('Ctrl Pts',(-0.186136921847663,0.00573830927961182,
-0.00960028215025333));
#36441=CARTESIAN_POINT('Ctrl Pts',(-0.186644248953973,0.00396647107157331,
-0.00918383236544583));
#36442=CARTESIAN_POINT('Ctrl Pts',(-0.188108094123016,0.00183866584854421,
-0.00802791806514813));
#36443=CARTESIAN_POINT('Ctrl Pts',(-0.190013954849379,0.000329756393205286,
-0.00666415905021552));
#36444=CARTESIAN_POINT('Ctrl Pts',(-0.191565762541839,-0.000294497235608542,
-0.0057981387366561));
#36445=CARTESIAN_POINT('Ctrl Pts',(-0.192436909186995,-0.000483437444660073,
-0.00550752136853039));
#36446=CARTESIAN_POINT('',(-0.192760058267355,-0.000547543173123365,-0.00559773047754231));
#36447=CARTESIAN_POINT('Ctrl Pts',(-0.192436908306343,-0.000483685301569694,
-0.00550688979015399));
#36448=CARTESIAN_POINT('Ctrl Pts',(-0.192468053494424,-0.000490526619111128,
-0.00550953117142323));
#36449=CARTESIAN_POINT('Ctrl Pts',(-0.192500024893769,-0.000497440829550889,
-0.00551318415929702));
#36450=CARTESIAN_POINT('Ctrl Pts',(-0.192526030662271,-0.000502770803046763,
-0.00551666078240278));
#36451=CARTESIAN_POINT('Ctrl Pts',(-0.192552036430774,-0.000508100776542638,
-0.00552013740550853));
#36452=CARTESIAN_POINT('Ctrl Pts',(-0.192572075699273,-0.000512091086316927,
-0.00552287359103419));
#36453=CARTESIAN_POINT('Ctrl Pts',(-0.192606479483278,-0.000519208585877513,
-0.00553001925783382));
#36454=CARTESIAN_POINT('Ctrl Pts',(-0.192640883267283,-0.000526326085438099,
-0.00553716492463345));
#36455=CARTESIAN_POINT('Ctrl Pts',(-0.192689655216252,-0.0005355448116613,
-0.005549838644018));
#36456=CARTESIAN_POINT('Ctrl Pts',(-0.192718970945351,-0.000540610831352234,
-0.00556188714561741));
#36457=CARTESIAN_POINT('Ctrl Pts',(-0.192748285725897,-0.000545676687124638,
-0.0055739352573698));
#36458=CARTESIAN_POINT('Ctrl Pts',(-0.192758140601795,-0.000547978991753478,
-0.00558509522749682));
#36459=CARTESIAN_POINT('Ctrl Pts',(-0.192759751083746,-0.000548263549761792,
-0.00559775493557849));
#36460=CARTESIAN_POINT('Ctrl Pts',(-0.192759756876124,-0.000546680419632493,
-0.00559779101339214));
#36461=CARTESIAN_POINT('Ctrl Pts',(-0.191825165385716,-0.000383070526138125,
-0.00584619740310806));
#36462=CARTESIAN_POINT('Ctrl Pts',(-0.190150361296732,0.000235470075430173,
-0.00671609199811723));
#36463=CARTESIAN_POINT('Ctrl Pts',(-0.1881181529752,0.00180741978905575,
-0.00813941771993866));
#36464=CARTESIAN_POINT('Ctrl Pts',(-0.186582686445248,0.00406221483284674,
-0.00933836675647093));
#36465=CARTESIAN_POINT('Ctrl Pts',(-0.18608965503935,0.00593890428125912,
-0.00973990799217201));
#36466=CARTESIAN_POINT('Ctrl Pts',(-0.186019885804631,0.00692129106638248,
-0.00979684105632399));
#36467=CARTESIAN_POINT('Origin',(-0.194168411395185,0.0075,-0.0165));
#36468=CARTESIAN_POINT('',(-0.192176435205664,0.015422462003074,0.00560000000000063));
#36469=CARTESIAN_POINT('',(-0.192751465176479,0.0155452244681588,0.0056));
#36470=CARTESIAN_POINT('Origin',(-0.194168411395185,0.0075,0.0056));
#36471=CARTESIAN_POINT('Ctrl Pts',(-0.192751465176479,0.0155452244681588,
0.00560000000000577));
#36472=CARTESIAN_POINT('Ctrl Pts',(-0.191813525435382,0.0153800320394353,
0.0058506525472026));
#36473=CARTESIAN_POINT('Ctrl Pts',(-0.190145096657311,0.0147607301998181,
0.00672019516858599));
#36474=CARTESIAN_POINT('Ctrl Pts',(-0.188114479081028,0.0131886463237939,
0.00814201325558834));
#36475=CARTESIAN_POINT('Ctrl Pts',(-0.18658186007787,0.0109350717238122,
0.00933911242506903));
#36476=CARTESIAN_POINT('Ctrl Pts',(-0.186089586988853,0.00906013840632952,
0.00973996390275296));
#36477=CARTESIAN_POINT('Ctrl Pts',(-0.186019885767525,0.00807870841113033,
0.00979684126041441));
#36478=CARTESIAN_POINT('Ctrl Pts',(-0.186041751490874,0.00833112702364014,
0.00967861612727941));
#36479=CARTESIAN_POINT('Ctrl Pts',(-0.186134520211485,0.00923820839715129,
0.00960225940762806));
#36480=CARTESIAN_POINT('Ctrl Pts',(-0.1866209358955,0.0109672061146848,
0.00920310409653587));
#36481=CARTESIAN_POINT('Ctrl Pts',(-0.188024941690495,0.0130628185286647,
0.00809245011053833));
#36482=CARTESIAN_POINT('Ctrl Pts',(-0.189858840973276,0.0145715969653575,
0.00676934907065498));
#36483=CARTESIAN_POINT('Ctrl Pts',(-0.191348256704472,0.0152142297825336,
0.0059114330126843));
#36484=CARTESIAN_POINT('Ctrl Pts',(-0.192176435205665,0.015422462003074,
0.00560000000000055));
#36485=CARTESIAN_POINT('Origin',(-0.194168411395185,0.0075,-0.0165));
#36486=CARTESIAN_POINT('',(-0.192751465176499,-0.000545224468162299,0.0056));
#36487=CARTESIAN_POINT('Ctrl Pts',(-0.186019885794595,0.00692129120770981,
0.00979684123832483));
#36488=CARTESIAN_POINT('Ctrl Pts',(-0.186089603411304,0.00593963099051061,
0.00973995050071142));
#36489=CARTESIAN_POINT('Ctrl Pts',(-0.186581991646468,0.00406427983701678,
0.00933894129944149));
#36490=CARTESIAN_POINT('Ctrl Pts',(-0.188115599150068,0.0018103891583067,
0.00814136010924737));
#36491=CARTESIAN_POINT('Ctrl Pts',(-0.190145486706124,0.000238420026637399,
0.0067193088022048));
#36492=CARTESIAN_POINT('Ctrl Pts',(-0.191818089971992,-0.000380835957701934,
0.00584943273245187));
#36493=CARTESIAN_POINT('Ctrl Pts',(-0.192751465176499,-0.000545224468162312,
0.00559999999999996));
#36494=CARTESIAN_POINT('',(-0.192176435205669,-0.000422462003075014,0.00559999999999858));
#36495=CARTESIAN_POINT('Origin',(-0.194168411395185,0.0075,0.0056));
#36496=CARTESIAN_POINT('Ctrl Pts',(-0.192176435205669,-0.00042246200307506,
0.0055999999999985));
#36497=CARTESIAN_POINT('Ctrl Pts',(-0.191343960306167,-0.000213149521988604,
0.00591304865504301));
#36498=CARTESIAN_POINT('Ctrl Pts',(-0.190604002024927,0.000106672964546729,
0.00633980594928245));
#36499=CARTESIAN_POINT('Ctrl Pts',(-0.1899280529401,0.000517676161234743,
0.00677375261658828));
#36500=CARTESIAN_POINT('Ctrl Pts',(-0.18992423716161,0.000519996302192667,
0.00677620227499601));
#36501=CARTESIAN_POINT('Ctrl Pts',(-0.189920423426153,0.000522319355858489,
0.00677865216741516));
#36502=CARTESIAN_POINT('Ctrl Pts',(-0.189916611729236,0.000524645318665928,
0.00678110227445219));
#36503=CARTESIAN_POINT('Ctrl Pts',(-0.189582810400498,0.000728336612260569,
0.0069956652374637));
#36504=CARTESIAN_POINT('Ctrl Pts',(-0.189264645340128,0.000954341979308797,
0.00721187576892209));
#36505=CARTESIAN_POINT('Ctrl Pts',(-0.188963032722283,0.00120353333031646,
0.00742469200704865));
#36506=CARTESIAN_POINT('Ctrl Pts',(-0.188657975972295,0.00145557021195114,
0.00763993840625852));
#36507=CARTESIAN_POINT('Ctrl Pts',(-0.188369852025587,0.00173132320188797,
0.00785170974812982));
#36508=CARTESIAN_POINT('Ctrl Pts',(-0.188099545041626,0.00203168328517292,
0.00805477666142801));
#36509=CARTESIAN_POINT('Ctrl Pts',(-0.188093712707518,0.00203816406614484,
0.00805915817635282));
#36510=CARTESIAN_POINT('Ctrl Pts',(-0.188087888681199,0.00204465628647009,
0.00806353559624864));
#36511=CARTESIAN_POINT('Ctrl Pts',(-0.188082072973036,0.00205115995285323,
0.00806790886983681));
#36512=CARTESIAN_POINT('Ctrl Pts',(-0.187818352247886,0.00234607702340897,
0.00826622055425919));
#36513=CARTESIAN_POINT('Ctrl Pts',(-0.187571749013941,0.00266453960709992,
0.00845600169657692));
#36514=CARTESIAN_POINT('Ctrl Pts',(-0.187347311208284,0.00300482365954855,
0.00863133886161257));
#36515=CARTESIAN_POINT('Ctrl Pts',(-0.18711792398207,0.00335261183493064,
0.00881054265404897));
#36516=CARTESIAN_POINT('Ctrl Pts',(-0.186911700373378,0.0037231940118813,
0.00897465749008297));
#36517=CARTESIAN_POINT('Ctrl Pts',(-0.186733850811817,0.00411455227599193,
0.0091172761862189));
#36518=CARTESIAN_POINT('Ctrl Pts',(-0.186727815350132,0.0041278333197421,
0.00912211606138361));
#36519=CARTESIAN_POINT('Ctrl Pts',(-0.186721812598099,0.00414113814333308,
0.00912693097454919));
#36520=CARTESIAN_POINT('Ctrl Pts',(-0.186715842718546,0.00415446673854782,
0.00913172071554889));
#36521=CARTESIAN_POINT('Ctrl Pts',(-0.186545895573612,0.00453389762703021,
0.00926807234554705));
#36522=CARTESIAN_POINT('Ctrl Pts',(-0.186402521055717,0.00493254220704179,
0.0093840785323548));
#36523=CARTESIAN_POINT('Ctrl Pts',(-0.186289552931936,0.00534545209131564,
0.00947595982899907));
#36524=CARTESIAN_POINT('Ctrl Pts',(-0.186172616479694,0.00577286661628877,
0.00957106871898892));
#36525=CARTESIAN_POINT('Ctrl Pts',(-0.186088197541083,0.00621565849694276,
0.00964038112619589));
#36526=CARTESIAN_POINT('Ctrl Pts',(-0.186041757857161,0.0066688741095359,
0.00967861049200898));
#36527=CARTESIAN_POINT('Ctrl Pts',(-0.214908904387703,-0.000412819837817,
0.00549924362755427));
#36528=CARTESIAN_POINT('Ctrl Pts',(-0.214908556120093,-0.000352592236114761,
0.00549921336268601));
#36529=CARTESIAN_POINT('Ctrl Pts',(-0.214907538880938,-0.000324420911413182,
0.0055524795130164));
#36530=CARTESIAN_POINT('Ctrl Pts',(-0.215674937410034,-0.000408049554921536,
0.00551196603108662));
#36531=CARTESIAN_POINT('Ctrl Pts',(-0.215679462273084,-0.000347576983031315,
0.00551248972391986));
#36532=CARTESIAN_POINT('Ctrl Pts',(-0.215687503951218,-0.000319594653488507,
0.00556554866444318));
#36533=CARTESIAN_POINT('Ctrl Pts',(-0.217146688138541,-0.000581852351431893,
0.00522168675990709));
#36534=CARTESIAN_POINT('Ctrl Pts',(-0.217202909083221,-0.000525975536923966,
0.00520094287146893));
#36535=CARTESIAN_POINT('Ctrl Pts',(-0.217185883978921,-0.00049120191472606,
0.00527389759715679));
#36536=CARTESIAN_POINT('Ctrl Pts',(-0.2186746596929,-0.00100105768310807,
0.00420084069381812));
#36537=CARTESIAN_POINT('Ctrl Pts',(-0.21871285197137,-0.000931067325908604,
0.00416353700088283));
#36538=CARTESIAN_POINT('Ctrl Pts',(-0.218741209646565,-0.000905486334259725,
0.00424664847380188));
#36539=CARTESIAN_POINT('Ctrl Pts',(-0.219590982556484,-0.00126551964588667,
0.00309225172418097));
#36540=CARTESIAN_POINT('Ctrl Pts',(-0.219605834846954,-0.00117755767893153,
0.00306843118737349));
#36541=CARTESIAN_POINT('Ctrl Pts',(-0.219673746789243,-0.00116683843606389,
0.00313100836683839));
#36542=CARTESIAN_POINT('Ctrl Pts',(-0.220279879401475,-0.00140079103123703,
0.00181632836118542));
#36543=CARTESIAN_POINT('Ctrl Pts',(-0.22028722062927,-0.00130284471617747,
0.00179819091483098));
#36544=CARTESIAN_POINT('Ctrl Pts',(-0.220374608257138,-0.00130053614138798,
0.00184630444409877));
#36545=CARTESIAN_POINT('Ctrl Pts',(-0.220646769346283,-0.00147114957019175,
2.23648118814017E-6));
#36546=CARTESIAN_POINT('Ctrl Pts',(-0.220641282870505,-0.00137222086809375,
2.22945995551979E-6));
#36547=CARTESIAN_POINT('Ctrl Pts',(-0.220747708299123,-0.00137133940053372,
2.26820978703318E-6));
#36548=CARTESIAN_POINT('Ctrl Pts',(-0.220279811878892,-0.00140077718961124,
-0.00181691872560231));
#36549=CARTESIAN_POINT('Ctrl Pts',(-0.220287131950059,-0.00130282536243108,
-0.00179879800073754));
#36550=CARTESIAN_POINT('Ctrl Pts',(-0.220374539523279,-0.00130052234399854,
-0.00184690438226544));
#36551=CARTESIAN_POINT('Ctrl Pts',(-0.219591001090582,-0.00126552646557676,
-0.00309233014391036));
#36552=CARTESIAN_POINT('Ctrl Pts',(-0.219605890119876,-0.00117757433237593,
-0.00306847780184537));
#36553=CARTESIAN_POINT('Ctrl Pts',(-0.219673765728205,-0.00116684522595654,
-0.00313108606374142));
#36554=CARTESIAN_POINT('Ctrl Pts',(-0.218672731854415,-0.00100053740872269,
-0.00420257854676322));
#36555=CARTESIAN_POINT('Ctrl Pts',(-0.218710929056937,-0.000930569929864368,
-0.00416525928590887));
#36556=CARTESIAN_POINT('Ctrl Pts',(-0.218739247444545,-0.000904972171632613,
-0.00424839789736909));
#36557=CARTESIAN_POINT('Ctrl Pts',(-0.217149041162339,-0.000582287155663073,
-0.00522050661308843));
#36558=CARTESIAN_POINT('Ctrl Pts',(-0.217205169333144,-0.000526365237140583,
-0.00519985099062644));
#36559=CARTESIAN_POINT('Ctrl Pts',(-0.217188279312873,-0.000491631333474201,
-0.00527271044190245));
#36560=CARTESIAN_POINT('Ctrl Pts',(-0.215673971815205,-0.000408030032539972,
-0.00551201428777479));
#36561=CARTESIAN_POINT('Ctrl Pts',(-0.215678500833659,-0.000347560008737919,
-0.00551253254967125));
#36562=CARTESIAN_POINT('Ctrl Pts',(-0.215686520820721,-0.000319575241216833,
-0.0055655974225352));
#36563=CARTESIAN_POINT('Ctrl Pts',(-0.214909020286864,-0.000412822472739081,
-0.00549924062753781));
#36564=CARTESIAN_POINT('Ctrl Pts',(-0.214908671883726,-0.000352594303262603,
-0.00549921069462562));
#36565=CARTESIAN_POINT('Ctrl Pts',(-0.214907656887067,-0.000324423258678074,
-0.00555247701276162));
#36566=CARTESIAN_POINT('Origin',(-0.214999964648729,-0.000412689929438997,
0.00559999998627548));
#36567=CARTESIAN_POINT('Origin',(-0.214999964645672,-0.000412691090472084,
-0.0055999999862731));
#36568=CARTESIAN_POINT('Origin',(-0.195909555102848,-0.000340904441697687,
-0.00560539994565062));
#36569=CARTESIAN_POINT('Ctrl Pts',(-0.19218256102446,-0.000325378183934642,
-0.00549961012006739));
#36570=CARTESIAN_POINT('Ctrl Pts',(-0.192184843256322,-0.000306151782977641,
-0.00549964929320649));
#36571=CARTESIAN_POINT('Ctrl Pts',(-0.192188722368746,-0.000279214203787051,
-0.00550497831707243));
#36572=CARTESIAN_POINT('Ctrl Pts',(-0.192196136252542,-0.000255497248569862,
-0.0055282091349877));
#36573=CARTESIAN_POINT('Ctrl Pts',(-0.192197708531578,-0.000250467540456901,
-0.00553313574686807));
#36574=CARTESIAN_POINT('Ctrl Pts',(-0.192199363429286,-0.000245783086052327,
-0.00553879864269582));
#36575=CARTESIAN_POINT('Ctrl Pts',(-0.192200962785523,-0.000241733447191861,
-0.00554503445704357));
#36576=CARTESIAN_POINT('Origin',(-0.195910717308576,-0.000340907999567637,
0.00560539870829468));
#36577=CARTESIAN_POINT('Origin',(-0.192200813655166,-0.000326595300734187,
0.00560462943321518));
#36578=CARTESIAN_POINT('Ctrl Pts',(-0.193540678138372,-0.000649552417819318,
-0.00523737591822536));
#36579=CARTESIAN_POINT('Ctrl Pts',(-0.193441105496944,-0.000646194280369797,
-0.00486953098091726));
#36580=CARTESIAN_POINT('Ctrl Pts',(-0.193548680125377,-0.00046236752507203,
-0.00518741811674645));
#36581=CARTESIAN_POINT('Ctrl Pts',(-0.19221784368241,-0.000532942846040005,
-0.00544735829321972));
#36582=CARTESIAN_POINT('Ctrl Pts',(-0.192317692121799,-0.000539647098916115,
-0.00504480941502384));
#36583=CARTESIAN_POINT('Ctrl Pts',(-0.192242056430693,-0.000348629122757424,
-0.00539460937276613));
#36584=CARTESIAN_POINT('Ctrl Pts',(-0.190280755377544,0.000121068599940136,
-0.00647511727459894));
#36585=CARTESIAN_POINT('Ctrl Pts',(-0.190539954106928,-4.11033634603214E-5,
-0.00602341757418173));
#36586=CARTESIAN_POINT('Ctrl Pts',(-0.190329131797122,0.000290675906173524,
-0.00641082489689668));
#36587=CARTESIAN_POINT('Ctrl Pts',(-0.188108313415062,0.00183522217201885,
-0.00802874354108597));
#36588=CARTESIAN_POINT('Ctrl Pts',(-0.188185831714158,0.00174861716519636,
-0.00778938974969843));
#36589=CARTESIAN_POINT('Ctrl Pts',(-0.18818459172986,0.00196541394824739,
-0.00794671383597527));
#36590=CARTESIAN_POINT('Ctrl Pts',(-0.186442115636933,0.00425799506259359,
-0.00934492203853191));
#36591=CARTESIAN_POINT('Ctrl Pts',(-0.186505177095779,0.00413522900627745,
-0.00917361754652802));
#36592=CARTESIAN_POINT('Ctrl Pts',(-0.186539821858752,0.00433279168103422,
-0.0092481696460331));
#36593=CARTESIAN_POINT('Ctrl Pts',(-0.185949933848258,0.00649864288516591,
-0.00975604832858269));
#36594=CARTESIAN_POINT('Ctrl Pts',(-0.185938996922361,0.00650356966711613,
-0.0096606155981595));
#36595=CARTESIAN_POINT('Ctrl Pts',(-0.186054161082477,0.00652165633138307,
-0.00965452990509759));
#36596=CARTESIAN_POINT('Ctrl Pts',(-0.186008609242487,0.00779556652501847,
-0.00970683855217618));
#36597=CARTESIAN_POINT('Ctrl Pts',(-0.186012519244314,0.00779930724970625,
-0.00959773856785611));
#36598=CARTESIAN_POINT('Ctrl Pts',(-0.186112045272954,0.00778881516418459,
-0.00960591497712815));
#36599=CARTESIAN_POINT('Ctrl Pts',(-0.192436962091582,-0.000483455930974332,
-0.0055068000272665));
#36600=CARTESIAN_POINT('Ctrl Pts',(-0.192417454388871,-0.000479179295420767,
-0.0055051608623328));
#36601=CARTESIAN_POINT('Ctrl Pts',(-0.192398518083474,-0.000474037136212224,
-0.00550349916183664));
#36602=CARTESIAN_POINT('Ctrl Pts',(-0.192358508328238,-0.000461146975878049,
-0.00550076542168802));
#36603=CARTESIAN_POINT('Ctrl Pts',(-0.192338355794539,-0.000453479114128204,
-0.00549985112232206));
#36604=CARTESIAN_POINT('Ctrl Pts',(-0.192317960073385,-0.000445032779133932,
-0.00549999396547274));
#36605=CARTESIAN_POINT('Ctrl Pts',(-0.186146182193085,0.00666198610159568,
-0.00957677543676099));
#36606=CARTESIAN_POINT('Ctrl Pts',(-0.186108276179088,0.00665976117994766,
-0.00957572084247029));
#36607=CARTESIAN_POINT('Ctrl Pts',(-0.186076614916844,0.00665569960762129,
-0.00959771890028863));
#36608=CARTESIAN_POINT('Ctrl Pts',(-0.186061509823992,0.00665290370623444,
-0.00961964518377239));
#36609=CARTESIAN_POINT('Ctrl Pts',(-0.186052741584085,0.00665128073480653,
-0.0096323730044966));
#36610=CARTESIAN_POINT('Ctrl Pts',(-0.186048069026781,0.00664991367016798,
-0.00964523184213603));
#36611=CARTESIAN_POINT('Ctrl Pts',(-0.186045770369396,0.00664869276501877,
-0.00965738685531515));
#36612=CARTESIAN_POINT('Ctrl Pts',(-0.186005598851858,0.00774016753564896,
0.00970831679928731));
#36613=CARTESIAN_POINT('Ctrl Pts',(-0.186009670836186,0.00774304435209903,
0.00960230395719931));
#36614=CARTESIAN_POINT('Ctrl Pts',(-0.186108014816518,0.00773474456881634,
0.00960842057355287));
#36615=CARTESIAN_POINT('Ctrl Pts',(-0.185960333964487,0.00648227707345362,
0.00974617139101431));
#36616=CARTESIAN_POINT('Ctrl Pts',(-0.185952179587332,0.00648769121866751,
0.00965136579735061));
#36617=CARTESIAN_POINT('Ctrl Pts',(-0.186063352151639,0.00650542775407373,
0.00964582108962002));
#36618=CARTESIAN_POINT('Ctrl Pts',(-0.186428987223196,0.00432575778421166,
0.00935548962635469));
#36619=CARTESIAN_POINT('Ctrl Pts',(-0.186483364142072,0.00421970259174358,
0.00919520509208301));
#36620=CARTESIAN_POINT('Ctrl Pts',(-0.186525917729122,0.00439824791225163,
0.00925957076353963));
#36621=CARTESIAN_POINT('Ctrl Pts',(-0.188010036483664,0.00195171154641976,
0.00810342874470907));
#36622=CARTESIAN_POINT('Ctrl Pts',(-0.188076570799909,0.00187804731004616,
0.00788256538710582));
#36623=CARTESIAN_POINT('Ctrl Pts',(-0.188086956158076,0.00207818061049679,
0.00802123465030675));
#36624=CARTESIAN_POINT('Ctrl Pts',(-0.190096769641379,0.000230160943820068,
0.00659753516612828));
#36625=CARTESIAN_POINT('Ctrl Pts',(-0.190313514403938,8.77705727554797E-5,
0.00619100739750346));
#36626=CARTESIAN_POINT('Ctrl Pts',(-0.190147199090351,0.000396274459653245,
0.0065322762088843));
#36627=CARTESIAN_POINT('Ctrl Pts',(-0.191946116765636,-0.000455424949601966,
0.00557143365312373));
#36628=CARTESIAN_POINT('Ctrl Pts',(-0.192036696545771,-0.000459166706784753,
0.00520128186042438));
#36629=CARTESIAN_POINT('Ctrl Pts',(-0.191973611942258,-0.000273697961367191,
0.00551749368314696));
#36630=CARTESIAN_POINT('Ctrl Pts',(-0.193225816082199,-0.000619663171657372,
0.00528509249354492));
#36631=CARTESIAN_POINT('Ctrl Pts',(-0.193123350533271,-0.000605932760873667,
0.00495167335479587));
#36632=CARTESIAN_POINT('Ctrl Pts',(-0.193237683484677,-0.000433914425303821,
0.00523470332505228));
#36633=CARTESIAN_POINT('Origin',(-0.192200819635387,-0.000325480563679127,
0.00560000000000713));
#36634=CARTESIAN_POINT('Ctrl Pts',(-0.186045766963236,0.00664869409545193,
0.00965738640065765));
#36635=CARTESIAN_POINT('Ctrl Pts',(-0.186050130369219,0.00665101100562805,
0.00963431766854684));
#36636=CARTESIAN_POINT('Ctrl Pts',(-0.186063617073953,0.00665414856520909,
0.00960600839114813));
#36637=CARTESIAN_POINT('Ctrl Pts',(-0.186096378519772,0.00665778543826778,
0.00958849515329468));
#36638=CARTESIAN_POINT('Ctrl Pts',(-0.186110518764896,0.00665935515765138,
0.00958093622327859));
#36639=CARTESIAN_POINT('Ctrl Pts',(-0.186128098007252,0.00666092475184653,
0.00957627595969465));
#36640=CARTESIAN_POINT('Ctrl Pts',(-0.186146182039353,0.00666198624828256,
0.00957677958184586));
#36641=CARTESIAN_POINT('Origin',(-0.187920131339758,0.00750009680678902,
-0.000575225526917647));
#36642=CARTESIAN_POINT('Ctrl Pts',(-0.186045768135075,0.00835131759320733,
-0.00965738542725037));
#36643=CARTESIAN_POINT('Ctrl Pts',(-0.186050128411678,0.00834900218136687,
-0.00963433280458853));
#36644=CARTESIAN_POINT('Ctrl Pts',(-0.186063611063362,0.00834585919375938,
-0.00960601547883551));
#36645=CARTESIAN_POINT('Ctrl Pts',(-0.186096369868285,0.0083422188034536,
-0.00958849943088495));
#36646=CARTESIAN_POINT('Ctrl Pts',(-0.186110513510244,0.00834064706183503,
-0.00958093686224691));
#36647=CARTESIAN_POINT('Ctrl Pts',(-0.186128096876543,0.00833907596658786,
-0.0095762756193603));
#36648=CARTESIAN_POINT('Ctrl Pts',(-0.186146182113142,0.00833801422983676,
-0.00957677929432219));
#36649=CARTESIAN_POINT('Origin',(-0.187954144158173,0.0074999097326559,
0.000581964911843834));
#36650=CARTESIAN_POINT('Ctrl Pts',(-0.186146182120156,0.00833801356110422,
0.00957677710043646));
#36651=CARTESIAN_POINT('Ctrl Pts',(-0.186108254991117,0.00834023913104114,
0.00957572208550327));
#36652=CARTESIAN_POINT('Ctrl Pts',(-0.186076596831025,0.00834429292618449,
0.00959772857351143));
#36653=CARTESIAN_POINT('Ctrl Pts',(-0.186061488244737,0.00834708538103843,
0.00961967482382124));
#36654=CARTESIAN_POINT('Ctrl Pts',(-0.186052741256565,0.00834870204914431,
0.00963238041971281));
#36655=CARTESIAN_POINT('Ctrl Pts',(-0.186048067263802,0.00835006607147121,
0.00964522644092186));
#36656=CARTESIAN_POINT('Ctrl Pts',(-0.186045767212607,0.00835128750327599,
0.00965738803265854));
#36657=CARTESIAN_POINT('Ctrl Pts',(-0.186005598759832,0.00725983232716103,
-0.00970831661057972));
#36658=CARTESIAN_POINT('Ctrl Pts',(-0.186009670651558,0.00725695543053303,
-0.00960230389666019));
#36659=CARTESIAN_POINT('Ctrl Pts',(-0.186108014721025,0.00726525532639936,
-0.00960842038224571));
#36660=CARTESIAN_POINT('Ctrl Pts',(-0.185960334112893,0.00851772391887955,
-0.00974617155991487));
#36661=CARTESIAN_POINT('Ctrl Pts',(-0.185952179909706,0.00851230994790259,
-0.00965136574061983));
#36662=CARTESIAN_POINT('Ctrl Pts',(-0.186063352297074,0.00849457313387128,
-0.00964582125981882));
#36663=CARTESIAN_POINT('Ctrl Pts',(-0.186428987230586,0.0106742426078354,
-0.00935548690241927));
#36664=CARTESIAN_POINT('Ctrl Pts',(-0.186483363531177,0.0107802970046063,
-0.00919520299654669));
#36665=CARTESIAN_POINT('Ctrl Pts',(-0.186525917701738,0.0106017524957044,
-0.00925956807298176));
#36666=CARTESIAN_POINT('Ctrl Pts',(-0.188010038139295,0.0130482906965545,
-0.00810343096067351));
#36667=CARTESIAN_POINT('Ctrl Pts',(-0.188076573310405,0.0131219557179719,
-0.00788256757658765));
#36668=CARTESIAN_POINT('Ctrl Pts',(-0.188086957836586,0.0129218218041267,
-0.00802123671042419));
#36669=CARTESIAN_POINT('Ctrl Pts',(-0.190096773684561,0.014769841299388,
-0.00659753906857564));
#36670=CARTESIAN_POINT('Ctrl Pts',(-0.190313521732662,0.0149122337257658,
-0.00619100814431022));
#36671=CARTESIAN_POINT('Ctrl Pts',(-0.190147203120692,0.0146037275463174,
-0.00653228029147483));
#36672=CARTESIAN_POINT('Ctrl Pts',(-0.191946119174527,0.0154554254581438,
-0.00557143325871853));
#36673=CARTESIAN_POINT('Ctrl Pts',(-0.192036697189508,0.0154591661112836,
-0.0052012805696902));
#36674=CARTESIAN_POINT('Ctrl Pts',(-0.191973614322155,0.0152736983544835,
-0.00551749349096378));
#36675=CARTESIAN_POINT('Ctrl Pts',(-0.193225819175554,0.0156196636689472,
-0.00528509177693916));
#36676=CARTESIAN_POINT('Ctrl Pts',(-0.193123353574421,0.0156059338233821,
-0.0049516714716164));
#36677=CARTESIAN_POINT('Ctrl Pts',(-0.193237686540076,0.0154339148303609,
-0.00523470274052404));
#36678=CARTESIAN_POINT('Origin',(-0.192200822443804,0.0153254812698099,
-0.00560000000000634));
#36679=CARTESIAN_POINT('Ctrl Pts',(-0.193214260006029,0.0156168327619888,
0.00529060396926718));
#36680=CARTESIAN_POINT('Ctrl Pts',(-0.193105326746743,0.0156061976053113,
0.00495284829763268));
#36681=CARTESIAN_POINT('Ctrl Pts',(-0.19322590280958,0.0154311830256504,
0.00523902729326042));
#36682=CARTESIAN_POINT('Ctrl Pts',(-0.191955055227124,0.0154575099667713,
0.00556923862400056));
#36683=CARTESIAN_POINT('Ctrl Pts',(-0.192046773552436,0.0154646012482818,
0.00519213961909146));
#36684=CARTESIAN_POINT('Ctrl Pts',(-0.191982782338575,0.0152758375961863,
0.00551388949624999));
#36685=CARTESIAN_POINT('Ctrl Pts',(-0.190092180578751,0.014769053477849,
0.00660075597892395));
#36686=CARTESIAN_POINT('Ctrl Pts',(-0.190314395130687,0.0149176874591946,
0.00618689814909584));
#36687=CARTESIAN_POINT('Ctrl Pts',(-0.190143807260092,0.0146038314661997,
0.00653331286575727));
#36688=CARTESIAN_POINT('Ctrl Pts',(-0.18800611600784,0.0130431899705215,
0.00810777841374931));
#36689=CARTESIAN_POINT('Ctrl Pts',(-0.188072355662852,0.013119110276285,
0.00788470947760386));
#36690=CARTESIAN_POINT('Ctrl Pts',(-0.188083496099574,0.0129174748375354,
0.00802401143707513));
#36691=CARTESIAN_POINT('Ctrl Pts',(-0.186423687793365,0.0106657581153738,
0.00936054389127776));
#36692=CARTESIAN_POINT('Ctrl Pts',(-0.186478607626537,0.0107749341497348,
0.00919840721838609));
#36693=CARTESIAN_POINT('Ctrl Pts',(-0.186521060649371,0.0105944580941384,
0.00926327090558671));
#36694=CARTESIAN_POINT('Ctrl Pts',(-0.185956374325204,0.00849572718688238,
0.00975032638663647));
#36695=CARTESIAN_POINT('Ctrl Pts',(-0.185946971953686,0.00849053224154058,
0.00965520189867485));
#36696=CARTESIAN_POINT('Ctrl Pts',(-0.186059252699007,0.00847305358346526,
0.00964917339214119));
#36697=CARTESIAN_POINT('Ctrl Pts',(-0.186007036580647,0.00723972881157616,
0.00970794245356266));
#36698=CARTESIAN_POINT('Ctrl Pts',(-0.186010557211458,0.00723652449630214,
0.00960090529757225));
#36699=CARTESIAN_POINT('Ctrl Pts',(-0.186109360775984,0.00724557446066228,
0.0096071910993323));
#36700=CARTESIAN_POINT('Origin',(-0.192200819635407,0.0153254805636842,
0.0056));
#36701=CARTESIAN_POINT('Origin',(-0.195909629570911,0.0153409047393749,
-0.0056053999692199));
#36702=CARTESIAN_POINT('Origin',(-0.192200816462806,0.0153265960442655,
-0.00560463083553559));
#36703=CARTESIAN_POINT('Origin',(-0.214999964645852,0.0154126910904719,
-0.00559999998627319));
#36704=CARTESIAN_POINT('Origin',(-0.195910759730015,0.0153409081694028,
0.00560539872657712));
#36705=CARTESIAN_POINT('Origin',(-0.192200813655147,0.0153265953091492,
0.00560462944582787));
#36706=CARTESIAN_POINT('Origin',(-0.214999964648748,0.0154126899294396,
0.00559999998627548));
#36707=CARTESIAN_POINT('Ctrl Pts',(-0.21490892586111,0.0154128208581019,
-0.0054992439839607));
#36708=CARTESIAN_POINT('Ctrl Pts',(-0.21490857773275,0.0153525928800433,
-0.00549921373553946));
#36709=CARTESIAN_POINT('Ctrl Pts',(-0.214907560745888,0.0153244216769054,
-0.00555248035802741));
#36710=CARTESIAN_POINT('Ctrl Pts',(-0.215674951408508,0.0154080524844426,
-0.00551196326634576));
#36711=CARTESIAN_POINT('Ctrl Pts',(-0.215679476448769,0.0153475795412595,
-0.00551248680902352));
#36712=CARTESIAN_POINT('Ctrl Pts',(-0.215687518203886,0.0153195973000356,
-0.00556554638259137));
#36713=CARTESIAN_POINT('Ctrl Pts',(-0.217146694343493,0.0155818524774486,
-0.00522168280336377));
#36714=CARTESIAN_POINT('Ctrl Pts',(-0.217202913591221,0.0155259749241154,
-0.00520093965385637));
#36715=CARTESIAN_POINT('Ctrl Pts',(-0.217185890291163,0.0154912018795859,
-0.00527389396523135));
#36716=CARTESIAN_POINT('Ctrl Pts',(-0.218674660178022,0.0160010546194908,
-0.00420084024173932));
#36717=CARTESIAN_POINT('Ctrl Pts',(-0.218712852213832,0.0159310643238046,
-0.00416353684961489));
#36718=CARTESIAN_POINT('Ctrl Pts',(-0.218741210132284,0.0159054833219791,
-0.00424664790585557));
#36719=CARTESIAN_POINT('Ctrl Pts',(-0.219590982727002,0.0162655190811837,
-0.00309225143892686));
#36720=CARTESIAN_POINT('Ctrl Pts',(-0.219605835201339,0.0161775572907052,
-0.00306843062806678));
#36721=CARTESIAN_POINT('Ctrl Pts',(-0.219673746959147,0.0161668379039925,
-0.00313100785533165));
#36722=CARTESIAN_POINT('Ctrl Pts',(-0.220279879435486,0.0164007913673191,
-0.00181632823374506));
#36723=CARTESIAN_POINT('Ctrl Pts',(-0.22028722076064,0.0163028450056265,
-0.00179819050090137));
#36724=CARTESIAN_POINT('Ctrl Pts',(-0.220374608289813,0.0163005364595407,
-0.00184630444517829));
#36725=CARTESIAN_POINT('Ctrl Pts',(-0.220646769339641,0.0164711495711873,
-2.23629763584961E-6));
#36726=CARTESIAN_POINT('Ctrl Pts',(-0.220641282865907,0.016372220872245,
-2.22983725660083E-6));
#36727=CARTESIAN_POINT('Ctrl Pts',(-0.220747708289112,0.0163713394014852,
-2.26793534779618E-6));
#36728=CARTESIAN_POINT('Ctrl Pts',(-0.220279811864962,0.0164007768505767,
0.00181691874798004));
#36729=CARTESIAN_POINT('Ctrl Pts',(-0.220287131833914,0.0163028250756232,
0.00179879831642603));
#36730=CARTESIAN_POINT('Ctrl Pts',(-0.220374539505672,0.0163005220232469,
0.00184690427045525));
#36731=CARTESIAN_POINT('Ctrl Pts',(-0.219591001034938,0.0162655270612487,
0.00309233026324212));
#36732=CARTESIAN_POINT('Ctrl Pts',(-0.219605889878344,0.016177574754681,
0.00306847819752524));
#36733=CARTESIAN_POINT('Ctrl Pts',(-0.219673765670875,0.0161668457892537,
0.00313108640475189));
#36734=CARTESIAN_POINT('Ctrl Pts',(-0.218672731422678,0.016000540491302,
0.0042025789662199));
#36735=CARTESIAN_POINT('Ctrl Pts',(-0.218710928868343,0.0159305729552991,
0.0041652594003139));
#36736=CARTESIAN_POINT('Ctrl Pts',(-0.21873924701127,0.0159049752045155,
0.00424839842626237));
#36737=CARTESIAN_POINT('Ctrl Pts',(-0.217149046760076,0.0155822902582286,
0.00522050271701136));
#36738=CARTESIAN_POINT('Ctrl Pts',(-0.217205175745837,0.0155263687734777,
0.00519984674122877));
#36739=CARTESIAN_POINT('Ctrl Pts',(-0.21718828501593,0.0154916345616469,
0.00527270616715176));
#36740=CARTESIAN_POINT('Ctrl Pts',(-0.21567398590997,0.0154080304197497,
0.00551201150898643));
#36741=CARTESIAN_POINT('Ctrl Pts',(-0.215678515075149,0.0153475607801394,
0.00551252965151365));
#36742=CARTESIAN_POINT('Ctrl Pts',(-0.215686535169183,0.0153195758716015,
0.00556559413069578));
#36743=CARTESIAN_POINT('Ctrl Pts',(-0.214909041723364,0.0154128211845327,
0.00549924098553293));
#36744=CARTESIAN_POINT('Ctrl Pts',(-0.214908693448483,0.0153525933808177,
0.00549921106697866));
#36745=CARTESIAN_POINT('Ctrl Pts',(-0.214907678712506,0.0153244222242064,
0.00555247689767116));
#36746=CARTESIAN_POINT('Ctrl Pts',(-0.2309214360969,0.0162188491192864,
-0.00255390765191895));
#36747=CARTESIAN_POINT('Ctrl Pts',(-0.230917643433025,0.016122876817595,
-0.00254933585070519));
#36748=CARTESIAN_POINT('Ctrl Pts',(-0.23084354609566,0.0161191167494639,
-0.00261050295657583));
#36749=CARTESIAN_POINT('Ctrl Pts',(-0.231731271674744,0.0161403427476591,
-0.00353010997290807));
#36750=CARTESIAN_POINT('Ctrl Pts',(-0.231695499917477,0.0160542517468595,
-0.00348698952548079));
#36751=CARTESIAN_POINT('Ctrl Pts',(-0.231653762816047,0.0160414018930904,
-0.00357577197956242));
#36752=CARTESIAN_POINT('Ctrl Pts',(-0.233318350359044,0.0156828169900615,
-0.00544322658274142));
#36753=CARTESIAN_POINT('Ctrl Pts',(-0.233239475942029,0.015640840163108,
-0.00534814877797674));
#36754=CARTESIAN_POINT('Ctrl Pts',(-0.233241585595557,0.0155889048507678,
-0.00546766123177619));
#36755=CARTESIAN_POINT('Ctrl Pts',(-0.235522804973632,0.0140286093773024,
-0.00810054835292838));
#36756=CARTESIAN_POINT('Ctrl Pts',(-0.235456558010287,0.0140244277754155,
-0.00802069209427084));
#36757=CARTESIAN_POINT('Ctrl Pts',(-0.235447062611451,0.0139534444838987,
-0.00809510346252179));
#36758=CARTESIAN_POINT('Ctrl Pts',(-0.237276829383983,0.0112829697892784,
-0.0102149068070439));
#36759=CARTESIAN_POINT('Ctrl Pts',(-0.237233935149465,0.0113000460915102,
-0.0101632006923216));
#36760=CARTESIAN_POINT('Ctrl Pts',(-0.237201895619677,0.0112392878602733,
-0.010185602465943));
#36761=CARTESIAN_POINT('Ctrl Pts',(-0.238023912985867,0.00751556963457164,
-0.0111154658415992));
#36762=CARTESIAN_POINT('Ctrl Pts',(-0.237996530980257,0.00751544365575127,
-0.0110824586755033));
#36763=CARTESIAN_POINT('Ctrl Pts',(-0.237949322608371,0.00751538718331989,
-0.0110759389184273));
#36764=CARTESIAN_POINT('Ctrl Pts',(-0.237280015258684,0.00371938391596711,
-0.0102187471647188));
#36765=CARTESIAN_POINT('Ctrl Pts',(-0.237237148916806,0.00370230591124238,
-0.0101670746726941));
#36766=CARTESIAN_POINT('Ctrl Pts',(-0.237205082965768,0.00376303943723787,
-0.0101893990031388));
#36767=CARTESIAN_POINT('Ctrl Pts',(-0.235529704617421,0.000981618018545073,
-0.00810886540945947));
#36768=CARTESIAN_POINT('Ctrl Pts',(-0.235463830484283,0.000985956441676499,
-0.0080294585725564));
#36769=CARTESIAN_POINT('Ctrl Pts',(-0.235453965445146,0.00105666489234918,
-0.00810332645705537));
#36770=CARTESIAN_POINT('Ctrl Pts',(-0.233330300192999,-0.000678550038604275,
-0.00545763130384987));
#36771=CARTESIAN_POINT('Ctrl Pts',(-0.233250985436449,-0.000636996429499461,
-0.00536202269932594));
#36772=CARTESIAN_POINT('Ctrl Pts',(-0.233253541020546,-0.000584686101854415,
-0.00548190240738322));
#36773=CARTESIAN_POINT('Ctrl Pts',(-0.231731717669817,-0.00114029951282499,
-0.00353064758997168));
#36774=CARTESIAN_POINT('Ctrl Pts',(-0.231695913807421,-0.0010542152324075,
-0.00348748844212362));
#36775=CARTESIAN_POINT('Ctrl Pts',(-0.231654209020796,-0.00104135909373062,
-0.00357630357546777));
#36776=CARTESIAN_POINT('Ctrl Pts',(-0.2309214360969,-0.00121884911929219,
-0.00255390765191891));
#36777=CARTESIAN_POINT('Ctrl Pts',(-0.230917643433025,-0.00112287681760122,
-0.00254933585070488));
#36778=CARTESIAN_POINT('Ctrl Pts',(-0.23084354609566,-0.00111911674946971,
-0.00261050295657523));
#36779=CARTESIAN_POINT('Ctrl Pts',(-0.2309214360969,0.0162188491192864,
-0.00255390765191895));
#36780=CARTESIAN_POINT('Ctrl Pts',(-0.230919775033979,0.0161747085289458,
-0.00255190535228738));
#36781=CARTESIAN_POINT('Ctrl Pts',(-0.230893153703761,0.0161330891388246,
-0.00257080002687729));
#36782=CARTESIAN_POINT('Ctrl Pts',(-0.230859886434142,0.0161221790363513,
-0.00259732739947869));
#36783=CARTESIAN_POINT('Ctrl Pts',(-0.23085451814243,0.0161204184887214,
-0.00260160808364952));
#36784=CARTESIAN_POINT('Ctrl Pts',(-0.230849026328935,0.0161193903409544,
-0.00260604101323845));
#36785=CARTESIAN_POINT('Ctrl Pts',(-0.230843551760371,0.0161191162061102,
-0.00261050970535095));
#36786=CARTESIAN_POINT('Ctrl Pts',(-0.230843551742607,-0.00111911620782001,
-0.0026105096841861));
#36787=CARTESIAN_POINT('Ctrl Pts',(-0.23087747757725,-0.00112081501570214,
-0.002582817285748));
#36788=CARTESIAN_POINT('Ctrl Pts',(-0.23091000473876,-0.00115445692580184,
-0.0025584489568953));
#36789=CARTESIAN_POINT('Ctrl Pts',(-0.230918875913022,-0.00119762015153162,
-0.00255440400298611));
#36790=CARTESIAN_POINT('Ctrl Pts',(-0.230920307572675,-0.00120458597668313,
-0.00255375121484989));
#36791=CARTESIAN_POINT('Ctrl Pts',(-0.230921168038885,-0.00121172579473758,
-0.00255358452601128));
#36792=CARTESIAN_POINT('Ctrl Pts',(-0.2309214360969,-0.00121884911929219,
-0.00255390765191891));
#36793=CARTESIAN_POINT('Origin',(-0.23397514962969,-0.000958411587553637,
-2.1312647177279E-10));
#36794=CARTESIAN_POINT('Ctrl Pts',(-0.2309214360969,-0.00121884929951176,
0.00255390765191896));
#36795=CARTESIAN_POINT('Ctrl Pts',(-0.230919775047316,-0.00117470864868834,
0.00255190536836447));
#36796=CARTESIAN_POINT('Ctrl Pts',(-0.230893153683133,-0.00113308926455962,
0.0025708001043909));
#36797=CARTESIAN_POINT('Ctrl Pts',(-0.230859886422908,-0.00112217919297818,
0.00259732750272073));
#36798=CARTESIAN_POINT('Ctrl Pts',(-0.230854518134609,-0.00112041865095552,
0.00260160818953043));
#36799=CARTESIAN_POINT('Ctrl Pts',(-0.230849026325164,-0.00111939050845762,
0.00260604112123923));
#36800=CARTESIAN_POINT('Ctrl Pts',(-0.230843551761021,-0.00111911637834476,
0.00261050981525893));
#36801=CARTESIAN_POINT('Origin',(-0.233975149629148,0.015958411588167,2.19838690515469E-10));
#36802=CARTESIAN_POINT('Ctrl Pts',(-0.230843551743257,0.0161191163800488,
0.00261050979409577));
#36803=CARTESIAN_POINT('Ctrl Pts',(-0.230877477562569,0.0161208151592145,
0.00258281737399711));
#36804=CARTESIAN_POINT('Ctrl Pts',(-0.230910004742525,0.016154457039061,
0.00255844899691895));
#36805=CARTESIAN_POINT('Ctrl Pts',(-0.230918875916907,0.0161976203127023,
0.00255440401393904));
#36806=CARTESIAN_POINT('Ctrl Pts',(-0.230920307576072,0.0162045861431113,
0.0025537512213432));
#36807=CARTESIAN_POINT('Ctrl Pts',(-0.230921168041133,0.0162117259677385,
0.00255358452872089));
#36808=CARTESIAN_POINT('Ctrl Pts',(-0.2309214360969,0.016218849299512,0.00255390765191894));
#36809=CARTESIAN_POINT('Ctrl Pts',(-0.2309214360969,-0.00121884929951176,
0.00255390765191896));
#36810=CARTESIAN_POINT('Ctrl Pts',(-0.230917643482494,-0.00112287692579763,
0.00254933591033698));
#36811=CARTESIAN_POINT('Ctrl Pts',(-0.230843546096085,-0.00111911692171259,
0.00261050306621451));
#36812=CARTESIAN_POINT('Ctrl Pts',(-0.231731271358665,-0.0011403440413955,
0.00353010959189706));
#36813=CARTESIAN_POINT('Ctrl Pts',(-0.231695500440064,-0.00105425268533019,
0.00348699015503689));
#36814=CARTESIAN_POINT('Ctrl Pts',(-0.231653762502425,-0.00104140314540818,
0.00357577200213956));
#36815=CARTESIAN_POINT('Ctrl Pts',(-0.233318351429915,-0.000682830411131618,
0.00544322787360406));
#36816=CARTESIAN_POINT('Ctrl Pts',(-0.233239475950391,-0.000640855225105034,
0.00534814878822644));
#36817=CARTESIAN_POINT('Ctrl Pts',(-0.233241586693064,-0.000588918662889074,
0.00546766133448137));
#36818=CARTESIAN_POINT('Ctrl Pts',(-0.235522785051244,0.000971430442923571,
0.00810052433783006));
#36819=CARTESIAN_POINT('Ctrl Pts',(-0.235456540369885,0.000975613862285589,
0.00802067082991012));
#36820=CARTESIAN_POINT('Ctrl Pts',(-0.235447042598565,0.00104659521317374,
0.00809507963380781));
#36821=CARTESIAN_POINT('Ctrl Pts',(-0.237276842725964,0.00371701980185319,
0.0102149228899044));
#36822=CARTESIAN_POINT('Ctrl Pts',(-0.237233947381609,0.00369994316081699,
0.0101632154373597));
#36823=CARTESIAN_POINT('Ctrl Pts',(-0.237201908997141,0.00376070251875742,
0.0101856188837833));
#36824=CARTESIAN_POINT('Ctrl Pts',(-0.238023907994334,0.00748443566710092,
0.0111154598246424));
#36825=CARTESIAN_POINT('Ctrl Pts',(-0.237996526448544,0.00748456159372698,
0.0110824532128226));
#36826=CARTESIAN_POINT('Ctrl Pts',(-0.237949317601923,0.00748461804540081,
0.0110759327314131));
#36827=CARTESIAN_POINT('Ctrl Pts',(-0.237280027202557,0.0112806277971099,
0.0102187615622546));
#36828=CARTESIAN_POINT('Ctrl Pts',(-0.237237159718854,0.0112977061424594,
0.0101670876938473));
#36829=CARTESIAN_POINT('Ctrl Pts',(-0.23720509494468,0.0112369714924193,
0.0101894137458077));
#36830=CARTESIAN_POINT('Ctrl Pts',(-0.235529684253431,0.0140183426910286,
0.00810884086203866));
#36831=CARTESIAN_POINT('Ctrl Pts',(-0.235463812480867,0.0140140023765735,
0.00802943687061338));
#36832=CARTESIAN_POINT('Ctrl Pts',(-0.235453944990362,0.0139432959143817,
0.00810330212192403));
#36833=CARTESIAN_POINT('Ctrl Pts',(-0.233330301704251,0.0156785630234985,
0.00545763312556219));
#36834=CARTESIAN_POINT('Ctrl Pts',(-0.233250985892042,0.0156370110386122,
0.0053620232486558));
#36835=CARTESIAN_POINT('Ctrl Pts',(-0.233253542558448,0.0155846994939661,
0.00548190301630521));
#36836=CARTESIAN_POINT('Ctrl Pts',(-0.231731717357689,0.0161403008067932,
0.00353064721372319));
#36837=CARTESIAN_POINT('Ctrl Pts',(-0.231695914333758,0.0160542161711817,
0.00348748907626018));
#36838=CARTESIAN_POINT('Ctrl Pts',(-0.231654208711274,0.016041360346251,
0.00357630360283988));
#36839=CARTESIAN_POINT('Ctrl Pts',(-0.2309214360969,0.016218849299512,0.00255390765191894));
#36840=CARTESIAN_POINT('Ctrl Pts',(-0.230917643482494,0.0161228769257979,
0.00254933591033697));
#36841=CARTESIAN_POINT('Ctrl Pts',(-0.230843546096085,0.0161191169217128,
0.00261050306621451));
#36842=CARTESIAN_POINT('Origin',(-0.192200819635407,0.0153254805636842,
0.0056));
#36843=CARTESIAN_POINT('Origin',(-0.192200819635407,0.0153254805636842,
0.00559999999999991));
#36844=CARTESIAN_POINT('Origin',(-0.194168411395185,0.0075,0.0056));
#36845=CARTESIAN_POINT('Origin',(-0.192768810476938,0.0154467402534237,
0.0056));
#36846=CARTESIAN_POINT('Origin',(-0.203884397086387,0.0154879659720582,
0.00559998733259232));
#36847=CARTESIAN_POINT('Origin',(-0.192768785940054,0.0154467401648028,
0.00559999999397933));
#36848=CARTESIAN_POINT('Origin',(-0.215,0.0155256283130765,0.0056));
#36849=CARTESIAN_POINT('Ctrl Pts',(-0.213229729843132,0.0157022153177789,
0.00520680787665651));
#36850=CARTESIAN_POINT('Ctrl Pts',(-0.213345218715168,0.0158225893493084,
0.00528453405189864));
#36851=CARTESIAN_POINT('Ctrl Pts',(-0.213196001721802,0.0157923672594748,
0.00534544678633676));
#36852=CARTESIAN_POINT('Ctrl Pts',(-0.214547134769444,0.0154162104902854,
0.00565430653154903));
#36853=CARTESIAN_POINT('Ctrl Pts',(-0.214582356671007,0.0156149459953766,
0.00559914657177998));
#36854=CARTESIAN_POINT('Ctrl Pts',(-0.214538193317879,0.0155026474148113,
0.00580706225979799));
#36855=CARTESIAN_POINT('Ctrl Pts',(-0.216690019804745,0.0155682893667712,
0.00552681293735305));
#36856=CARTESIAN_POINT('Ctrl Pts',(-0.216451145680206,0.0156840968084039,
0.00562885092889451));
#36857=CARTESIAN_POINT('Ctrl Pts',(-0.216722901066365,0.0156574855861506,
0.00567355244670012));
#36858=CARTESIAN_POINT('Ctrl Pts',(-0.218675003043817,0.0161056764401404,
0.00420057423278555));
#36859=CARTESIAN_POINT('Ctrl Pts',(-0.218617098144112,0.0162182154556049,
0.00425851519670619));
#36860=CARTESIAN_POINT('Ctrl Pts',(-0.218743439038924,0.0162011697080541,
0.00430773273508922));
#36861=CARTESIAN_POINT('Ctrl Pts',(-0.219591213832591,0.016366893294022,
0.00309190376565664));
#36862=CARTESIAN_POINT('Ctrl Pts',(-0.219573634362248,0.016475367130996,
0.00312025455357957));
#36863=CARTESIAN_POINT('Ctrl Pts',(-0.21967659313197,0.0164655000154654,
0.00316589708552006));
#36864=CARTESIAN_POINT('Ctrl Pts',(-0.22028001583951,0.0165005526889646,
0.00181590820288125));
#36865=CARTESIAN_POINT('Ctrl Pts',(-0.220272524676665,0.0166017602705409,
0.00183458973337379));
#36866=CARTESIAN_POINT('Ctrl Pts',(-0.220378568714464,0.0166007864600911,
0.00185228354006585));
#36867=CARTESIAN_POINT('Ctrl Pts',(-0.22064664085763,0.0165713244858559,
2.35907764938227E-6));
#36868=CARTESIAN_POINT('Ctrl Pts',(-0.220652325872645,0.0166753647140379,
2.36179922074191E-6));
#36869=CARTESIAN_POINT('Ctrl Pts',(-0.220752242592502,0.0166711024300162,
2.41267673127293E-6));
#36870=CARTESIAN_POINT('Ctrl Pts',(-0.220280060746434,0.0165005514591195,
-0.00181618365853376));
#36871=CARTESIAN_POINT('Ctrl Pts',(-0.220272599527913,0.0166017669045666,
-0.0018348368457429));
#36872=CARTESIAN_POINT('Ctrl Pts',(-0.220378614204616,0.0166007849096865,
-0.00185256631919835));
#36873=CARTESIAN_POINT('Ctrl Pts',(-0.219591366060322,0.0163669363399105,
-0.00309179373683757));
#36874=CARTESIAN_POINT('Ctrl Pts',(-0.219573740983601,0.016475396719567,
-0.00312018560140071));
#36875=CARTESIAN_POINT('Ctrl Pts',(-0.219676748701557,0.0164655437352039,
-0.00316578368963275));
#36876=CARTESIAN_POINT('Ctrl Pts',(-0.218673191355524,0.0161051953605198,
-0.00420222688246931));
#36877=CARTESIAN_POINT('Ctrl Pts',(-0.218615263580567,0.0162177542044613,
-0.00426021396407952));
#36878=CARTESIAN_POINT('Ctrl Pts',(-0.218741593455134,0.0162006827472677,
-0.00430943468512786));
#36879=CARTESIAN_POINT('Ctrl Pts',(-0.216693610859714,0.0155689870287889,
-0.00552479954599455));
#36880=CARTESIAN_POINT('Ctrl Pts',(-0.216455449539926,0.0156849298060722,
-0.00562628440487122));
#36881=CARTESIAN_POINT('Ctrl Pts',(-0.216726553008683,0.0156581905368916,
-0.00567148258730312));
#36882=CARTESIAN_POINT('Ctrl Pts',(-0.214542851116322,0.0154156975121673,
-0.00565574169440847));
#36883=CARTESIAN_POINT('Ctrl Pts',(-0.214576974400863,0.0156142882723724,
-0.00560107345113347));
#36884=CARTESIAN_POINT('Ctrl Pts',(-0.214533839877423,0.0155021297478814,
-0.00580853651161884));
#36885=CARTESIAN_POINT('Ctrl Pts',(-0.213238161199259,0.0157028755263122,
-0.00520501194558692));
#36886=CARTESIAN_POINT('Ctrl Pts',(-0.213354454181688,0.0158232964870154,
-0.00528243459469491));
#36887=CARTESIAN_POINT('Ctrl Pts',(-0.213204580729378,0.0157930357316283,
-0.00534359720917359));
#36888=CARTESIAN_POINT('Origin',(-0.215,0.0155256291596528,-0.00560000000000002));
#36889=CARTESIAN_POINT('Origin',(-0.203884398706272,0.0154879667406767,
-0.0055999873317088));
#36890=CARTESIAN_POINT('Origin',(-0.192768785327122,0.0154485451014724,
-0.00559995859404333));
#36891=CARTESIAN_POINT('Ctrl Pts',(-0.186128733753088,0.00811916857619173,
0.00989255350779034));
#36892=CARTESIAN_POINT('Ctrl Pts',(-0.186018778618736,0.00811313503271661,
0.00990168049066551));
#36893=CARTESIAN_POINT('Ctrl Pts',(-0.186023944961261,0.00811996577256876,
0.00979312213356084));
#36894=CARTESIAN_POINT('Ctrl Pts',(-0.186018485294857,0.00670554737044195,
0.00998601759439623));
#36895=CARTESIAN_POINT('Ctrl Pts',(-0.185922064757894,0.00670303587685495,
0.00998410879659885));
#36896=CARTESIAN_POINT('Ctrl Pts',(-0.185913335621815,0.00670391887197537,
0.00988488069051847));
#36897=CARTESIAN_POINT('Ctrl Pts',(-0.186483100624033,0.00435893839440719,
0.0095907193630887));
#36898=CARTESIAN_POINT('Ctrl Pts',(-0.186324782316601,0.00446640991982842,
0.00964072473835667));
#36899=CARTESIAN_POINT('Ctrl Pts',(-0.186378987360796,0.0043601940661907,
0.00949725178366898));
#36900=CARTESIAN_POINT('Ctrl Pts',(-0.188201072765365,0.00181549250946339,
0.00821893131634974));
#36901=CARTESIAN_POINT('Ctrl Pts',(-0.188078336118818,0.0018504078480918,
0.0082484121438556));
#36902=CARTESIAN_POINT('Ctrl Pts',(-0.188118956208556,0.00180751667010245,
0.00813902082106135));
#36903=CARTESIAN_POINT('Ctrl Pts',(-0.190470772042906,4.0286060397758E-5,
0.0065914793017016));
#36904=CARTESIAN_POINT('Ctrl Pts',(-0.190354564891624,6.51615565258696E-5,
0.00662079265626122));
#36905=CARTESIAN_POINT('Ctrl Pts',(-0.190415663760779,2.89000666232802E-5,
0.0065295234995035));
#36906=CARTESIAN_POINT('Ctrl Pts',(-0.192527761414073,-0.000596244059895659,
0.00555832684088505));
#36907=CARTESIAN_POINT('Ctrl Pts',(-0.19249929215549,-0.000615208227213908,
0.00553484330744896));
#36908=CARTESIAN_POINT('Ctrl Pts',(-0.192505145382581,-0.000612248109762194,
0.00550334510791334));
#36909=CARTESIAN_POINT('Ctrl Pts',(-0.193914490094568,-0.000653721049803873,
0.00545568506849627));
#36910=CARTESIAN_POINT('Ctrl Pts',(-0.193918273424759,-0.000668045313244978,
0.00543022477246777));
#36911=CARTESIAN_POINT('Ctrl Pts',(-0.19391192840682,-0.000669112281798238,
0.00540217205656248));
#36912=CARTESIAN_POINT('Origin',(-0.192768810476942,-0.000446740253424534,
0.00560000000000438));
#36913=CARTESIAN_POINT('Ctrl Pts',(-0.186116972251352,0.00692238523863633,
0.0098966261734716));
#36914=CARTESIAN_POINT('Ctrl Pts',(-0.186078299389446,0.00691967369755638,
0.0098954315730185));
#36915=CARTESIAN_POINT('Ctrl Pts',(-0.186041366807831,0.00691866352655612,
0.00986822062204796));
#36916=CARTESIAN_POINT('Ctrl Pts',(-0.186027502170506,0.00691962821437211,
0.0098347241084879));
#36917=CARTESIAN_POINT('Ctrl Pts',(-0.186022400056034,0.00691998321447427,
0.00982239756560122));
#36918=CARTESIAN_POINT('Ctrl Pts',(-0.186019959759874,0.00692055847709167,
0.00980946425272828));
#36919=CARTESIAN_POINT('Ctrl Pts',(-0.186019887800529,0.00692126510446277,
0.00979701417759536));
#36920=CARTESIAN_POINT('Origin',(-0.185989784446262,0.00750308162677683,
0.00987843431341192));
#36921=CARTESIAN_POINT('Origin',(-0.185989783463039,0.00749692179129775,
0.00987845623397708));
#36922=CARTESIAN_POINT('Ctrl Pts',(-0.186019887786807,0.00807873471322789,
0.00979701374348257));
#36923=CARTESIAN_POINT('Ctrl Pts',(-0.186020093677862,0.0080807581272644,
0.00983266188385409));
#36924=CARTESIAN_POINT('Ctrl Pts',(-0.186043173449962,0.00808148714810779,
0.00987274783946665));
#36925=CARTESIAN_POINT('Ctrl Pts',(-0.186081182198031,0.00807971774323728,
0.00988879730954875));
#36926=CARTESIAN_POINT('Ctrl Pts',(-0.186092525490223,0.0080791896838438,
0.00989358709710865));
#36927=CARTESIAN_POINT('Ctrl Pts',(-0.186104812966911,0.008078467319158,
0.00989625064514937));
#36928=CARTESIAN_POINT('Ctrl Pts',(-0.186116972833414,0.0080776147210469,
0.0098966261914198));
#36929=CARTESIAN_POINT('Ctrl Pts',(-0.186023972731768,0.00688051014267458,
0.00979310237707671));
#36930=CARTESIAN_POINT('Ctrl Pts',(-0.186018810213327,0.00688730839985145,
0.00990129751290525));
#36931=CARTESIAN_POINT('Ctrl Pts',(-0.186128366061288,0.00688133137396351,
0.009892610868904));
#36932=CARTESIAN_POINT('Ctrl Pts',(-0.185913319128721,0.00829598470916531,
0.00988477449605492));
#36933=CARTESIAN_POINT('Ctrl Pts',(-0.185921918992968,0.00829687156644818,
0.00998368580418176));
#36934=CARTESIAN_POINT('Ctrl Pts',(-0.186018138486974,0.00829436520850232,
0.00998594242117922));
#36935=CARTESIAN_POINT('Ctrl Pts',(-0.186379085964777,0.0106388494478239,
0.00949735159004442));
#36936=CARTESIAN_POINT('Ctrl Pts',(-0.186325170520145,0.0105330510663237,
0.00964031833428041));
#36937=CARTESIAN_POINT('Ctrl Pts',(-0.186482574570187,0.0106396543485447,
0.00959107234597323));
#36938=CARTESIAN_POINT('Ctrl Pts',(-0.188116939791643,0.0131908723913694,
0.00814009748260041));
#36939=CARTESIAN_POINT('Ctrl Pts',(-0.188076305605751,0.0131480938494406,
0.00824921860919713));
#36940=CARTESIAN_POINT('Ctrl Pts',(-0.188198545915983,0.0131827291314941,
0.00822019894550857));
#36941=CARTESIAN_POINT('Ctrl Pts',(-0.190415937111015,0.0149698341055998,
0.00653082897886206));
#36942=CARTESIAN_POINT('Ctrl Pts',(-0.190355170838482,0.0149336698703752,
0.006621860304423));
#36943=CARTESIAN_POINT('Ctrl Pts',(-0.190470436359477,0.0149583114745633,
0.00659299102128988));
#36944=CARTESIAN_POINT('Ctrl Pts',(-0.192492055253889,0.0156105230518145,
0.00550622573432866));
#36945=CARTESIAN_POINT('Ctrl Pts',(-0.192486126269825,0.0156134661142462,
0.00553773279556526));
#36946=CARTESIAN_POINT('Ctrl Pts',(-0.192514707567575,0.0155946170172933,
0.00556113935696853));
#36947=CARTESIAN_POINT('Ctrl Pts',(-0.193930356418938,0.0156719780414651,
0.00539761904618806));
#36948=CARTESIAN_POINT('Ctrl Pts',(-0.193936349353485,0.0156708752141232,
0.00542558152286841));
#36949=CARTESIAN_POINT('Ctrl Pts',(-0.193932726634534,0.0156566594700174,
0.0054509632651032));
#36950=CARTESIAN_POINT('Origin',(-0.19276881047694,0.015446740253424,0.00560000000000575));
#36951=CARTESIAN_POINT('Origin',(-0.192768810476937,0.0154467402534276,
0.0056));
#36952=CARTESIAN_POINT('Origin',(-0.185989784252021,0.00749691842201206,
-0.00987843432316569));
#36953=CARTESIAN_POINT('Ctrl Pts',(-0.186116972293536,0.00807761530404597,
-0.00989662596793202));
#36954=CARTESIAN_POINT('Ctrl Pts',(-0.186078299413494,0.00808032684892871,
-0.00989543136817047));
#36955=CARTESIAN_POINT('Ctrl Pts',(-0.186041366832626,0.00808133701405912,
-0.00986822040267438));
#36956=CARTESIAN_POINT('Ctrl Pts',(-0.186027502200621,0.00808037231720565,
-0.00983472388492247));
#36957=CARTESIAN_POINT('Ctrl Pts',(-0.186022400090923,0.00808001731397372,
-0.00982239734729829));
#36958=CARTESIAN_POINT('Ctrl Pts',(-0.186019959796752,0.00807944204809531,
-0.00980946404050643));
#36959=CARTESIAN_POINT('Ctrl Pts',(-0.186019887837588,0.00807873541742951,
-0.00979701396990226));
#36960=CARTESIAN_POINT('Ctrl Pts',(-0.193944739328741,0.0156748013854394,
-0.00539335846462329));
#36961=CARTESIAN_POINT('Ctrl Pts',(-0.193950405063627,0.0156736055039752,
-0.00542214039838788));
#36962=CARTESIAN_POINT('Ctrl Pts',(-0.193946792457245,0.0156587687228256,
-0.0054479092071319));
#36963=CARTESIAN_POINT('Ctrl Pts',(-0.192479951547028,0.0156079751812,-0.00551008560225899));
#36964=CARTESIAN_POINT('Ctrl Pts',(-0.192474038576552,0.0156110162627067,
-0.00554243345066391));
#36965=CARTESIAN_POINT('Ctrl Pts',(-0.192504190847607,0.0155911177095731,
-0.00556621720267825));
#36966=CARTESIAN_POINT('Ctrl Pts',(-0.190424348361861,0.0149720682294561,
-0.00652716548449426));
#36967=CARTESIAN_POINT('Ctrl Pts',(-0.190362307407983,0.0149351914758667,
-0.00662047975539135));
#36968=CARTESIAN_POINT('Ctrl Pts',(-0.190484255774687,0.0149617060832159,
-0.0065878831497931));
#36969=CARTESIAN_POINT('Ctrl Pts',(-0.188119418738792,0.0131951211101891,
-0.00813770573613879));
#36970=CARTESIAN_POINT('Ctrl Pts',(-0.188077128181627,0.0131507446359388,
-0.00825043507259777));
#36971=CARTESIAN_POINT('Ctrl Pts',(-0.188206302928862,0.0131885075000646,
-0.00821645594207363));
#36972=CARTESIAN_POINT('Ctrl Pts',(-0.18637868791602,0.0106375219868189,
-0.00949784839851767));
#36973=CARTESIAN_POINT('Ctrl Pts',(-0.186322706105325,0.0105275875956226,
-0.00964615897678578));
#36974=CARTESIAN_POINT('Ctrl Pts',(-0.186488066256925,0.0106423773751142,
-0.00958965009614401));
#36975=CARTESIAN_POINT('Ctrl Pts',(-0.185913669513949,0.00830000359003704,
-0.00988441259603338));
#36976=CARTESIAN_POINT('Ctrl Pts',(-0.185922643233334,0.00830115989286702,
-0.00998702246588958));
#36977=CARTESIAN_POINT('Ctrl Pts',(-0.186021834644838,0.00829826476234554,
-0.00998560862165242));
#36978=CARTESIAN_POINT('Ctrl Pts',(-0.186023567857763,0.00687519942614235,
-0.0097934618530046));
#36979=CARTESIAN_POINT('Ctrl Pts',(-0.186018168818418,0.00688206724060213,
-0.00990578909223112));
#36980=CARTESIAN_POINT('Ctrl Pts',(-0.186131856313941,0.00687583464295538,
-0.00989260188754259));
#36981=CARTESIAN_POINT('Origin',(-0.192768813717277,0.0154467408241202,
-0.0056));
#36982=CARTESIAN_POINT('Origin',(-0.192768813717277,0.0154467408241202,
-0.0056));
#36983=CARTESIAN_POINT('Origin',(-0.192768813717277,0.0154467408241202,
-0.0056));
#36984=CARTESIAN_POINT('Origin',(-0.194168411395185,0.0075,-0.0056));
#36985=CARTESIAN_POINT('Origin',(-0.192200822443821,0.0153254812698141,
-0.0056));
#36986=CARTESIAN_POINT('Origin',(-0.192200822443821,0.0153254812698141,
-0.0056));
#36987=CARTESIAN_POINT('Origin',(-0.18598978326554,0.00750307815796359,
-0.00987845625295267));
#36988=CARTESIAN_POINT('Ctrl Pts',(-0.186019887823865,0.00692126476492155,
-0.00979701353578103));
#36989=CARTESIAN_POINT('Ctrl Pts',(-0.186020093714527,0.00691924134015948,
-0.00983266168510107));
#36990=CARTESIAN_POINT('Ctrl Pts',(-0.186043173490947,0.00691851231002105,
-0.00987274764345759));
#36991=CARTESIAN_POINT('Ctrl Pts',(-0.186081182254119,0.00692028171431255,
-0.00988879711126473));
#36992=CARTESIAN_POINT('Ctrl Pts',(-0.186092525541513,0.00692080977310006,
-0.00989358689421662));
#36993=CARTESIAN_POINT('Ctrl Pts',(-0.186104813013035,0.00692153213765697,
-0.00989625044013151));
#36994=CARTESIAN_POINT('Ctrl Pts',(-0.186116972875644,0.00692238473624832,
-0.00989662598588015));
#36995=CARTESIAN_POINT('Ctrl Pts',(-0.186024639723174,0.00812811219565812,
-0.00979252019536039));
#36996=CARTESIAN_POINT('Ctrl Pts',(-0.186019307378118,0.00812086552414072,
-0.00990231673970523));
#36997=CARTESIAN_POINT('Ctrl Pts',(-0.186130557641939,0.00812738702814064,
-0.00989184348985861));
#36998=CARTESIAN_POINT('Ctrl Pts',(-0.185911665726943,0.00670243418658247,
-0.00988630161052383));
#36999=CARTESIAN_POINT('Ctrl Pts',(-0.185920664362397,0.00670182531369318,
-0.00998651802648809));
#37000=CARTESIAN_POINT('Ctrl Pts',(-0.186017796509969,0.00670406967969763,
-0.00998748004843489));
#37001=CARTESIAN_POINT('Ctrl Pts',(-0.186383092477577,0.00434243298325542,
-0.00949365754992548));
#37002=CARTESIAN_POINT('Ctrl Pts',(-0.186327057599337,0.00445165179097786,
-0.00963954915710208));
#37003=CARTESIAN_POINT('Ctrl Pts',(-0.186488965294518,0.00433989462961623,
-0.00958646459001603));
#37004=CARTESIAN_POINT('Ctrl Pts',(-0.18814229846019,0.00178054587572309,
-0.00812126933382206));
#37005=CARTESIAN_POINT('Ctrl Pts',(-0.188100433060655,0.00182438698528336,
-0.00823203675775219));
#37006=CARTESIAN_POINT('Ctrl Pts',(-0.188225725746846,0.00178808327780345,
-0.00820056143173852));
#37007=CARTESIAN_POINT('Ctrl Pts',(-0.19044452191719,1.6202403067083E-5,
-0.00651141629438544));
#37008=CARTESIAN_POINT('Ctrl Pts',(-0.19038385400963,5.14577023083873E-5,
-0.00660218703061461));
#37009=CARTESIAN_POINT('Ctrl Pts',(-0.190500763004092,2.74049476685753E-5,
-0.00657287877422572));
#37010=CARTESIAN_POINT('Ctrl Pts',(-0.19253117826135,-0.000615266065116062,
-0.00549731033749768));
#37011=CARTESIAN_POINT('Ctrl Pts',(-0.192526147348343,-0.000618092939049415,
-0.00552868410424512));
#37012=CARTESIAN_POINT('Ctrl Pts',(-0.19255375702597,-0.000599009037967802,
-0.00555258554180868));
#37013=CARTESIAN_POINT('Ctrl Pts',(-0.193918783756537,-0.000668624514627959,
-0.00540402469955559));
#37014=CARTESIAN_POINT('Ctrl Pts',(-0.193924564628155,-0.000667662297456414,
-0.00543253495238252));
#37015=CARTESIAN_POINT('Ctrl Pts',(-0.193921264643106,-0.000653011155466118,
-0.00545790459201301));
#37016=CARTESIAN_POINT('Ctrl Pts',(-0.192768459141627,-0.000531128306595919,
-0.00565363457355974));
#37017=CARTESIAN_POINT('Ctrl Pts',(-0.19276562570579,-0.000541650536466089,
-0.00563706845375414));
#37018=CARTESIAN_POINT('Ctrl Pts',(-0.192762819238559,-0.000547210055500382,
-0.00561736740483649));
#37019=CARTESIAN_POINT('Ctrl Pts',(-0.192760018688902,-0.000546732541444601,
-0.00559775525115174));
#37020=CARTESIAN_POINT('Origin',(-0.203590952700175,-0.000486871388071358,
-0.0055999858664995));
#37021=CARTESIAN_POINT('Origin',(-0.215,-0.000525629159653763,-0.0056));
#37022=CARTESIAN_POINT('Ctrl Pts',(-0.213229730364857,-0.000702212951003181,
-0.00520680784009235));
#37023=CARTESIAN_POINT('Ctrl Pts',(-0.21334554019071,-0.000822928423967307,
-0.0052847510567193));
#37024=CARTESIAN_POINT('Ctrl Pts',(-0.213195754239947,-0.000792314496048851,
-0.00534554749344366));
#37025=CARTESIAN_POINT('Ctrl Pts',(-0.214547134435015,-0.000416213562106486,
-0.00565430653835661));
#37026=CARTESIAN_POINT('Ctrl Pts',(-0.214582465858957,-0.00061556757186644,
-0.00559897618104724));
#37027=CARTESIAN_POINT('Ctrl Pts',(-0.214538126572902,-0.000502481732189858,
-0.00580737405250504));
#37028=CARTESIAN_POINT('Ctrl Pts',(-0.216690020107536,-0.000568288146151568,
-0.00552681299596838));
#37029=CARTESIAN_POINT('Ctrl Pts',(-0.216450453443573,-0.000684435862739555,
-0.00562914645532142));
#37030=CARTESIAN_POINT('Ctrl Pts',(-0.216723337291576,-0.00065744162975446,
-0.00567362346679069));
#37031=CARTESIAN_POINT('Ctrl Pts',(-0.218675003475181,-0.00110567341750779,
-0.00420057382676157));
#37032=CARTESIAN_POINT('Ctrl Pts',(-0.218616955185385,-0.00121849151929721,
-0.0042586581440736));
#37033=CARTESIAN_POINT('Ctrl Pts',(-0.218743679225851,-0.00120113404056507,
-0.00430782564282987));
#37034=CARTESIAN_POINT('Ctrl Pts',(-0.21959121396959,-0.00136689275323617,
-0.0030919035315441));
#37035=CARTESIAN_POINT('Ctrl Pts',(-0.219573593820357,-0.0014756160323326,
-0.00312031990591821));
#37036=CARTESIAN_POINT('Ctrl Pts',(-0.219676803998535,-0.00146547899713251,
-0.00316599038852783));
#37037=CARTESIAN_POINT('Ctrl Pts',(-0.220280015856011,-0.00150055300539941,
-0.00181590812685752));
#37038=CARTESIAN_POINT('Ctrl Pts',(-0.220272508157456,-0.0016019827403939,
-0.00183463094445556));
#37039=CARTESIAN_POINT('Ctrl Pts',(-0.220378796107586,-0.00160078446929803,
-0.00185232121959389));
#37040=CARTESIAN_POINT('Ctrl Pts',(-0.220646640852067,-0.00157132448681648,
-2.35895081128692E-6));
#37041=CARTESIAN_POINT('Ctrl Pts',(-0.220652338405761,-0.00167559421886387,
-2.36109324866209E-6));
#37042=CARTESIAN_POINT('Ctrl Pts',(-0.22075245579331,-0.00167109309083381,
-2.41275124305137E-6));
#37043=CARTESIAN_POINT('Ctrl Pts',(-0.220280060746729,-0.00150055113982659,
0.00181618363817644));
#37044=CARTESIAN_POINT('Ctrl Pts',(-0.220272583236875,-0.00160198890362842,
0.00183487750996121));
#37045=CARTESIAN_POINT('Ctrl Pts',(-0.220378841515704,-0.00160078222822346,
0.00185260440179092));
#37046=CARTESIAN_POINT('Ctrl Pts',(-0.219591366035501,-0.00136693691002698,
0.00309179380892092));
#37047=CARTESIAN_POINT('Ctrl Pts',(-0.219573700695601,-0.00147564663065069,
0.0031202505503224));
#37048=CARTESIAN_POINT('Ctrl Pts',(-0.219676959497499,-0.00146552392066298,
0.00316587679000158));
#37049=CARTESIAN_POINT('Ctrl Pts',(-0.218673190971741,-0.00110519840036426,
0.0042022272613154));
#37050=CARTESIAN_POINT('Ctrl Pts',(-0.21861511946106,-0.00121803612509124,
0.0042603583574915));
#37051=CARTESIAN_POINT('Ctrl Pts',(-0.218741832748112,-0.00120065320451856,
0.00430952815393783));
#37052=CARTESIAN_POINT('Ctrl Pts',(-0.216693610695147,-0.000568988272581022,
0.00552479943366079));
#37053=CARTESIAN_POINT('Ctrl Pts',(-0.216454744952011,-0.000685269450178146,
0.00562658481509268));
#37054=CARTESIAN_POINT('Ctrl Pts',(-0.216726987943305,-0.000658148482718064,
0.00567155509388602));
#37055=CARTESIAN_POINT('Ctrl Pts',(-0.214542851347544,-0.000415694418949238,
0.00565574173556768));
#37056=CARTESIAN_POINT('Ctrl Pts',(-0.214577081649168,-0.000614907730571467,
0.00560090086194077));
#37057=CARTESIAN_POINT('Ctrl Pts',(-0.214533775275375,-0.000501957450787837,
0.00580884872688636));
#37058=CARTESIAN_POINT('Ctrl Pts',(-0.21323816078666,-0.000702877922631073,
0.0052050119165415));
#37059=CARTESIAN_POINT('Ctrl Pts',(-0.213354787946414,-0.000823638003085672,
0.00528265601711787));
#37060=CARTESIAN_POINT('Ctrl Pts',(-0.213204331015681,-0.000792987504077056,
0.00534369882673873));
#37061=CARTESIAN_POINT('Origin',(-0.215,-0.000525628313076073,0.0056));
#37062=CARTESIAN_POINT('Origin',(-0.2038843971522,-0.000487965972298664,
0.00559998733259273));
#37063=CARTESIAN_POINT('Origin',(-0.192768785940078,-0.000446740164802543,
0.00559999999397934));
#37064=CARTESIAN_POINT('Origin',(-0.192768810476959,-0.00044674025342738,
0.0056));
#37065=CARTESIAN_POINT('Origin',(-0.192768810476942,-0.000446740253424536,
0.00560000000000438));
#37066=CARTESIAN_POINT('Origin',(-0.194168411395185,0.0075,0.0056));
#37067=CARTESIAN_POINT('Origin',(-0.192200819635406,-0.000325480563683811,
0.0056));
#37068=CARTESIAN_POINT('Origin',(-0.192200819635406,-0.000325480563683833,
0.0056));
#37069=CARTESIAN_POINT('Origin',(-0.23397529105232,0.0160594292892167,-2.10028825614146E-10));
#37070=CARTESIAN_POINT('Origin',(-0.230844479079951,0.0163191139685996,
0.00261776387735059));
#37071=CARTESIAN_POINT('Origin',(-0.230844479057671,0.0163191137983529,
-0.0026177638505009));
#37072=CARTESIAN_POINT('Ctrl Pts',(-0.228930011320165,-0.00121666210944132,
-0.000153558508944395));
#37073=CARTESIAN_POINT('Ctrl Pts',(-0.228925068649108,-0.00130356078038321,
-0.00014061325969051));
#37074=CARTESIAN_POINT('Ctrl Pts',(-0.228852816272702,-0.00131993372474197,
-0.000198511747305299));
#37075=CARTESIAN_POINT('Ctrl Pts',(-0.230431551941403,-0.00149901747374101,
-0.00196359261958752));
#37076=CARTESIAN_POINT('Ctrl Pts',(-0.230546199755791,-0.00163485191727014,
-0.00209314633244308));
#37077=CARTESIAN_POINT('Ctrl Pts',(-0.230356760340796,-0.00160667853259381,
-0.00203317374358696));
#37078=CARTESIAN_POINT('Ctrl Pts',(-0.232741868391858,-0.00122412725612965,
-0.00474856455279266));
#37079=CARTESIAN_POINT('Ctrl Pts',(-0.233002328000619,-0.00122807080927364,
-0.00505085271150412));
#37080=CARTESIAN_POINT('Ctrl Pts',(-0.232669082600517,-0.00132530889872912,
-0.00485258198260278));
#37081=CARTESIAN_POINT('Ctrl Pts',(-0.235571864603083,0.000893540287141985,
-0.00815998429435824));
#37082=CARTESIAN_POINT('Ctrl Pts',(-0.235780526318094,0.000886440100530878,
-0.00839417044424366));
#37083=CARTESIAN_POINT('Ctrl Pts',(-0.23549602082886,0.000816861323350659,
-0.00829967543390585));
#37084=CARTESIAN_POINT('Ctrl Pts',(-0.237350191606613,0.00367117676218051,
-0.0103036684753349));
#37085=CARTESIAN_POINT('Ctrl Pts',(-0.237562885455937,0.00375230645071915,
-0.0105367888728918));
#37086=CARTESIAN_POINT('Ctrl Pts',(-0.237273146969764,0.00362802005513088,
-0.0104664740917656));
#37087=CARTESIAN_POINT('Ctrl Pts',(-0.237978275379249,0.00684374843593728,
-0.011060791815887));
#37088=CARTESIAN_POINT('Ctrl Pts',(-0.23815533351796,0.00681408943718553,
-0.0112478230763381));
#37089=CARTESIAN_POINT('Ctrl Pts',(-0.237900276754974,0.00683577450692037,
-0.011231052981414));
#37090=CARTESIAN_POINT('Ctrl Pts',(-0.237735579461005,0.00941406809132023,
-0.0107682341472069));
#37091=CARTESIAN_POINT('Ctrl Pts',(-0.237905547438819,0.00945031005365003,
-0.0109479806253355));
#37092=CARTESIAN_POINT('Ctrl Pts',(-0.237657647464612,0.00943669370360537,
-0.010935275193432));
#37093=CARTESIAN_POINT('Ctrl Pts',(-0.237055387725117,0.0117812538241882,
-0.00994829713676746));
#37094=CARTESIAN_POINT('Ctrl Pts',(-0.237219994321457,0.0118075629637152,
-0.0101246180217082));
#37095=CARTESIAN_POINT('Ctrl Pts',(-0.236977820224706,0.0118312943583801,
-0.0101063746716028));
#37096=CARTESIAN_POINT('Ctrl Pts',(-0.235580244204118,0.0140975190661438,
-0.00817008549077605));
#37097=CARTESIAN_POINT('Ctrl Pts',(-0.23578623244027,0.0141029322156517,
-0.00840102389984029));
#37098=CARTESIAN_POINT('Ctrl Pts',(-0.235504346470908,0.01417405436759,
-0.00830983268046781));
#37099=CARTESIAN_POINT('Ctrl Pts',(-0.232754563684081,0.0162205064390394,
-0.00476386809962718));
#37100=CARTESIAN_POINT('Ctrl Pts',(-0.233017755071115,0.0162243053630947,
-0.005069430660515));
#37101=CARTESIAN_POINT('Ctrl Pts',(-0.232681829483814,0.016321647383219,
-0.00486812521810131));
#37102=CARTESIAN_POINT('Ctrl Pts',(-0.230420611920092,0.0165030822444603,
-0.00195040496493689));
#37103=CARTESIAN_POINT('Ctrl Pts',(-0.230536669856679,0.0166381031145872,
-0.0020816713149296));
#37104=CARTESIAN_POINT('Ctrl Pts',(-0.230345861479217,0.0166107689301663,
-0.00201988343589639));
#37105=CARTESIAN_POINT('Ctrl Pts',(-0.22894365783775,0.0162108337471327,
-0.000170008710922436));
#37106=CARTESIAN_POINT('Ctrl Pts',(-0.228934589862323,0.0162990618020438,
-0.000152076705750483));
#37107=CARTESIAN_POINT('Ctrl Pts',(-0.228866347045808,0.0163140754347603,
-0.00021501163526663));
#37108=CARTESIAN_POINT('Origin',(-0.230844479079726,-0.00131911379624309,
-0.00261776387708007));
#37109=CARTESIAN_POINT('Ctrl Pts',(-0.228930018643561,0.0162166782265411,
0.000153567348635035));
#37110=CARTESIAN_POINT('Ctrl Pts',(-0.228925034474289,0.0163035747204591,
0.000140571617611529));
#37111=CARTESIAN_POINT('Ctrl Pts',(-0.228852822004403,0.0163199491706983,
0.00019852322100711));
#37112=CARTESIAN_POINT('Ctrl Pts',(-0.230431547159926,0.0164990010424598,
0.00196358686148426));
#37113=CARTESIAN_POINT('Ctrl Pts',(-0.230546210928832,0.0166348359316639,
0.00209315975026496));
#37114=CARTESIAN_POINT('Ctrl Pts',(-0.23035675495291,0.0166066625558943,
0.00203316613867527));
#37115=CARTESIAN_POINT('Ctrl Pts',(-0.232741874999713,0.0162241552295754,
0.00474857253009821));
#37116=CARTESIAN_POINT('Ctrl Pts',(-0.233002336525729,0.0162280967339862,
0.00505086248822097));
#37117=CARTESIAN_POINT('Ctrl Pts',(-0.232669087560718,0.0163253369091607,
0.00485259065406883));
#37118=CARTESIAN_POINT('Ctrl Pts',(-0.235571844631025,0.0141064194522958,
0.00815996023088895));
#37119=CARTESIAN_POINT('Ctrl Pts',(-0.235780503221004,0.0141135232971628,
0.00839414213517375));
#37120=CARTESIAN_POINT('Ctrl Pts',(-0.235495999776369,0.0141830986004907,
0.00829965082076248));
#37121=CARTESIAN_POINT('Ctrl Pts',(-0.23735020499403,0.0113288345386507,
0.0103036846257339));
#37122=CARTESIAN_POINT('Ctrl Pts',(-0.237562903802203,0.0112477073380563,
0.0105368103191969));
#37123=CARTESIAN_POINT('Ctrl Pts',(-0.237273159453406,0.0113719926988885,
0.0104664898863485));
#37124=CARTESIAN_POINT('Ctrl Pts',(-0.237978272727021,0.00815624622582596,
0.0110607886321847));
#37125=CARTESIAN_POINT('Ctrl Pts',(-0.238155332546526,0.0081858990714908,
0.0112478210492935));
#37126=CARTESIAN_POINT('Ctrl Pts',(-0.23790027337051,0.00816421945360661,
0.0112310497653436));
#37127=CARTESIAN_POINT('Ctrl Pts',(-0.237735583958034,0.00558592810337824,
0.0107682395816002));
#37128=CARTESIAN_POINT('Ctrl Pts',(-0.237905555367753,0.00554968907454929,
0.0109479892946036));
#37129=CARTESIAN_POINT('Ctrl Pts',(-0.237657651224066,0.00556330322602589,
0.0109352808534232));
#37130=CARTESIAN_POINT('Ctrl Pts',(-0.237055393487095,0.00321874016769531,
0.00994830409475942));
#37131=CARTESIAN_POINT('Ctrl Pts',(-0.23722000314611,0.0031924317775692,
0.0101246280895804));
#37132=CARTESIAN_POINT('Ctrl Pts',(-0.236977825203511,0.00316869826984275,
0.0101063812287948));
#37133=CARTESIAN_POINT('Ctrl Pts',(-0.235580224122505,0.000902521439204644,
0.00817006129529639));
#37134=CARTESIAN_POINT('Ctrl Pts',(-0.235786207806912,0.000897102342494172,
0.00840099372924289));
#37135=CARTESIAN_POINT('Ctrl Pts',(-0.235504325292979,0.000825986039287472,
0.00830980795273018));
#37136=CARTESIAN_POINT('Ctrl Pts',(-0.232754570759086,-0.00122053420958835,
0.00476387664005792));
#37137=CARTESIAN_POINT('Ctrl Pts',(-0.233017765329059,-0.00122432956214392,
0.00506944252624999));
#37138=CARTESIAN_POINT('Ctrl Pts',(-0.232681834927955,-0.00132167522919554,
0.00486813447178729));
#37139=CARTESIAN_POINT('Ctrl Pts',(-0.230420606752338,-0.00150306601983695,
0.00195039874119751));
#37140=CARTESIAN_POINT('Ctrl Pts',(-0.230536680061682,-0.00163808816037902,
0.00208168356580272));
#37141=CARTESIAN_POINT('Ctrl Pts',(-0.23034585568313,-0.00161075313981024,
0.00201987533518042));
#37142=CARTESIAN_POINT('Ctrl Pts',(-0.228943665649166,-0.00121084957355264,
0.000170018138880857));
#37143=CARTESIAN_POINT('Ctrl Pts',(-0.228934556962248,-0.00129907450314452,
0.000152036599788699));
#37144=CARTESIAN_POINT('Ctrl Pts',(-0.228866353311391,-0.00131409060945743,
0.000215023759721046));
#37145=CARTESIAN_POINT('Origin',(-0.230844479057897,-0.00131911397071442,
0.00261776385077347));
#37146=CARTESIAN_POINT('Origin',(-0.233975291052864,-0.00105942928952791,
2.16727099247223E-10));
#37147=CARTESIAN_POINT('Origin',(-0.226549796019406,0.0104788589677295,
-0.00737701084641453));
#37148=CARTESIAN_POINT('Ctrl Pts',(-0.225965068063626,0.0102955231026494,
-0.0103688478531334));
#37149=CARTESIAN_POINT('Ctrl Pts',(-0.225965835469434,0.0102847030452682,
-0.0103375543236173));
#37150=CARTESIAN_POINT('Ctrl Pts',(-0.22596662506635,0.0102740358497316,
-0.0103060888750999));
#37151=CARTESIAN_POINT('Ctrl Pts',(-0.225967436625428,0.0102635326203732,
-0.0102744751969217));
#37152=CARTESIAN_POINT('Ctrl Pts',(-0.224903047769934,0.0163974953490442,
0.00232527569536224));
#37153=CARTESIAN_POINT('Ctrl Pts',(-0.228003678801843,0.0163652528946496,
0.00231821622721085));
#37154=CARTESIAN_POINT('Ctrl Pts',(-0.23110431006382,0.0163330357098684,
0.00231114482972889));
#37155=CARTESIAN_POINT('Ctrl Pts',(-0.234204941533998,0.0163008422866106,
0.00230405918705812));
#37156=CARTESIAN_POINT('Ctrl Pts',(-0.224902923051373,0.016421905903896,
0.001999690061282));
#37157=CARTESIAN_POINT('Ctrl Pts',(-0.228003554472057,0.0163857948128496,
0.00199154431614981));
#37158=CARTESIAN_POINT('Ctrl Pts',(-0.231104186130884,0.0163497065102629,
0.00198339075959686));
#37159=CARTESIAN_POINT('Ctrl Pts',(-0.23420481801057,0.0163136399270852,
0.00197522735965944));
#37160=CARTESIAN_POINT('Ctrl Pts',(-0.224902686634519,0.0164496060066283,
0.00134999605462854));
#37161=CARTESIAN_POINT('Ctrl Pts',(-0.228003316903349,0.0164061218898441,
0.00134119319572166));
#37162=CARTESIAN_POINT('Ctrl Pts',(-0.231103947348719,0.0163626446434222,
0.00133240817680761));
#37163=CARTESIAN_POINT('Ctrl Pts',(-0.234204577993315,0.0163191760221561,
0.00132364096404516));
#37164=CARTESIAN_POINT('Ctrl Pts',(-0.22490247733934,0.0164891827557564,
8.48946422705292E-5));
#37165=CARTESIAN_POINT('Ctrl Pts',(-0.2280031047451,0.0164387037966636,
8.36968421714054E-5));
#37166=CARTESIAN_POINT('Ctrl Pts',(-0.231103732057188,0.01638822192355,
8.25020821930779E-5));
#37167=CARTESIAN_POINT('Ctrl Pts',(-0.234204359262361,0.016337735996471,
8.13110569434896E-5));
#37168=CARTESIAN_POINT('Ctrl Pts',(-0.224902601832635,0.0164577305274795,
-0.00116946331798178));
#37169=CARTESIAN_POINT('Ctrl Pts',(-0.22800323228218,0.0164115731563456,
-0.00115947279336496));
#37170=CARTESIAN_POINT('Ctrl Pts',(-0.231103862912676,0.016365419418937,
-0.00114950763219157));
#37171=CARTESIAN_POINT('Ctrl Pts',(-0.234204493754791,0.0163192718567599,
-0.00113956819841304));
#37172=CARTESIAN_POINT('Ctrl Pts',(-0.2249031047193,0.016401050271707,-0.00247428944274167));
#37173=CARTESIAN_POINT('Ctrl Pts',(-0.228003735976318,0.016370691448232,
-0.00246735407024901));
#37174=CARTESIAN_POINT('Ctrl Pts',(-0.231104367476673,0.0163403620163895,
-0.00246039974613875));
#37175=CARTESIAN_POINT('Ctrl Pts',(-0.234204999188339,0.0163100597051565,
-0.00245342363871553));
#37176=CARTESIAN_POINT('Ctrl Pts',(-0.224903620482978,0.0162331344936927,
-0.00377581649114323));
#37177=CARTESIAN_POINT('Ctrl Pts',(-0.228004247053984,0.0162183248288798,
-0.00377611183675602));
#37178=CARTESIAN_POINT('Ctrl Pts',(-0.231104873706723,0.0162035348039987,
-0.00377640360674382));
#37179=CARTESIAN_POINT('Ctrl Pts',(-0.23420550044494,0.0161887639228305,
-0.00377669038870648));
#37180=CARTESIAN_POINT('Ctrl Pts',(-0.224904244439412,0.0157454055087051,
-0.00535508843351867));
#37181=CARTESIAN_POINT('Ctrl Pts',(-0.228004869356698,0.015745877431058,
-0.00536654194974573));
#37182=CARTESIAN_POINT('Ctrl Pts',(-0.231105494288016,0.0157463686608469,
-0.00537798949180189));
#37183=CARTESIAN_POINT('Ctrl Pts',(-0.234206119236561,0.0157468784277487,
-0.00538942975580705));
#37184=CARTESIAN_POINT('Ctrl Pts',(-0.224904927056323,0.014756116525245,
-0.0070809462510311));
#37185=CARTESIAN_POINT('Ctrl Pts',(-0.228005551277712,0.0147682738612367,
-0.00710847555851588));
#37186=CARTESIAN_POINT('Ctrl Pts',(-0.231106175457583,0.0147804448844733,
-0.00713600323790223));
#37187=CARTESIAN_POINT('Ctrl Pts',(-0.234206799604821,0.014792629252247,
-0.00716352865861212));
#37188=CARTESIAN_POINT('Ctrl Pts',(-0.224905705935764,0.0129587456084716,
-0.00904270204015799));
#37189=CARTESIAN_POINT('Ctrl Pts',(-0.228006331471737,0.0129775263446935,
-0.00909152831654588));
#37190=CARTESIAN_POINT('Ctrl Pts',(-0.231106956961612,0.0129963155259409,
-0.00914035417356039));
#37191=CARTESIAN_POINT('Ctrl Pts',(-0.234207582410669,0.0130151128918419,
-0.00918917939755658));
#37192=CARTESIAN_POINT('Ctrl Pts',(-0.224906344901157,0.00996717482975785,
-0.0106558172504251));
#37193=CARTESIAN_POINT('Ctrl Pts',(-0.228006973196984,0.00997888641244874,
-0.0107253416344494));
#37194=CARTESIAN_POINT('Ctrl Pts',(-0.23110760149003,0.00999060093234777,
-0.0107948661290257));
#37195=CARTESIAN_POINT('Ctrl Pts',(-0.234208229780548,0.0100023182636535,
-0.010864390745125));
#37196=CARTESIAN_POINT('Ctrl Pts',(-0.224906421473904,0.00588448586822914,
-0.0108495989887083));
#37197=CARTESIAN_POINT('Ctrl Pts',(-0.228007050197119,0.00587660352368733,
-0.0109217704181749));
#37198=CARTESIAN_POINT('Ctrl Pts',(-0.231107678925808,0.00586871925150363,
-0.0109939418074081));
#37199=CARTESIAN_POINT('Ctrl Pts',(-0.23420830765933,0.00586083314294305,
-0.0110661131658069));
#37200=CARTESIAN_POINT('Ctrl Pts',(-0.224905896797368,0.00275206275993148,
-0.00952499259309634));
#37201=CARTESIAN_POINT('Ctrl Pts',(-0.22800652301585,0.00273399542249794,
-0.00957977151548));
#37202=CARTESIAN_POINT('Ctrl Pts',(-0.231107149196805,0.00271592133715538,
-0.00963455045765119));
#37203=CARTESIAN_POINT('Ctrl Pts',(-0.234207775344483,0.00269784071003669,
-0.00968932931015458));
#37204=CARTESIAN_POINT('Ctrl Pts',(-0.224905188461513,0.000775386387695849,
-0.00774097724716007));
#37205=CARTESIAN_POINT('Ctrl Pts',(-0.228005812987761,0.000760338332521188,
-0.0077754138708565));
#37206=CARTESIAN_POINT('Ctrl Pts',(-0.231106437467874,0.000745278047377309,
-0.00780984908461508));
#37207=CARTESIAN_POINT('Ctrl Pts',(-0.234207061909447,0.000730205873823641,
-0.00784428237662763));
#37208=CARTESIAN_POINT('Ctrl Pts',(-0.224904545212544,-0.00037433699893992,
-0.00611286595312136));
#37209=CARTESIAN_POINT('Ctrl Pts',(-0.228005169500613,-0.000380655003703386,
-0.00613103039787742));
#37210=CARTESIAN_POINT('Ctrl Pts',(-0.231105793767721,-0.000386989095479687,
-0.00614919200572512));
#37211=CARTESIAN_POINT('Ctrl Pts',(-0.234206418022201,-0.000393338834079428,
-0.00616734988680402));
#37212=CARTESIAN_POINT('Ctrl Pts',(-0.224903937950997,-0.00100476933014151,
-0.00458381173225385));
#37213=CARTESIAN_POINT('Ctrl Pts',(-0.228004563842973,-0.000997949740617374,
-0.00458943898701532));
#37214=CARTESIAN_POINT('Ctrl Pts',(-0.231105189790958,-0.000991151361328939,
-0.00459505880592969));
#37215=CARTESIAN_POINT('Ctrl Pts',(-0.234205815794275,-0.000984373265027772,
-0.00460066961067425));
#37216=CARTESIAN_POINT('Ctrl Pts',(-0.224903434943426,-0.00130314167877163,
-0.00330350941820122));
#37217=CARTESIAN_POINT('Ctrl Pts',(-0.228004062879574,-0.00128286930948369,
-0.00330122419140405));
#37218=CARTESIAN_POINT('Ctrl Pts',(-0.231104690943801,-0.00126261869681616,
-0.0032989320974583));
#37219=CARTESIAN_POINT('Ctrl Pts',(-0.234205319131308,-0.00124238896138437,
-0.00329663139924215));
#37220=CARTESIAN_POINT('Ctrl Pts',(-0.224903041260456,-0.00140805611840559,
-0.00232453718253355));
#37221=CARTESIAN_POINT('Ctrl Pts',(-0.228003673257076,-0.0013756315595115,
-0.00231672000225054));
#37222=CARTESIAN_POINT('Ctrl Pts',(-0.231104305522642,-0.00134323774830377,
-0.00230888218475535));
#37223=CARTESIAN_POINT('Ctrl Pts',(-0.234204938019884,-0.00131087220379368,
-0.00230102069899992));
#37224=CARTESIAN_POINT('Ctrl Pts',(-0.224902686634356,-0.00144960594189391,
-0.00134999602285112));
#37225=CARTESIAN_POINT('Ctrl Pts',(-0.228003316903184,-0.00140612182039602,
-0.00134119316178982));
#37226=CARTESIAN_POINT('Ctrl Pts',(-0.23110394734855,-0.00136264456921374,
-0.00133240814074275));
#37227=CARTESIAN_POINT('Ctrl Pts',(-0.234204577993143,-0.00131917594314456,
-0.00132364092587474));
#37228=CARTESIAN_POINT('Ctrl Pts',(-0.22490247733939,-0.0014891827680679,
-8.48946648711828E-5));
#37229=CARTESIAN_POINT('Ctrl Pts',(-0.228003104745152,-0.00143870380997731,
-8.36968663193096E-5));
#37230=CARTESIAN_POINT('Ctrl Pts',(-0.231103732057244,-0.00138822193789455,
-8.25021078797203E-5));
#37231=CARTESIAN_POINT('Ctrl Pts',(-0.23420435926242,-0.00133773601187166,
-8.1311084157012E-5));
#37232=CARTESIAN_POINT('Ctrl Pts',(-0.22490260183294,-0.0014577307002292,
0.00116946334942344));
#37233=CARTESIAN_POINT('Ctrl Pts',(-0.228003232282475,-0.00141157334093523,
0.00115947282708936));
#37234=CARTESIAN_POINT('Ctrl Pts',(-0.231103862912961,-0.00136541961535455,
0.00114950766822477));
#37235=CARTESIAN_POINT('Ctrl Pts',(-0.234204493755065,-0.001319272064998,
0.00113956823678177));
#37236=CARTESIAN_POINT('Ctrl Pts',(-0.224903104718753,-0.00140104996632292,
0.00247428939345485));
#37237=CARTESIAN_POINT('Ctrl Pts',(-0.228003735975788,-0.00137069112187628,
0.00246735401736931));
#37238=CARTESIAN_POINT('Ctrl Pts',(-0.231104367476161,-0.0013403616690761,
0.00246039968961847));
#37239=CARTESIAN_POINT('Ctrl Pts',(-0.234204999187845,-0.00131005933689176,
0.00245342357850486));
#37240=CARTESIAN_POINT('Ctrl Pts',(-0.224903620487317,-0.00123313642614889,
0.00377581720335721));
#37241=CARTESIAN_POINT('Ctrl Pts',(-0.228004247058324,-0.00121832689931329,
0.00377611259775251));
#37242=CARTESIAN_POINT('Ctrl Pts',(-0.231104873711069,-0.00120353701330459,
0.00377640441621043));
#37243=CARTESIAN_POINT('Ctrl Pts',(-0.234205500449294,-0.00118876627184354,
0.00377669124621538));
#37244=CARTESIAN_POINT('Ctrl Pts',(-0.224904244452509,-0.000745411287960432,
0.00535508951527424));
#37245=CARTESIAN_POINT('Ctrl Pts',(-0.228004869369835,-0.000745883603517816,
0.00536654310520161));
#37246=CARTESIAN_POINT('Ctrl Pts',(-0.231105494301186,-0.000746375225293753,
0.00537799072107391));
#37247=CARTESIAN_POINT('Ctrl Pts',(-0.234206119249757,-0.000746885383007411,
0.00538943105918803));
#37248=CARTESIAN_POINT('Ctrl Pts',(-0.224904927022406,0.000243903830950042,
0.00708094602779947));
#37249=CARTESIAN_POINT('Ctrl Pts',(-0.22800555124417,0.000231747907332828,
0.00710847531073915));
#37250=CARTESIAN_POINT('Ctrl Pts',(-0.231106175424446,0.00021957829815924,
0.00713600296412369));
#37251=CARTESIAN_POINT('Ctrl Pts',(-0.234206799572117,0.000207395346249357,
0.0071635283576419));
#37252=CARTESIAN_POINT('Ctrl Pts',(-0.224905705882564,0.00204129536417242,
0.00904270545084878));
#37253=CARTESIAN_POINT('Ctrl Pts',(-0.228006331417495,0.00202251745037019,
0.00909153197079319));
#37254=CARTESIAN_POINT('Ctrl Pts',(-0.231106956906316,0.00200373108991613,
0.00914035807264341));
#37255=CARTESIAN_POINT('Ctrl Pts',(-0.234207582354303,0.00198493654309014,
0.00918918354252649));
#37256=CARTESIAN_POINT('Ctrl Pts',(-0.224906344934492,0.00503279669879239,
0.0106558220281949));
#37257=CARTESIAN_POINT('Ctrl Pts',(-0.228006973230644,0.00502108315461209,
0.0107253467403358));
#37258=CARTESIAN_POINT('Ctrl Pts',(-0.231107601524016,0.00500936667421796,
0.0107948715627757));
#37259=CARTESIAN_POINT('Ctrl Pts',(-0.234208229814862,0.00499764738343722,
0.0108643965065502));
#37260=CARTESIAN_POINT('Ctrl Pts',(-0.22490642148267,0.00911553811978304,
0.0108495997280891));
#37261=CARTESIAN_POINT('Ctrl Pts',(-0.22800705020616,0.00912342211753167,
0.0109217712057851));
#37262=CARTESIAN_POINT('Ctrl Pts',(-0.231107678935135,0.0091313080421625,
0.0109939426427322));
#37263=CARTESIAN_POINT('Ctrl Pts',(-0.234208307668951,0.00913919580236395,
0.0110661140483708));
#37264=CARTESIAN_POINT('Ctrl Pts',(-0.224905896781363,0.0122479140000228,
0.00952499840433065));
#37265=CARTESIAN_POINT('Ctrl Pts',(-0.228006522998932,0.0122659797356893,
0.00957977773742142));
#37266=CARTESIAN_POINT('Ctrl Pts',(-0.231107149178945,0.012284052220171,
0.00963455709198015));
#37267=CARTESIAN_POINT('Ctrl Pts',(-0.234207775325653,0.0123021312474762,
0.00968933635838273));
#37268=CARTESIAN_POINT('Ctrl Pts',(-0.224905188406661,0.0142245802852993,
0.00774097735435126));
#37269=CARTESIAN_POINT('Ctrl Pts',(-0.228005812932864,0.014239626038719,
0.0077754139801973));
#37270=CARTESIAN_POINT('Ctrl Pts',(-0.231106437412959,0.0142546840218181,
0.00780984919513146));
#37271=CARTESIAN_POINT('Ctrl Pts',(-0.234207061854539,0.014269753892948,
0.00784428248742507));
#37272=CARTESIAN_POINT('Ctrl Pts',(-0.224904545213284,0.0153743354777482,
0.00611286639462737));
#37273=CARTESIAN_POINT('Ctrl Pts',(-0.228005169501712,0.0153806533667306,
0.00613103086359291));
#37274=CARTESIAN_POINT('Ctrl Pts',(-0.231105793769188,0.0153869873403304,
0.0061491924949429));
#37275=CARTESIAN_POINT('Ctrl Pts',(-0.234206418024041,0.0153933369583363,
0.00616735039916125));
#37276=CARTESIAN_POINT('Ctrl Pts',(-0.224903937959543,0.0160047733300576,
0.00458381273421664));
#37277=CARTESIAN_POINT('Ctrl Pts',(-0.228004563851456,0.015997954017428,
0.00458944005855562));
#37278=CARTESIAN_POINT('Ctrl Pts',(-0.231105189799372,0.0159911559151915,
0.00459505994710943));
#37279=CARTESIAN_POINT('Ctrl Pts',(-0.234205815802617,0.0159843780961064,
0.00460067082154373));
#37280=CARTESIAN_POINT('Ctrl Pts',(-0.224903434945887,0.0163031426775171,
0.00330350985910996));
#37281=CARTESIAN_POINT('Ctrl Pts',(-0.228004062882068,0.0162828703806443,
0.0033012246620879));
#37282=CARTESIAN_POINT('Ctrl Pts',(-0.231104690946332,0.0162626198410551,
0.00329893259759974));
#37283=CARTESIAN_POINT('Ctrl Pts',(-0.23420531913388,0.0162423901793082,
0.00329663192843727));
#37284=CARTESIAN_POINT('Ctrl Pts',(-0.224903172488496,0.0163730847941923,
0.00265086132944247));
#37285=CARTESIAN_POINT('Ctrl Pts',(-0.22800380313163,0.0163447109764496,
0.00264488813827189));
#37286=CARTESIAN_POINT('Ctrl Pts',(-0.231104433996755,0.0163163649094739,
0.00263889889986091));
#37287=CARTESIAN_POINT('Ctrl Pts',(-0.234205065057425,0.0162880446461359,
0.00263289101445681));
#37288=CARTESIAN_POINT('Ctrl Pts',(-0.224903047769934,0.0163974953490442,
0.00232527569536224));
#37289=CARTESIAN_POINT('Ctrl Pts',(-0.228003678801843,0.0163652528946496,
0.00231821622721085));
#37290=CARTESIAN_POINT('Ctrl Pts',(-0.23110431006382,0.0163330357098684,
0.00231114482972889));
#37291=CARTESIAN_POINT('Ctrl Pts',(-0.234204941533998,0.0163008422866106,
0.00230405918705812));
#37292=CARTESIAN_POINT('',(-0.227006637251675,0.0126927900142701,-0.00906369458471356));
#37293=CARTESIAN_POINT('Ctrl Pts',(-0.227310930575325,0.0119192283365604,
-0.00956777733553797));
#37294=CARTESIAN_POINT('Ctrl Pts',(-0.227301909529503,0.0119391596141039,
-0.00955613795792144));
#37295=CARTESIAN_POINT('Ctrl Pts',(-0.227293027054935,0.0119591053495831,
-0.00954439308709731));
#37296=CARTESIAN_POINT('Ctrl Pts',(-0.227284273384487,0.0119790594444581,
-0.00953254512793306));
#37297=CARTESIAN_POINT('Ctrl Pts',(-0.227231597305896,0.012099135185951,
-0.00946124886063881));
#37298=CARTESIAN_POINT('Ctrl Pts',(-0.227183591614038,0.0122195086983642,
-0.0093862131580218));
#37299=CARTESIAN_POINT('Ctrl Pts',(-0.227138063814653,0.01233888863127,
-0.0093079134742992));
#37300=CARTESIAN_POINT('Ctrl Pts',(-0.227092536015269,0.0124582685641757,
-0.0092296137905766));
#37301=CARTESIAN_POINT('Ctrl Pts',(-0.227049486174156,0.0125766585785184,
-0.00914804828974315));
#37302=CARTESIAN_POINT('Ctrl Pts',(-0.227006637251675,0.0126927900142701,
-0.00906369458471356));
#37303=CARTESIAN_POINT('',(-0.22626372592396,0.0126609459515122,-0.00907137389400092));
#37304=CARTESIAN_POINT('Ctrl Pts',(-0.226263728585857,0.0126609457742137,
-0.00907137404226376));
#37305=CARTESIAN_POINT('Ctrl Pts',(-0.226386619259017,0.0126771073815086,
-0.00906231630609566));
#37306=CARTESIAN_POINT('Ctrl Pts',(-0.226510405436089,0.0126878531263563,
-0.0090570429094382));
#37307=CARTESIAN_POINT('Ctrl Pts',(-0.226758531947056,0.0126985222461932,
-0.00905426871011949));
#37308=CARTESIAN_POINT('Ctrl Pts',(-0.226882687732036,0.0126984539951922,
-0.00905675848878095));
#37309=CARTESIAN_POINT('Ctrl Pts',(-0.227006496256814,0.012692991252369,
-0.00906311899234723));
#37310=CARTESIAN_POINT('',(-0.226391100213263,0.0131362729035505,-0.00871148491867768));
#37311=CARTESIAN_POINT('Origin',(-0.227688300131171,0.00723376617371606,
-0.00189119032934214));
#37312=CARTESIAN_POINT('',(-0.225391419217308,0.0131367695109091,-0.00869218205150295));
#37313=CARTESIAN_POINT('Ctrl Pts',(-0.226391100213325,0.0131362728985425,
-0.00871148491535396));
#37314=CARTESIAN_POINT('Ctrl Pts',(-0.226224497789347,0.0131363544611319,
-0.00870826654206384));
#37315=CARTESIAN_POINT('Ctrl Pts',(-0.226057895192789,0.013136436623428,
-0.00870504888489742));
#37316=CARTESIAN_POINT('Ctrl Pts',(-0.225724668190818,0.013136602159935,
-0.00869861459466251));
#37317=CARTESIAN_POINT('Ctrl Pts',(-0.225558043667431,0.0131366855343623,
-0.00869539795950626));
#37318=CARTESIAN_POINT('Ctrl Pts',(-0.225391419217304,0.0131367695104093,
-0.00869218205167778));
#37319=CARTESIAN_POINT('',(-0.225267117543399,0.0126690414880847,-0.00904616167166099));
#37320=CARTESIAN_POINT('Origin',(-0.226746990060653,0.00723483562453479,
-0.00187833795146874));
#37321=CARTESIAN_POINT('',(-0.224973343469933,0.0127081065850716,-0.00901241391075122));
#37322=CARTESIAN_POINT('Ctrl Pts',(-0.224972872689331,0.0127080240555426,
-0.00901235812756441));
#37323=CARTESIAN_POINT('Ctrl Pts',(-0.225023054977778,0.0127112197679192,
-0.0090110474151989));
#37324=CARTESIAN_POINT('Ctrl Pts',(-0.2250734691889,0.012709520923146,-0.00901326014049183));
#37325=CARTESIAN_POINT('Ctrl Pts',(-0.225172251825652,0.0126964311153787,
-0.00902458937587981));
#37326=CARTESIAN_POINT('Ctrl Pts',(-0.225220266854037,0.0126851548120693,
-0.00903361573608797));
#37327=CARTESIAN_POINT('Ctrl Pts',(-0.225266060957984,0.0126693218437064,
-0.00904576810780379));
#37328=CARTESIAN_POINT('Ctrl Pts',(-0.225105867141788,0.0119077821064707,
-0.00952780373316783));
#37329=CARTESIAN_POINT('Ctrl Pts',(-0.225095444062685,0.0120459270894792,
-0.00944903969813657));
#37330=CARTESIAN_POINT('Ctrl Pts',(-0.225079187043228,0.0121814942140962,
-0.00936678104310605));
#37331=CARTESIAN_POINT('Ctrl Pts',(-0.225034785732628,0.012448678452175,
-0.00919471546264362));
#37332=CARTESIAN_POINT('Ctrl Pts',(-0.225006520539429,0.0125799968801818,
-0.00910496411764648));
#37333=CARTESIAN_POINT('Ctrl Pts',(-0.224972407900901,0.0127079109487015,
-0.0090124302414561));
#37334=CARTESIAN_POINT('Origin',(-0.203568281266003,0.00750000064956461,
-0.000977039010395701));
#37335=CARTESIAN_POINT('',(-0.203180932155927,0.0122574475529592,-0.00887884679402051));
#37336=CARTESIAN_POINT('',(-0.203099975589327,0.00748772692520692,-0.0102016315939729));
#37337=CARTESIAN_POINT('Ctrl Pts',(-0.203180932155927,0.0122574475529592,
-0.00887884679402051));
#37338=CARTESIAN_POINT('Ctrl Pts',(-0.203144389557098,0.0120211460710307,
-0.00902023995050872));
#37339=CARTESIAN_POINT('Ctrl Pts',(-0.203099004528403,0.0117059840990509,
-0.00918853528176113));
#37340=CARTESIAN_POINT('Ctrl Pts',(-0.203054201982351,0.0113485760860837,
-0.00935714677214135));
#37341=CARTESIAN_POINT('Ctrl Pts',(-0.203033800001085,0.0111722119519007,
-0.00943586125013318));
#37342=CARTESIAN_POINT('Ctrl Pts',(-0.203004790952906,0.0108566700800293,
-0.00956601535400645));
#37343=CARTESIAN_POINT('Ctrl Pts',(-0.202980217443486,0.010477728951912,
-0.00970594622761543));
#37344=CARTESIAN_POINT('Ctrl Pts',(-0.202964642390056,0.00996004413167459,
-0.0098682196553169));
#37345=CARTESIAN_POINT('Ctrl Pts',(-0.202970397699778,0.00949324515176631,
-0.00998162264848546));
#37346=CARTESIAN_POINT('Ctrl Pts',(-0.202983931631907,0.00912176212646602,
-0.0100529635069714));
#37347=CARTESIAN_POINT('Ctrl Pts',(-0.20299393266481,0.00891420132184156,
-0.0100873844335844));
#37348=CARTESIAN_POINT('Ctrl Pts',(-0.203004460841773,0.00872918961470634,
-0.0101141562984169));
#37349=CARTESIAN_POINT('Ctrl Pts',(-0.203010134685348,0.00864074678625943,
-0.0101255182078198));
#37350=CARTESIAN_POINT('Ctrl Pts',(-0.203021726690619,0.00846795517814871,
-0.0101463016488843));
#37351=CARTESIAN_POINT('Ctrl Pts',(-0.203045893326094,0.00813922185990422,
-0.01017849081334));
#37352=CARTESIAN_POINT('Ctrl Pts',(-0.203075503013031,0.00777516939207381,
-0.0101975550358818));
#37353=CARTESIAN_POINT('Ctrl Pts',(-0.203099132557942,0.00750037293252254,
-0.0101980787679676));
#37354=CARTESIAN_POINT('',(-0.203173200311358,0.00274689768564807,-0.008881289974441));
#37355=CARTESIAN_POINT('Ctrl Pts',(-0.203103782510698,0.00748459366645466,
-0.0101981667986033));
#37356=CARTESIAN_POINT('Ctrl Pts',(-0.203056815772698,0.00710265220262713,
-0.0101965099598228));
#37357=CARTESIAN_POINT('Ctrl Pts',(-0.203021349803096,0.0067170805498119,
-0.0101713884403401));
#37358=CARTESIAN_POINT('Ctrl Pts',(-0.202934394875737,0.00526489448036165,
-0.00998387785797495));
#37359=CARTESIAN_POINT('Ctrl Pts',(-0.202965303386757,0.00422151948414504,
-0.0096619097669541));
#37360=CARTESIAN_POINT('Ctrl Pts',(-0.203118124523932,0.00308108700338837,
-0.0090738493251725));
#37361=CARTESIAN_POINT('Ctrl Pts',(-0.203144125164855,0.00291254238670889,
-0.00898020598093925));
#37362=CARTESIAN_POINT('Ctrl Pts',(-0.203173200310812,0.00274689768556089,
-0.00888128997442626));
#37363=CARTESIAN_POINT('',(-0.204179808594537,0.00274695694953536,-0.00890316850546251));
#37364=CARTESIAN_POINT('Ctrl Pts',(-0.203173200311351,0.00274689768609342,
-0.00888128997475801));
#37365=CARTESIAN_POINT('Ctrl Pts',(-0.203511887957009,0.00274691735937696,
-0.00888865115679395));
#37366=CARTESIAN_POINT('Ctrl Pts',(-0.2038476742076,0.00274693265699481,
-0.00889594675021198));
#37367=CARTESIAN_POINT('Ctrl Pts',(-0.204179864222553,0.00274694378498237,
-0.00890316180123792));
#37368=CARTESIAN_POINT('',(-0.204098753207029,0.00750019449511319,-0.010219767218868));
#37369=CARTESIAN_POINT('Ctrl Pts',(-0.204179808594537,0.00274695694953536,
-0.00890316850546251));
#37370=CARTESIAN_POINT('Ctrl Pts',(-0.204143308707588,0.00298395730820233,
-0.0090448031502624));
#37371=CARTESIAN_POINT('Ctrl Pts',(-0.204097954903568,0.00330018647005424,
-0.00921338606909646));
#37372=CARTESIAN_POINT('Ctrl Pts',(-0.204053158933222,0.00365864570901938,
-0.00938214415921903));
#37373=CARTESIAN_POINT('Ctrl Pts',(-0.204032678472951,0.00383632055569296,
-0.00946122584533509));
#37374=CARTESIAN_POINT('Ctrl Pts',(-0.204003768789267,0.00415082622990258,
-0.00959060202023825));
#37375=CARTESIAN_POINT('Ctrl Pts',(-0.203979179919398,0.00452842436729695,
-0.00972964246551787));
#37376=CARTESIAN_POINT('Ctrl Pts',(-0.203963454897067,0.00503954981670578,
-0.00988970685319689));
#37377=CARTESIAN_POINT('Ctrl Pts',(-0.203968942557704,0.00550841835918545,
-0.0100036492041412));
#37378=CARTESIAN_POINT('Ctrl Pts',(-0.203982363369764,0.00587797498451415,
-0.0100745671040912));
#37379=CARTESIAN_POINT('Ctrl Pts',(-0.20399231704185,0.00608447450262321,
-0.0101088319704821));
#37380=CARTESIAN_POINT('Ctrl Pts',(-0.204002786998696,0.00626792725225948,
-0.0101354241310119));
#37381=CARTESIAN_POINT('Ctrl Pts',(-0.204008516600288,0.00635676412948642,
-0.0101468715278863));
#37382=CARTESIAN_POINT('Ctrl Pts',(-0.204020200606318,0.00652958263497338,
-0.0101677050009321));
#37383=CARTESIAN_POINT('Ctrl Pts',(-0.204044661227922,0.00685904773966244,
-0.0102000610115712));
#37384=CARTESIAN_POINT('Ctrl Pts',(-0.20407472551262,0.00722428924687252,
-0.0102192517952231));
#37385=CARTESIAN_POINT('Ctrl Pts',(-0.204098753205607,0.00750019441693834,
-0.0102197672188388));
#37386=CARTESIAN_POINT('',(-0.204181212510367,0.0122570585516106,-0.00890078076054459));
#37387=CARTESIAN_POINT('Ctrl Pts',(-0.204098753207029,0.00750019449511319,
-0.010219767218868));
#37388=CARTESIAN_POINT('Ctrl Pts',(-0.204074969826491,0.00777525417200037,
-0.010219245316851));
#37389=CARTESIAN_POINT('Ctrl Pts',(-0.20404518935886,0.00813953722805785,
-0.0102001521705759));
#37390=CARTESIAN_POINT('Ctrl Pts',(-0.204020924281112,0.00846830075501304,
-0.0101679429006501));
#37391=CARTESIAN_POINT('Ctrl Pts',(-0.204009307531493,0.00864098654128726,
-0.0101471667925929));
#37392=CARTESIAN_POINT('Ctrl Pts',(-0.204003623011863,0.00872944215982944,
-0.0101357983481098));
#37393=CARTESIAN_POINT('Ctrl Pts',(-0.203993124102833,0.00891393094068779,
-0.0101091022096258));
#37394=CARTESIAN_POINT('Ctrl Pts',(-0.203983158153701,0.00912121165876486,
-0.010074736990353));
#37395=CARTESIAN_POINT('Ctrl Pts',(-0.203969711708032,0.00949232807053968,
-0.0100035209917527));
#37396=CARTESIAN_POINT('Ctrl Pts',(-0.203964148109392,0.00996155782354372,
-0.00988948548415189));
#37397=CARTESIAN_POINT('Ctrl Pts',(-0.203979984609945,0.0104768772720125,
-0.00972790469770468));
#37398=CARTESIAN_POINT('Ctrl Pts',(-0.204004794840732,0.0108561848221544,
-0.00958791591559206));
#37399=CARTESIAN_POINT('Ctrl Pts',(-0.204034076180802,0.0111727868553702,
-0.00945731833040206));
#37400=CARTESIAN_POINT('Ctrl Pts',(-0.204054512850181,0.0113489102407224,
-0.00937869140214235));
#37401=CARTESIAN_POINT('Ctrl Pts',(-0.204099372796569,0.0117062274665102,
-0.00921011084626496));
#37402=CARTESIAN_POINT('Ctrl Pts',(-0.204144720651052,0.0120210387403513,
-0.009041989911057));
#37403=CARTESIAN_POINT('Ctrl Pts',(-0.204181212510367,0.0122570585516106,
-0.00890078076054459));
#37404=CARTESIAN_POINT('Ctrl Pts',(-0.204181268812703,0.012257066354676,
-0.00890077728725559));
#37405=CARTESIAN_POINT('Ctrl Pts',(-0.203847894597336,0.0122571900460014,
-0.00889347070490962));
#37406=CARTESIAN_POINT('Ctrl Pts',(-0.203514406607199,0.0122573177004729,
-0.00888615926607952));
#37407=CARTESIAN_POINT('Ctrl Pts',(-0.203181012549154,0.0122574492374588,
-0.00887884752447026));
#37408=CARTESIAN_POINT('Origin',(-0.205569668377583,0.00750000053546121,
-0.00105476362107362));
#37409=CARTESIAN_POINT('',(-0.205181486251685,0.0122552975429564,-0.00891989779273504));
#37410=CARTESIAN_POINT('',(-0.205098440188702,0.00750015102883512,-0.0102432543024386));
#37411=CARTESIAN_POINT('Ctrl Pts',(-0.205181486251685,0.0122552975429564,
-0.00891989779273504));
#37412=CARTESIAN_POINT('Ctrl Pts',(-0.205145010746124,0.0120195671299043,
-0.00906154417007191));
#37413=CARTESIAN_POINT('Ctrl Pts',(-0.205099665823808,0.0117050967237337,
-0.00923018880615341));
#37414=CARTESIAN_POINT('Ctrl Pts',(-0.20505473701453,0.0113479801935507,
-0.00939935025380538));
#37415=CARTESIAN_POINT('Ctrl Pts',(-0.205034268942562,0.0111721994041601,
-0.00947814554233864));
#37416=CARTESIAN_POINT('Ctrl Pts',(-0.205004748571038,0.0108549239719047,
-0.00960952696160696));
#37417=CARTESIAN_POINT('Ctrl Pts',(-0.204979722424145,0.010475498663842,
-0.00975002068728981));
#37418=CARTESIAN_POINT('Ctrl Pts',(-0.20496362799297,0.00996219476279488,
-0.00991159079101826));
#37419=CARTESIAN_POINT('Ctrl Pts',(-0.204969004055025,0.00949117200399576,
-0.0100264939808952));
#37420=CARTESIAN_POINT('Ctrl Pts',(-0.204982377945537,0.009120408049961,
-0.010097842256249));
#37421=CARTESIAN_POINT('Ctrl Pts',(-0.204992318932816,0.0089133766789427,
-0.0101322743370575));
#37422=CARTESIAN_POINT('Ctrl Pts',(-0.205002800013507,0.00872932653396566,
-0.0101589956283636));
#37423=CARTESIAN_POINT('Ctrl Pts',(-0.205008498844975,0.00864085623694867,
-0.0101704072675598));
#37424=CARTESIAN_POINT('Ctrl Pts',(-0.205020148419491,0.00846828167738281,
-0.0101912420545331));
#37425=CARTESIAN_POINT('Ctrl Pts',(-0.205044525931656,0.00813958304043702,
-0.0102235622044265));
#37426=CARTESIAN_POINT('Ctrl Pts',(-0.205074491969353,0.00777527627334546,
-0.010242729856909));
#37427=CARTESIAN_POINT('Ctrl Pts',(-0.205098440307258,0.00750015170665339,
-0.0102432543053281));
#37428=CARTESIAN_POINT('',(-0.205180409732413,0.00274852659771838,-0.00892218213689432));
#37429=CARTESIAN_POINT('Ctrl Pts',(-0.205098440247425,0.00750015102368582,
-0.0102432543040401));
#37430=CARTESIAN_POINT('Ctrl Pts',(-0.205093952951413,0.00744893039446262,
-0.0102431577065131));
#37431=CARTESIAN_POINT('Ctrl Pts',(-0.205080198588494,0.00729028603855544,
-0.0102413201101437));
#37432=CARTESIAN_POINT('Ctrl Pts',(-0.205060248277069,0.00705318842883126,
-0.0102327637584102));
#37433=CARTESIAN_POINT('Ctrl Pts',(-0.205037071982337,0.00676558988861412,
-0.0102143707027614));
#37434=CARTESIAN_POINT('Ctrl Pts',(-0.205019741813002,0.00653305075314794,
-0.01019134977702));
#37435=CARTESIAN_POINT('Ctrl Pts',(-0.205008015508058,0.00636038697474645,
-0.0101705570943968));
#37436=CARTESIAN_POINT('Ctrl Pts',(-0.205002287358874,0.00627190834821762,
-0.0101591465651645));
#37437=CARTESIAN_POINT('Ctrl Pts',(-0.204991791760696,0.00608850277435127,
-0.0101325524012929));
#37438=CARTESIAN_POINT('Ctrl Pts',(-0.204981832022474,0.00588182305608673,
-0.0100982193342052));
#37439=CARTESIAN_POINT('Ctrl Pts',(-0.204968413283859,0.00551192613026262,
-0.0100272159798676));
#37440=CARTESIAN_POINT('Ctrl Pts',(-0.204963297415599,0.00503789180459126,
-0.00991130245284762));
#37441=CARTESIAN_POINT('Ctrl Pts',(-0.204978689645553,0.00453288307852895,
-0.00975337405009284));
#37442=CARTESIAN_POINT('Ctrl Pts',(-0.205001886359724,0.00418947678318943,
-0.00962547804925551));
#37443=CARTESIAN_POINT('Ctrl Pts',(-0.205017689619932,0.00400142298949485,
-0.00955045506899675));
#37444=CARTESIAN_POINT('Ctrl Pts',(-0.205033338680103,0.00384193801459521,
-0.00948318984329787));
#37445=CARTESIAN_POINT('Ctrl Pts',(-0.205042517205282,0.00375845349593796,
-0.00944652183840551));
#37446=CARTESIAN_POINT('Ctrl Pts',(-0.205060590791516,0.00360208362519979,
-0.00937617788322102));
#37447=CARTESIAN_POINT('Ctrl Pts',(-0.205098306119765,0.00330504246940279,
-0.00923472043191907));
#37448=CARTESIAN_POINT('Ctrl Pts',(-0.205144087161525,0.00298418033850801,
-0.00906362922856368));
#37449=CARTESIAN_POINT('Ctrl Pts',(-0.205180409732413,0.00274852659771838,
-0.00892218213689432));
#37450=CARTESIAN_POINT('',(-0.206180961328082,0.00274847806016448,-0.00894387894537355));
#37451=CARTESIAN_POINT('Ctrl Pts',(-0.205180479464195,0.00274853066302267,
-0.00892218610479268));
#37452=CARTESIAN_POINT('Ctrl Pts',(-0.205511119540387,0.00274851289143719,
-0.00892935493901173));
#37453=CARTESIAN_POINT('Ctrl Pts',(-0.205844838618331,0.00274849107317641,
-0.00893658818851419));
#37454=CARTESIAN_POINT('Ctrl Pts',(-0.206181011406301,0.00274846505131942,
-0.00894387218078926));
#37455=CARTESIAN_POINT('',(-0.206098160870363,0.00750010608734745,-0.010264959897942));
#37456=CARTESIAN_POINT('Ctrl Pts',(-0.206180961328082,0.00274847806016448,
-0.00894387894537355));
#37457=CARTESIAN_POINT('Ctrl Pts',(-0.206144503244658,0.0029851394815468,
-0.00908593313274618));
#37458=CARTESIAN_POINT('Ctrl Pts',(-0.206099163905087,0.00330094991332194,
-0.00925502338592517));
#37459=CARTESIAN_POINT('Ctrl Pts',(-0.206054223946957,0.00365935700615154,
-0.00942444106050021));
#37460=CARTESIAN_POINT('Ctrl Pts',(-0.206033685907648,0.00383642966844798,
-0.00950359601200414));
#37461=CARTESIAN_POINT('Ctrl Pts',(-0.206004239839081,0.00415297153187771,
-0.00963430969563866));
#37462=CARTESIAN_POINT('Ctrl Pts',(-0.20597916333659,0.00453120900848722,
-0.00977393705103434));
#37463=CARTESIAN_POINT('Ctrl Pts',(-0.20596285353138,0.0050377641666255,
-0.00993320305773024));
#37464=CARTESIAN_POINT('Ctrl Pts',(-0.205967863395825,0.00551099034506471,
-0.0100486504485952));
#37465=CARTESIAN_POINT('Ctrl Pts',(-0.205981049669001,0.00587956688186075,
-0.0101195069636298));
#37466=CARTESIAN_POINT('Ctrl Pts',(-0.205990901558899,0.00608537450600959,
-0.0101537508288514));
#37467=CARTESIAN_POINT('Ctrl Pts',(-0.206001282208726,0.00626761766659463,
-0.0101802563825301));
#37468=CARTESIAN_POINT('Ctrl Pts',(-0.206007030871337,0.00635656589256591,
-0.0101917668973418));
#37469=CARTESIAN_POINT('Ctrl Pts',(-0.206018754543683,0.006529146193304,
-0.0102126501798417));
#37470=CARTESIAN_POINT('Ctrl Pts',(-0.20604340588525,0.00685855965021963,
-0.0102451399879971));
#37471=CARTESIAN_POINT('Ctrl Pts',(-0.206073816600126,0.00722395965705849,
-0.0102644346030527));
#37472=CARTESIAN_POINT('Ctrl Pts',(-0.206098160870452,0.00750010608733958,
-0.0102649598979439));
#37473=CARTESIAN_POINT('',(-0.206181715574144,0.0122551196169534,-0.00894171946680973));
#37474=CARTESIAN_POINT('Ctrl Pts',(-0.206098160870363,0.00750010608734745,
-0.010264959897942));
#37475=CARTESIAN_POINT('Ctrl Pts',(-0.206074054827856,0.00777528552125095,
-0.0102644332675757));
#37476=CARTESIAN_POINT('Ctrl Pts',(-0.206043911255022,0.00813957901293385,
-0.0102452587525356));
#37477=CARTESIAN_POINT('Ctrl Pts',(-0.206019426951112,0.00846815073558031,
-0.0102129497512625));
#37478=CARTESIAN_POINT('Ctrl Pts',(-0.206007747489499,0.0086405593599698,
-0.0101921395316813));
#37479=CARTESIAN_POINT('Ctrl Pts',(-0.206002034855823,0.0087290293396645,
-0.0101807278839575));
#37480=CARTESIAN_POINT('Ctrl Pts',(-0.205991576991469,0.00891250482133831,
-0.0101541029899592));
#37481=CARTESIAN_POINT('Ctrl Pts',(-0.205981666019672,0.00911922871637835,
-0.0101197394207395));
#37482=CARTESIAN_POINT('Ctrl Pts',(-0.20596833683428,0.0094893100438307,
-0.0100486653436722));
#37483=CARTESIAN_POINT('Ctrl Pts',(-0.205963343815955,0.0099645263554711,
-0.00993235088092946));
#37484=CARTESIAN_POINT('Ctrl Pts',(-0.205978910244621,0.0104689773112782,
-0.00977445835237511));
#37485=CARTESIAN_POINT('Ctrl Pts',(-0.206002303757198,0.0108128077782491,
-0.00964632045704586));
#37486=CARTESIAN_POINT('Ctrl Pts',(-0.206018229482252,0.0110011334046898,
-0.00957112831725541));
#37487=CARTESIAN_POINT('Ctrl Pts',(-0.206033997054145,0.0111609344223277,
-0.00950367117882155));
#37488=CARTESIAN_POINT('Ctrl Pts',(-0.206043234920356,0.0112445506318481,
-0.00946691067775824));
#37489=CARTESIAN_POINT('Ctrl Pts',(-0.206061414877685,0.0114011476494823,
-0.00939639690988238));
#37490=CARTESIAN_POINT('Ctrl Pts',(-0.206099313687172,0.0116984707478102,
-0.00925466076457502));
#37491=CARTESIAN_POINT('Ctrl Pts',(-0.206145270450179,0.0120194511993669,
-0.00908332193822784));
#37492=CARTESIAN_POINT('Ctrl Pts',(-0.206181715574144,0.0122551196169534,
-0.00894171946680973));
#37493=CARTESIAN_POINT('Ctrl Pts',(-0.206181766675709,0.0122551273964408,
-0.00894171587571898));
#37494=CARTESIAN_POINT('Ctrl Pts',(-0.205849139539492,0.0122551803210089,
-0.0089344628329478));
#37495=CARTESIAN_POINT('Ctrl Pts',(-0.205515630029343,0.0122552371745374,
-0.00892718825993729));
#37496=CARTESIAN_POINT('Ctrl Pts',(-0.205181559737592,0.0122552979498864,
-0.0089198991421701));
#37497=CARTESIAN_POINT('Origin',(-0.207569531999201,0.00750000042399001,
-0.0011316682782873));
#37498=CARTESIAN_POINT('',(-0.207182021343611,0.0122531890606491,-0.00896101780551548));
#37499=CARTESIAN_POINT('',(-0.207097778441897,0.00750000135331723,-0.0102884291114441));
#37500=CARTESIAN_POINT('Ctrl Pts',(-0.207182021343611,0.0122531890606491,
-0.00896101780551548));
#37501=CARTESIAN_POINT('Ctrl Pts',(-0.207145589529982,0.012017810159708,
-0.00910303844719066));
#37502=CARTESIAN_POINT('Ctrl Pts',(-0.207114946631626,0.0118040522654641,
-0.00921766339889173));
#37503=CARTESIAN_POINT('Ctrl Pts',(-0.207090279354578,0.0116196010293119,
-0.00930996556537863));
#37504=CARTESIAN_POINT('Ctrl Pts',(-0.207077945716054,0.0115273754112358,
-0.00935611664862208));
#37505=CARTESIAN_POINT('Ctrl Pts',(-0.207067105565684,0.0114424881905947,
-0.00939670623860649));
#37506=CARTESIAN_POINT('Ctrl Pts',(-0.207057415290073,0.0113620447273888,
-0.00943388414297075));
#37507=CARTESIAN_POINT('Ctrl Pts',(-0.207052570152267,0.0113218229957858,
-0.00945247309515288));
#37508=CARTESIAN_POINT('Ctrl Pts',(-0.207048013105317,0.0112826983783498,
-0.00947018048739905));
#37509=CARTESIAN_POINT('Ctrl Pts',(-0.20704419346178,0.0112492058999985,
-0.00948511621392071));
#37510=CARTESIAN_POINT('Ctrl Pts',(-0.207040373818242,0.0112157134216472,
-0.00950005194044236));
#37511=CARTESIAN_POINT('Ctrl Pts',(-0.207037289600169,0.0111878944163724,
-0.00951230704660541));
#37512=CARTESIAN_POINT('Ctrl Pts',(-0.207033098186437,0.0111473183720926,
-0.00952982204190615));
#37513=CARTESIAN_POINT('Ctrl Pts',(-0.207028906772705,0.0111067423278128,
-0.00954733703720688));
#37514=CARTESIAN_POINT('Ctrl Pts',(-0.207023611716941,0.0110533378977748,
-0.00956994834796696));
#37515=CARTESIAN_POINT('Ctrl Pts',(-0.207018960141398,0.0110030579020677,
-0.00959064979089299));
#37516=CARTESIAN_POINT('Ctrl Pts',(-0.207014308565855,0.0109527779063606,
-0.00961135123381902));
#37517=CARTESIAN_POINT('Ctrl Pts',(-0.20701029799187,0.0109056687548309,
-0.00963025690129191));
#37518=CARTESIAN_POINT('Ctrl Pts',(-0.207006500480265,0.0108578827174683,
-0.00964899548438834));
#37519=CARTESIAN_POINT('Ctrl Pts',(-0.206998905457053,0.0107623106427431,
-0.00968647265058121));
#37520=CARTESIAN_POINT('Ctrl Pts',(-0.206992165145035,0.0106639906501456,
-0.00972316816953493));
#37521=CARTESIAN_POINT('Ctrl Pts',(-0.206986617295028,0.0105649667408118,
-0.0097581953819392));
#37522=CARTESIAN_POINT('Ctrl Pts',(-0.206975521595013,0.0103669189221444,
-0.00982824980674773));
#37523=CARTESIAN_POINT('Ctrl Pts',(-0.20696919711927,0.0101660098746444,
-0.00989156765480013));
#37524=CARTESIAN_POINT('Ctrl Pts',(-0.206967001402819,0.0099701265364059,
-0.00994635646975916));
#37525=CARTESIAN_POINT('Ctrl Pts',(-0.206964805686368,0.00977424319816743,
-0.0100011452847182));
#37526=CARTESIAN_POINT('Ctrl Pts',(-0.206966726116684,0.00958356196070715,
-0.0100479856097936));
#37527=CARTESIAN_POINT('Ctrl Pts',(-0.206972407397417,0.00937916938864513,
-0.0100909377062068));
#37528=CARTESIAN_POINT('Ctrl Pts',(-0.206975248037783,0.00927697310261412,
-0.0101124137544134));
#37529=CARTESIAN_POINT('Ctrl Pts',(-0.206979032483084,0.0091713144408141,
-0.0101327523961511));
#37530=CARTESIAN_POINT('Ctrl Pts',(-0.206983588109306,0.0090672379345247,
-0.0101509193285515));
#37531=CARTESIAN_POINT('Ctrl Pts',(-0.206985865922417,0.00901519968138,
-0.0101600027947517));
#37532=CARTESIAN_POINT('Ctrl Pts',(-0.206988335561166,0.00896356508380256,
-0.0101685879622218));
#37533=CARTESIAN_POINT('Ctrl Pts',(-0.206991307138919,0.00890723708154231,
-0.0101774073832468));
#37534=CARTESIAN_POINT('Ctrl Pts',(-0.206994278716672,0.00885090907928206,
-0.0101862268042718));
#37535=CARTESIAN_POINT('Ctrl Pts',(-0.20699775554717,0.00878986325834849,
-0.0101951279537617));
#37536=CARTESIAN_POINT('Ctrl Pts',(-0.207000448895413,0.00874458601643362,
-0.0102013940653026));
#37537=CARTESIAN_POINT('Ctrl Pts',(-0.207003142243657,0.00869930877451875,
-0.0102076601768436));
#37538=CARTESIAN_POINT('Ctrl Pts',(-0.207005047495907,0.00866982864377494,
-0.0102115036111103));
#37539=CARTESIAN_POINT('Ctrl Pts',(-0.207007461526474,0.00863355577397413,
-0.0102160782502125));
#37540=CARTESIAN_POINT('Ctrl Pts',(-0.207009875557042,0.00859728290417331,
-0.0102206528893147));
#37541=CARTESIAN_POINT('Ctrl Pts',(-0.20701280082912,0.00855420375341624,
-0.0102258453580294));
#37542=CARTESIAN_POINT('Ctrl Pts',(-0.207015921463241,0.0085098402872069,
-0.0102308325011764));
#37543=CARTESIAN_POINT('Ctrl Pts',(-0.207022162731483,0.00842111335478822,
-0.0102408067874703));
#37544=CARTESIAN_POINT('Ctrl Pts',(-0.207029182339711,0.00832726285498634,
-0.0102501028339772));
#37545=CARTESIAN_POINT('Ctrl Pts',(-0.207037228948747,0.00822421591382894,
-0.0102584479867199));
#37546=CARTESIAN_POINT('Ctrl Pts',(-0.20705332216682,0.00801812203151415,
-0.0102751382922053));
#37547=CARTESIAN_POINT('Ctrl Pts',(-0.207073526056755,0.00777524126012205,
-0.0102879021939248));
#37548=CARTESIAN_POINT('Ctrl Pts',(-0.207097778441897,0.00750000135331723,
-0.0102884291114441));
#37549=CARTESIAN_POINT('',(-0.207181532792705,0.00275005700218644,-0.0089629743514168));
#37550=CARTESIAN_POINT('Ctrl Pts',(-0.207097778313067,0.00749999989891767,
-0.010288429108645));
#37551=CARTESIAN_POINT('Ctrl Pts',(-0.207073419625904,0.00722500789874744,
-0.0102878998379192));
#37552=CARTESIAN_POINT('Ctrl Pts',(-0.207042990834877,0.006861018988083,
-0.0102686874301281));
#37553=CARTESIAN_POINT('Ctrl Pts',(-0.207018331514006,0.00653274297319404,
-0.0102363194044195));
#37554=CARTESIAN_POINT('Ctrl Pts',(-0.207006602442421,0.00636060530882933,
-0.0102154904597151));
#37555=CARTESIAN_POINT('Ctrl Pts',(-0.207000862677054,0.00627205965399394,
-0.0102040358443934));
#37556=CARTESIAN_POINT('Ctrl Pts',(-0.206990449366781,0.00608957659382692,
-0.0101774937656562));
#37557=CARTESIAN_POINT('Ctrl Pts',(-0.206980590513266,0.0058834710399858,
-0.0101431671415748));
#37558=CARTESIAN_POINT('Ctrl Pts',(-0.206967394593663,0.00551434385411936,
-0.0100721886506396));
#37559=CARTESIAN_POINT('Ctrl Pts',(-0.206962734755496,0.00503619279538927,
-0.00995481286789569));
#37560=CARTESIAN_POINT('Ctrl Pts',(-0.20697864418332,0.00453579661021954,
-0.00979775023715801));
#37561=CARTESIAN_POINT('Ctrl Pts',(-0.207002283619446,0.00419160943361069,
-0.00966922538535609));
#37562=CARTESIAN_POINT('Ctrl Pts',(-0.207018336605471,0.00400301457636903,
-0.00959373456705133));
#37563=CARTESIAN_POINT('Ctrl Pts',(-0.207034242024311,0.0038424762579756,
-0.00952577398159521));
#37564=CARTESIAN_POINT('Ctrl Pts',(-0.20704345921084,0.00375923635338582,
-0.00948906520200336));
#37565=CARTESIAN_POINT('Ctrl Pts',(-0.207061638331585,0.00360277318013875,
-0.00941840556840703));
#37566=CARTESIAN_POINT('Ctrl Pts',(-0.207099453178564,0.0033059120017622,
-0.00927646000782889));
#37567=CARTESIAN_POINT('Ctrl Pts',(-0.207145244487981,0.00298536163401571,
-0.00910481968417944));
#37568=CARTESIAN_POINT('Ctrl Pts',(-0.207181532792705,0.00275005700218644,
-0.0089629743514168));
#37569=CARTESIAN_POINT('',(-0.208182049566434,0.00275001859964783,-0.00898469078812813));
#37570=CARTESIAN_POINT('Ctrl Pts',(-0.207181595750663,0.00275006108290852,
-0.00896297819299416));
#37571=CARTESIAN_POINT('Ctrl Pts',(-0.207511950573292,0.00275004656769739,
-0.00897014750465242));
#37572=CARTESIAN_POINT('Ctrl Pts',(-0.207845671547403,0.00275002816037635,
-0.00897738759838072));
#37573=CARTESIAN_POINT('Ctrl Pts',(-0.208182094596618,0.0027500056881023,
-0.00898468393992406));
#37574=CARTESIAN_POINT('',(-0.208097512100336,0.00749999999333244,-0.0103101497453589));
#37575=CARTESIAN_POINT('Ctrl Pts',(-0.208182049566434,0.00275001859964783,
-0.00898469078812813));
#37576=CARTESIAN_POINT('Ctrl Pts',(-0.208145638937197,0.00298627876255052,
-0.00912711411657463));
#37577=CARTESIAN_POINT('Ctrl Pts',(-0.208099688434819,0.00330817190051734,
-0.0092993952508412));
#37578=CARTESIAN_POINT('Ctrl Pts',(-0.208061716122496,0.00360646955884461,
-0.00944187715419658));
#37579=CARTESIAN_POINT('Ctrl Pts',(-0.208043467883132,0.00376356938216498,
-0.00951273322332168));
#37580=CARTESIAN_POINT('Ctrl Pts',(-0.208034173093545,0.00384757541839402,
-0.00954971832383919));
#37581=CARTESIAN_POINT('Ctrl Pts',(-0.208018311977663,0.00400760211155766,
-0.00961734982946915));
#37582=CARTESIAN_POINT('Ctrl Pts',(-0.208002254883357,0.00419574367676322,
-0.00969254902841235));
#37583=CARTESIAN_POINT('Ctrl Pts',(-0.207978587895246,0.00453876056307716,
-0.0098204277346072));
#37584=CARTESIAN_POINT('Ctrl Pts',(-0.207962491805793,0.00503450927170103,
-0.00997600800815991));
#37585=CARTESIAN_POINT('Ctrl Pts',(-0.207966830101282,0.00551329932707707,
-0.0100936573257618));
#37586=CARTESIAN_POINT('Ctrl Pts',(-0.207979805946424,0.00588082572595351,
-0.0101643937148489));
#37587=CARTESIAN_POINT('Ctrl Pts',(-0.20798954667625,0.00608609437374459,
-0.0101986511546884));
#37588=CARTESIAN_POINT('Ctrl Pts',(-0.20799983239929,0.00626736392668125,
-0.0102251009669269));
#37589=CARTESIAN_POINT('Ctrl Pts',(-0.208005585937768,0.00635637311449185,
-0.0102366662104294));
#37590=CARTESIAN_POINT('Ctrl Pts',(-0.208017332757161,0.006528741960817,
-0.0102576007511969));
#37591=CARTESIAN_POINT('Ctrl Pts',(-0.208042143315929,0.00685809179282729,
-0.0102902189911923));
#37592=CARTESIAN_POINT('Ctrl Pts',(-0.20807287172922,0.00722363415368649,
-0.0103096143982934));
#37593=CARTESIAN_POINT('Ctrl Pts',(-0.208097512282003,0.00749999794611554,
-0.0103101497493061));
#37594=CARTESIAN_POINT('',(-0.208182230285086,0.0122530779316807,-0.00898281412196308));
#37595=CARTESIAN_POINT('Ctrl Pts',(-0.208097512100336,0.00749999999333126,
-0.0103101497453589));
#37596=CARTESIAN_POINT('Ctrl Pts',(-0.208073095868969,0.00777529216228051,
-0.0103096192065392));
#37597=CARTESIAN_POINT('Ctrl Pts',(-0.208052770097806,0.00801816593243897,
-0.0102968489434138));
#37598=CARTESIAN_POINT('Ctrl Pts',(-0.208036595893026,0.00822421145027163,
-0.0102801607371037));
#37599=CARTESIAN_POINT('Ctrl Pts',(-0.208028508790636,0.00832723420918796,
-0.0102718166339487));
#37600=CARTESIAN_POINT('Ctrl Pts',(-0.208021458921539,0.00842105016711052,
-0.0102625233446917));
#37601=CARTESIAN_POINT('Ctrl Pts',(-0.208015198382678,0.00850971509292231,
-0.0102525567157745));
#37602=CARTESIAN_POINT('Ctrl Pts',(-0.208012068113248,0.0085540475558282,
-0.0102475734013159));
#37603=CARTESIAN_POINT('Ctrl Pts',(-0.208009135949875,0.00859708885229161,
-0.0102423861496861));
#37604=CARTESIAN_POINT('Ctrl Pts',(-0.208006716705287,0.00863334075408494,
-0.0102378148682447));
#37605=CARTESIAN_POINT('Ctrl Pts',(-0.208004297460699,0.00866959265587827,
-0.0102332435868033));
#37606=CARTESIAN_POINT('Ctrl Pts',(-0.20800238868474,0.00869906863367712,
-0.0102294010507216));
#37607=CARTESIAN_POINT('Ctrl Pts',(-0.207999697808039,0.00874426209474986,
-0.0102231481050333));
#37608=CARTESIAN_POINT('Ctrl Pts',(-0.207997006931337,0.0087894555558226,
-0.010216895159345));
#37609=CARTESIAN_POINT('Ctrl Pts',(-0.20799353853445,0.00885033817316214,
-0.0102080209706738));
#37610=CARTESIAN_POINT('Ctrl Pts',(-0.207990574887146,0.00890654940277088,
-0.0101992242222599));
#37611=CARTESIAN_POINT('Ctrl Pts',(-0.207987611239842,0.00896276063237962,
-0.010190427473846));
#37612=CARTESIAN_POINT('Ctrl Pts',(-0.207985149057711,0.00901432467196044,
-0.0101818593407826));
#37613=CARTESIAN_POINT('Ctrl Pts',(-0.207982879750747,0.00906629658792817,
-0.0101727931378578));
#37614=CARTESIAN_POINT('Ctrl Pts',(-0.20797834113682,0.00917024041986364,
-0.010154660732008));
#37615=CARTESIAN_POINT('Ctrl Pts',(-0.207974577832061,0.00927578369170264,
-0.0101343607483211));
#37616=CARTESIAN_POINT('Ctrl Pts',(-0.207971762511418,0.00937804782437877,
-0.0101128843431944));
#37617=CARTESIAN_POINT('Ctrl Pts',(-0.207966131870133,0.00958257608973103,
-0.0100699315329408));
#37618=CARTESIAN_POINT('Ctrl Pts',(-0.20796427977108,0.0097741179809218,
-0.0100228895524523));
#37619=CARTESIAN_POINT('Ctrl Pts',(-0.207966549569727,0.00996992151477133,
-0.00996812951220845));
#37620=CARTESIAN_POINT('Ctrl Pts',(-0.207968819368374,0.0101657250486209,
-0.00991336947196463));
#37621=CARTESIAN_POINT('Ctrl Pts',(-0.207975222005227,0.0103656352498877,
-0.00985038778992463));
#37622=CARTESIAN_POINT('Ctrl Pts',(-0.207986417905805,0.010563559735708,
-0.00978041553776925));
#37623=CARTESIAN_POINT('Ctrl Pts',(-0.207992015856095,0.0106625219786182,
-0.00974542941169156));
#37624=CARTESIAN_POINT('Ctrl Pts',(-0.20799881204306,0.0107609944554867,
-0.00970869929203595));
#37625=CARTESIAN_POINT('Ctrl Pts',(-0.208006463466485,0.0108567448312281,
-0.00967116784099722));
#37626=CARTESIAN_POINT('Ctrl Pts',(-0.208010289178198,0.0109046200190988,
-0.00965240211547786));
#37627=CARTESIAN_POINT('Ctrl Pts',(-0.208014328064145,0.0109518251710427,
-0.00963346528036175));
#37628=CARTESIAN_POINT('Ctrl Pts',(-0.20801901390864,0.0110022628486564,
-0.00961270486607612));
#37629=CARTESIAN_POINT('Ctrl Pts',(-0.208023699753135,0.0110527005262702,
-0.0095919444517905));
#37630=CARTESIAN_POINT('Ctrl Pts',(-0.208029035072463,0.0111063236122112,
-0.00956924463408429));
#37631=CARTESIAN_POINT('Ctrl Pts',(-0.20803324932473,0.0111470006771207,
-0.00955168810886531));
#37632=CARTESIAN_POINT('Ctrl Pts',(-0.208037463576997,0.0111876777420301,
-0.00953413158364634));
#37633=CARTESIAN_POINT('Ctrl Pts',(-0.208040553165688,0.0112154809968615,
-0.00952188389873837));
#37634=CARTESIAN_POINT('Ctrl Pts',(-0.20804438099605,0.0112489841224429,
-0.0095069446265188));
#37635=CARTESIAN_POINT('Ctrl Pts',(-0.208048208826411,0.0112824872480244,
-0.00949200535429924));
#37636=CARTESIAN_POINT('Ctrl Pts',(-0.208052776893594,0.0113216485495595,
-0.00947428265767254));
#37637=CARTESIAN_POINT('Ctrl Pts',(-0.20805763091643,0.011361898207728,
-0.00945568176171258));
#37638=CARTESIAN_POINT('Ctrl Pts',(-0.208067338962103,0.011442397524065,
-0.00941847996979267));
#37639=CARTESIAN_POINT('Ctrl Pts',(-0.208078188322781,0.0115273059902323,
-0.00937788080676488));
#37640=CARTESIAN_POINT('Ctrl Pts',(-0.208090526205669,0.0116195439206632,
-0.00933172437706195));
#37641=CARTESIAN_POINT('Ctrl Pts',(-0.208115201971445,0.0118040197815248,
-0.0092394115176561));
#37642=CARTESIAN_POINT('Ctrl Pts',(-0.208145833538144,0.0120177654804916,
-0.00912479078211141));
#37643=CARTESIAN_POINT('Ctrl Pts',(-0.208182230285086,0.0122530779316807,
-0.00898281412196308));
#37644=CARTESIAN_POINT('Ctrl Pts',(-0.208182276449934,0.0122530856411887,
-0.00898281044739297));
#37645=CARTESIAN_POINT('Ctrl Pts',(-0.207850571746568,0.0122531164075521,
-0.00897558571096322));
#37646=CARTESIAN_POINT('Ctrl Pts',(-0.207517024495258,0.0122531509908904,
-0.00896831863032881));
#37647=CARTESIAN_POINT('Ctrl Pts',(-0.207182088327276,0.0122531894495252,
-0.00896101902474837));
#37648=CARTESIAN_POINT('Origin',(-0.209569677721342,0.00750000034173499,
-0.00120784314777216));
#37649=CARTESIAN_POINT('',(-0.209182495727072,0.0122512742386181,-0.00900210870397552));
#37650=CARTESIAN_POINT('',(-0.209097173656828,0.00749996683895177,-0.0103336053779799));
#37651=CARTESIAN_POINT('Ctrl Pts',(-0.209182495727072,0.0122512742386181,
-0.00900210870397552));
#37652=CARTESIAN_POINT('Ctrl Pts',(-0.209146116898134,0.0120162484633245,
-0.0091444993018481));
#37653=CARTESIAN_POINT('Ctrl Pts',(-0.209115485562962,0.0118027042814943,
-0.00925946898166217));
#37654=CARTESIAN_POINT('Ctrl Pts',(-0.209090795759128,0.0116183929515475,
-0.0093520603329931));
#37655=CARTESIAN_POINT('Ctrl Pts',(-0.209078450857211,0.0115262372865741,
-0.00939835600865857));
#37656=CARTESIAN_POINT('Ctrl Pts',(-0.209067590900416,0.0114414021296796,
-0.00943907723696154));
#37657=CARTESIAN_POINT('Ctrl Pts',(-0.209057864907749,0.0113609473140376,
-0.00947640086291531));
#37658=CARTESIAN_POINT('Ctrl Pts',(-0.209053001911415,0.0113207199062166,
-0.00949506267589219));
#37659=CARTESIAN_POINT('Ctrl Pts',(-0.209048423039397,0.0112815734658911,
-0.00951284595782519));
#37660=CARTESIAN_POINT('Ctrl Pts',(-0.209044587689804,0.0112481086307926,
-0.00952782476656639));
#37661=CARTESIAN_POINT('Ctrl Pts',(-0.209040752340212,0.0112146437956942,
-0.00954280357530759));
#37662=CARTESIAN_POINT('Ctrl Pts',(-0.209037658496315,0.0111869028464035,
-0.00955507067833089));
#37663=CARTESIAN_POINT('Ctrl Pts',(-0.209033422336463,0.0111461861938047,
-0.00957271035297675));
#37664=CARTESIAN_POINT('Ctrl Pts',(-0.20902918617661,0.011105469541206,
-0.00959035002762261));
#37665=CARTESIAN_POINT('Ctrl Pts',(-0.209023811347096,0.0110517037399591,
-0.00961319454862126));
#37666=CARTESIAN_POINT('Ctrl Pts',(-0.209019091651199,0.01100117207776,
-0.00963406841813438));
#37667=CARTESIAN_POINT('Ctrl Pts',(-0.209014371955302,0.010950640415561,
-0.00965494228764749));
#37668=CARTESIAN_POINT('Ctrl Pts',(-0.209010304834951,0.0109033909435601,
-0.00967396317346768));
#37669=CARTESIAN_POINT('Ctrl Pts',(-0.209006450770597,0.0108554755926814,
-0.00969280968065493));
#37670=CARTESIAN_POINT('Ctrl Pts',(-0.208998742641888,0.010759644890924,
-0.00973050269502944));
#37671=CARTESIAN_POINT('Ctrl Pts',(-0.208991889348806,0.0106611071742381,
-0.00976737806350049));
#37672=CARTESIAN_POINT('Ctrl Pts',(-0.208986238313865,0.0105622377320011,
-0.00980244686196568));
#37673=CARTESIAN_POINT('Ctrl Pts',(-0.208974936243982,0.0103644988475271,
-0.00987258445889605));
#37674=CARTESIAN_POINT('Ctrl Pts',(-0.208968442737192,0.0101654202293464,
-0.0099355173677369));
#37675=CARTESIAN_POINT('Ctrl Pts',(-0.208966088716348,0.00996977678241938,
-0.00999042751774837));
#37676=CARTESIAN_POINT('Ctrl Pts',(-0.208963734695503,0.00977413333549238,
-0.0100453376677598));
#37677=CARTESIAN_POINT('Ctrl Pts',(-0.208965510366025,0.00958206588990063,
-0.0100926755906785));
#37678=CARTESIAN_POINT('Ctrl Pts',(-0.208971084439266,0.00937745137366946,
-0.0101357826877813));
#37679=CARTESIAN_POINT('Ctrl Pts',(-0.208973871475886,0.00927514411555387,
-0.0101573362363327));
#37680=CARTESIAN_POINT('Ctrl Pts',(-0.208977611311151,0.00916966863997126,
-0.0101776849801711));
#37681=CARTESIAN_POINT('Ctrl Pts',(-0.20898213094383,0.00906579616679699,
-0.0101958616298435));
#37682=CARTESIAN_POINT('Ctrl Pts',(-0.208984390760169,0.00901385993020985,
-0.0102049499546797));
#37683=CARTESIAN_POINT('Ctrl Pts',(-0.208986844580244,0.00896233246271355,
-0.010213538751811));
#37684=CARTESIAN_POINT('Ctrl Pts',(-0.208989799995037,0.00890618019447978,
-0.0102223541299263));
#37685=CARTESIAN_POINT('Ctrl Pts',(-0.208992755409829,0.00885002792624601,
-0.0102311695080417));
#37686=CARTESIAN_POINT('Ctrl Pts',(-0.208996215703227,0.00878922659380881,
-0.010240060417762));
#37687=CARTESIAN_POINT('Ctrl Pts',(-0.208998902942324,0.00874408042561425,
-0.0102463272818958));
#37688=CARTESIAN_POINT('Ctrl Pts',(-0.209001590181421,0.00869893425741969,
-0.0102525941460297));
#37689=CARTESIAN_POINT('Ctrl Pts',(-0.209003499782319,0.00866947167989352,
-0.0102564478100287));
#37690=CARTESIAN_POINT('Ctrl Pts',(-0.209005922071796,0.0086332384398221,
-0.010261031993143));
#37691=CARTESIAN_POINT('Ctrl Pts',(-0.209008344361273,0.00859700519975068,
-0.0102656161762573));
#37692=CARTESIAN_POINT('Ctrl Pts',(-0.209011281793522,0.0085539877664341,
-0.0102708179931996));
#37693=CARTESIAN_POINT('Ctrl Pts',(-0.209014420106914,0.00850967487191003,
-0.0102758160109009));
#37694=CARTESIAN_POINT('Ctrl Pts',(-0.209020696733697,0.00842104908286189,
-0.0102858120463034));
#37695=CARTESIAN_POINT('Ctrl Pts',(-0.209027773784346,0.0083272551517127,
-0.0102951355071637));
#37696=CARTESIAN_POINT('Ctrl Pts',(-0.209035898856334,0.00822424368548321,
-0.0103035078611286));
#37697=CARTESIAN_POINT('Ctrl Pts',(-0.209052149000311,0.00801822075302423,
-0.0103202525690584));
#37698=CARTESIAN_POINT('Ctrl Pts',(-0.209072593856506,0.00777532666243376,
-0.0103330720239394));
#37699=CARTESIAN_POINT('Ctrl Pts',(-0.209097173656828,0.00749996683895177,
-0.0103336053779799));
#37700=CARTESIAN_POINT('',(-0.209182613690262,0.00275154001515932,-0.00900382387632688));
#37701=CARTESIAN_POINT('Ctrl Pts',(-0.20909717356973,0.00749996586807601,
-0.0103336053760826));
#37702=CARTESIAN_POINT('Ctrl Pts',(-0.209072489707309,0.00722481928663946,
-0.01033306766277));
#37703=CARTESIAN_POINT('Ctrl Pts',(-0.20904171049841,0.00686077358303126,
-0.0103137662843188));
#37704=CARTESIAN_POINT('Ctrl Pts',(-0.209016873870949,0.00653266430565598,
-0.010281293384316));
#37705=CARTESIAN_POINT('Ctrl Pts',(-0.209005115616393,0.00636077619910354,
-0.0102604255694866));
#37706=CARTESIAN_POINT('Ctrl Pts',(-0.208999372618018,0.00627224778053745,
-0.0102489323528682));
#37707=CARTESIAN_POINT('Ctrl Pts',(-0.208989045745688,0.0060906225411391,
-0.0102224377908441));
#37708=CARTESIAN_POINT('Ctrl Pts',(-0.208979290894002,0.00588500517489839,
-0.0101881039000263));
#37709=CARTESIAN_POINT('Ctrl Pts',(-0.208966327046493,0.00551658091107566,
-0.0101171362638947));
#37710=CARTESIAN_POINT('Ctrl Pts',(-0.208962151603096,0.00503451819218248,
-0.00999833805250308));
#37711=CARTESIAN_POINT('Ctrl Pts',(-0.208978587062817,0.00453890814300135,
-0.00984222924809274));
#37712=CARTESIAN_POINT('Ctrl Pts',(-0.209002677049482,0.00419387918757995,
-0.00971306850389939));
#37713=CARTESIAN_POINT('Ctrl Pts',(-0.209018982861624,0.00400468657447842,
-0.0096370935893603));
#37714=CARTESIAN_POINT('Ctrl Pts',(-0.209035148855368,0.0038430099342979,
-0.00956840324924233));
#37715=CARTESIAN_POINT('Ctrl Pts',(-0.209044401153986,0.00376000689156962,
-0.00953165274028389));
#37716=CARTESIAN_POINT('Ctrl Pts',(-0.209062680278958,0.00360343910340024,
-0.00946067603908059));
#37717=CARTESIAN_POINT('Ctrl Pts',(-0.209100582810176,0.00330674321880253,
-0.00931824322218647));
#37718=CARTESIAN_POINT('Ctrl Pts',(-0.209146370547163,0.00298649792918081,
-0.00914605984684738));
#37719=CARTESIAN_POINT('Ctrl Pts',(-0.209182613690262,0.00275154001515932,
-0.00900382387632688));
#37720=CARTESIAN_POINT('',(-0.210183371239666,0.00275146176851279,-0.00902553543512514));
#37721=CARTESIAN_POINT('Ctrl Pts',(-0.209182669503787,0.00275154408037991,
-0.00900382756445142));
#37722=CARTESIAN_POINT('Ctrl Pts',(-0.209514380222137,0.00275151621947163,
-0.00901102289771852));
#37723=CARTESIAN_POINT('Ctrl Pts',(-0.209848122110046,0.00275148453891749,
-0.00901826006884851));
#37724=CARTESIAN_POINT('Ctrl Pts',(-0.21018341152138,0.00275144896457034,
-0.00902552851673686));
#37725=CARTESIAN_POINT('',(-0.210096846436932,0.00749994274414048,-0.0103553392159764));
#37726=CARTESIAN_POINT('Ctrl Pts',(-0.210183371239666,0.00275146176851279,
-0.00902553543512514));
#37727=CARTESIAN_POINT('Ctrl Pts',(-0.210146994593344,0.0029873235141714,
-0.00916832180670742));
#37728=CARTESIAN_POINT('Ctrl Pts',(-0.210116353263695,0.00320164542671377,
-0.00928356921553769));
#37729=CARTESIAN_POINT('Ctrl Pts',(-0.210091638158358,0.00338667278164948,
-0.0093763774552128));
#37730=CARTESIAN_POINT('Ctrl Pts',(-0.21007928060569,0.00347918645911733,
-0.00942278157505036));
#37731=CARTESIAN_POINT('Ctrl Pts',(-0.210068404179204,0.00356436440277715,
-0.00946359567450267));
#37732=CARTESIAN_POINT('Ctrl Pts',(-0.21005865995935,0.00364512021905286,
-0.00950098725273489));
#37733=CARTESIAN_POINT('Ctrl Pts',(-0.210053787849423,0.00368549812719071,
-0.00951968304185099));
#37734=CARTESIAN_POINT('Ctrl Pts',(-0.210049199422547,0.00372478455364116,
-0.00953749416088998));
#37735=CARTESIAN_POINT('Ctrl Pts',(-0.21004535108913,0.00375841244086312,
-0.00955251441648829));
#37736=CARTESIAN_POINT('Ctrl Pts',(-0.210041502755713,0.00379204032808509,
-0.00956753467208659));
#37737=CARTESIAN_POINT('Ctrl Pts',(-0.210038392506187,0.00381996763616456,
-0.00957985649103939));
#37738=CARTESIAN_POINT('Ctrl Pts',(-0.210034148670161,0.00386075504915408,
-0.00959748660077347));
#37739=CARTESIAN_POINT('Ctrl Pts',(-0.210029904834134,0.00390154246214361,
-0.00961511671050755));
#37740=CARTESIAN_POINT('Ctrl Pts',(-0.210024531039477,0.00395526288300835,
-0.00963788825278974));
#37741=CARTESIAN_POINT('Ctrl Pts',(-0.210019806380593,0.0040057336415685,
-0.00965868830426901));
#37742=CARTESIAN_POINT('Ctrl Pts',(-0.210015081721709,0.00405620440012864,
-0.00967948835574828));
#37743=CARTESIAN_POINT('Ctrl Pts',(-0.210011003655277,0.00410337781766793,
-0.0096984338930203));
#37744=CARTESIAN_POINT('Ctrl Pts',(-0.21000713624919,0.00415119528734392,
-0.0097171980344378));
#37745=CARTESIAN_POINT('Ctrl Pts',(-0.209999401437016,0.0042468302266959,
-0.0097547263172728));
#37746=CARTESIAN_POINT('Ctrl Pts',(-0.209992511923845,0.00434508601214227,
-0.00979140678221356));
#37747=CARTESIAN_POINT('Ctrl Pts',(-0.209986811465036,0.00444335069677145,
-0.00982618735090269));
#37748=CARTESIAN_POINT('Ctrl Pts',(-0.209975410547418,0.0046398800660298,
-0.00989574848828094));
#37749=CARTESIAN_POINT('Ctrl Pts',(-0.209968763765471,0.00483642846725269,
-0.00995780579218629));
#37750=CARTESIAN_POINT('Ctrl Pts',(-0.209966215642179,0.00503111252250329,
-0.0100124209606021));
#37751=CARTESIAN_POINT('Ctrl Pts',(-0.209963667518888,0.0052257965777539,
-0.0100670361290179));
#37752=CARTESIAN_POINT('Ctrl Pts',(-0.209965211079014,0.00541851214447677,
-0.0101145299821102));
#37753=CARTESIAN_POINT('Ctrl Pts',(-0.209970565738309,0.00562248776116485,
-0.0101574995487602));
#37754=CARTESIAN_POINT('Ctrl Pts',(-0.209973243067956,0.00572447556950889,
-0.0101789843320852));
#37755=CARTESIAN_POINT('Ctrl Pts',(-0.209976875917157,0.00582930603355706,
-0.0101992117990275));
#37756=CARTESIAN_POINT('Ctrl Pts',(-0.20998129401994,0.00593255289743084,
-0.0102172968845377));
#37757=CARTESIAN_POINT('Ctrl Pts',(-0.209983503071332,0.00598417632936772,
-0.0102263394272928));
#37758=CARTESIAN_POINT('Ctrl Pts',(-0.209985907538537,0.00603539616134188,
-0.0102348876589781));
#37759=CARTESIAN_POINT('Ctrl Pts',(-0.209988804349278,0.006091090092447,
-0.0102436475952405));
#37760=CARTESIAN_POINT('Ctrl Pts',(-0.20999170116002,0.00614678402355212,
-0.0102524075315029));
#37761=CARTESIAN_POINT('Ctrl Pts',(-0.209995093480332,0.00620697551148496,
-0.0102612335501065));
#37762=CARTESIAN_POINT('Ctrl Pts',(-0.2099977485288,0.00625192088319922,
-0.0102674923467883));
#37763=CARTESIAN_POINT('Ctrl Pts',(-0.210000403577268,0.00629686625491348,
-0.0102737511434701));
#37764=CARTESIAN_POINT('Ctrl Pts',(-0.210002316904279,0.00632653780075192,
-0.0102776473796006));
#37765=CARTESIAN_POINT('Ctrl Pts',(-0.210004741283944,0.00636289412582311,
-0.0102822627645651));
#37766=CARTESIAN_POINT('Ctrl Pts',(-0.210007165663609,0.00639925045089429,
-0.0102868781495297));
#37767=CARTESIAN_POINT('Ctrl Pts',(-0.21001010349879,0.00644230485879222,
-0.0102921021626682));
#37768=CARTESIAN_POINT('Ctrl Pts',(-0.210013249753823,0.00648669002716698,
-0.0102971263935411));
#37769=CARTESIAN_POINT('Ctrl Pts',(-0.210019542263891,0.00657546036391651,
-0.0103071748552868));
#37770=CARTESIAN_POINT('Ctrl Pts',(-0.21002666540856,0.00666954022906901,
-0.0103165642357206));
#37771=CARTESIAN_POINT('Ctrl Pts',(-0.210034860263665,0.00677289174688065,
-0.0103249978927266));
#37772=CARTESIAN_POINT('Ctrl Pts',(-0.210051249973874,0.00697959478250394,
-0.0103418652067386));
#37773=CARTESIAN_POINT('Ctrl Pts',(-0.210071929000393,0.00722338510027445,
-0.0103547958065898));
#37774=CARTESIAN_POINT('Ctrl Pts',(-0.210096846437032,0.00749994274413152,
-0.0103553392159786));
#37775=CARTESIAN_POINT('',(-0.210182952559,0.0122509750948127,-0.0090240400549463));
#37776=CARTESIAN_POINT('Ctrl Pts',(-0.210096846436932,0.00749994274414048,
-0.0103553392159764));
#37777=CARTESIAN_POINT('Ctrl Pts',(-0.210096421573129,0.00750467804303478,
-0.0103553300078083));
#37778=CARTESIAN_POINT('Ctrl Pts',(-0.210094091070512,0.00753069899736505,
-0.0103552503224888));
#37779=CARTESIAN_POINT('Ctrl Pts',(-0.210092277287072,0.00755102334106925,
-0.0103550973215045));
#37780=CARTESIAN_POINT('Ctrl Pts',(-0.210090463503631,0.00757134768477346,
-0.0103549443205201));
#37781=CARTESIAN_POINT('Ctrl Pts',(-0.210089165078757,0.00758597569404241,
-0.0103547805867168));
#37782=CARTESIAN_POINT('Ctrl Pts',(-0.210087794381028,0.00760145938077238,
-0.0103545787390152));
#37783=CARTESIAN_POINT('Ctrl Pts',(-0.210085052985569,0.00763242675423232,
-0.0103541750436119));
#37784=CARTESIAN_POINT('Ctrl Pts',(-0.210082023924896,0.00766681588579745,
-0.0103535532925314));
#37785=CARTESIAN_POINT('Ctrl Pts',(-0.210079125509802,0.00769995376384079,
-0.0103527644907727));
#37786=CARTESIAN_POINT('Ctrl Pts',(-0.210073328679614,0.00776622951992748,
-0.0103511868872554));
#37787=CARTESIAN_POINT('Ctrl Pts',(-0.21006805238263,0.00782750311150865,
-0.0103490353326892));
#37788=CARTESIAN_POINT('Ctrl Pts',(-0.210062967839213,0.00788740023130505,
-0.010346381440422));
#37789=CARTESIAN_POINT('Ctrl Pts',(-0.210057883295797,0.00794729735110145,
-0.0103437275481549));
#37790=CARTESIAN_POINT('Ctrl Pts',(-0.210052991179761,0.00800581599859524,
-0.0103405403250739));
#37791=CARTESIAN_POINT('Ctrl Pts',(-0.210048369589446,0.00806208143919039,
-0.0103369699750641));
#37792=CARTESIAN_POINT('Ctrl Pts',(-0.210043747999131,0.00811834687978555,
-0.0103333996250543));
#37793=CARTESIAN_POINT('Ctrl Pts',(-0.210039396828702,0.00817235991846103,
-0.0103294510161944));
#37794=CARTESIAN_POINT('Ctrl Pts',(-0.210035314943403,0.00822397052514526,
-0.0103252576166531));
#37795=CARTESIAN_POINT('Ctrl Pts',(-0.210027151172807,0.00832719173851372,
-0.0103168708175704));
#37796=CARTESIAN_POINT('Ctrl Pts',(-0.210020063277611,0.00842080552037382,
-0.0103075630469351));
#37797=CARTESIAN_POINT('Ctrl Pts',(-0.210013778935997,0.00850937355036198,
-0.0102975762177072));
#37798=CARTESIAN_POINT('Ctrl Pts',(-0.21001063676519,0.00855365756535605,
-0.0102925828030932));
#37799=CARTESIAN_POINT('Ctrl Pts',(-0.210007696289592,0.00859667666147962,
-0.0102873825130392));
#37800=CARTESIAN_POINT('Ctrl Pts',(-0.210005271703267,0.00863292877725493,
-0.0102827971657773));
#37801=CARTESIAN_POINT('Ctrl Pts',(-0.210002847116943,0.00866918089303023,
-0.0102782118185155));
#37802=CARTESIAN_POINT('Ctrl Pts',(-0.210000935973877,0.0086986795055452,
-0.0102743539231139));
#37803=CARTESIAN_POINT('Ctrl Pts',(-0.209998256336171,0.00874376620306087,
-0.0102680969834612));
#37804=CARTESIAN_POINT('Ctrl Pts',(-0.209995576698465,0.00878885290057654,
-0.0102618400438085));
#37805=CARTESIAN_POINT('Ctrl Pts',(-0.209992133114742,0.00884949947558208,
-0.010252974837074));
#37806=CARTESIAN_POINT('Ctrl Pts',(-0.209989192135327,0.00890555230308399,
-0.010244179247103));
#37807=CARTESIAN_POINT('Ctrl Pts',(-0.209986251155911,0.0089616051305859,
-0.010235383657132));
#37808=CARTESIAN_POINT('Ctrl Pts',(-0.209983809530347,0.00901308822745524,
-0.0102268071956456));
#37809=CARTESIAN_POINT('Ctrl Pts',(-0.209981563015109,0.00906497838414453,
-0.0102177320221761));
#37810=CARTESIAN_POINT('Ctrl Pts',(-0.209977069984633,0.0091687586975231,
-0.0101995816752372));
#37811=CARTESIAN_POINT('Ctrl Pts',(-0.209973361104316,0.0092741356329341,
-0.0101792658831118));
#37812=CARTESIAN_POINT('Ctrl Pts',(-0.209970608023758,0.00937649422666917,
-0.0101577136994801));
#37813=CARTESIAN_POINT('Ctrl Pts',(-0.209965101862643,0.0095812114141393,
-0.0101146093322166));
#37814=CARTESIAN_POINT('Ctrl Pts',(-0.209963406965898,0.00977397402149797,
-0.0100671083632951));
#37815=CARTESIAN_POINT('Ctrl Pts',(-0.209965844413768,0.0099694793343208,
-0.0100122458991389));
#37816=CARTESIAN_POINT('Ctrl Pts',(-0.209968281861638,0.0101649846471436,
-0.0099573834349827));
#37817=CARTESIAN_POINT('Ctrl Pts',(-0.209974859957364,0.0103631109907,-0.00989477754227005));
#37818=CARTESIAN_POINT('Ctrl Pts',(-0.209986266187064,0.0105607267647511,
-0.0098247250529686));
#37819=CARTESIAN_POINT('Ctrl Pts',(-0.209991969301913,0.0106595346517767,
-0.00978969880831788));
#37820=CARTESIAN_POINT('Ctrl Pts',(-0.209998879810517,0.0107582137766952,
-0.00975279434377352));
#37821=CARTESIAN_POINT('Ctrl Pts',(-0.210006645172636,0.0108542149694637,
-0.00971505164932369));
#37822=CARTESIAN_POINT('Ctrl Pts',(-0.210010527853695,0.010902215565848,
-0.00969618030209878));
#37823=CARTESIAN_POINT('Ctrl Pts',(-0.21001462357696,0.0109495579232455,
-0.00967713027028166));
#37824=CARTESIAN_POINT('Ctrl Pts',(-0.2100193774721,0.0110002414631578,
-0.00965620063211537));
#37825=CARTESIAN_POINT('Ctrl Pts',(-0.210024131367239,0.0110509250030702,
-0.00963527099394908));
#37826=CARTESIAN_POINT('Ctrl Pts',(-0.210029546028417,0.01110490099765,
-0.00961234242141701));
#37827=CARTESIAN_POINT('Ctrl Pts',(-0.210033805218153,0.0111457179693001,
-0.00959466225771742));
#37828=CARTESIAN_POINT('Ctrl Pts',(-0.210038064407889,0.0111865349409501,
-0.00957698209401783));
#37829=CARTESIAN_POINT('Ctrl Pts',(-0.210041164439004,0.0112142671573592,
-0.00956471994512065));
#37830=CARTESIAN_POINT('Ctrl Pts',(-0.210045008403367,0.0112477443471597,
-0.00954973750983502));
#37831=CARTESIAN_POINT('Ctrl Pts',(-0.21004885236773,0.0112812215369602,
-0.00953475507454939));
#37832=CARTESIAN_POINT('Ctrl Pts',(-0.210053442297848,0.0113204010892225,
-0.00951695885970419));
#37833=CARTESIAN_POINT('Ctrl Pts',(-0.210058314380606,0.0113606536646177,
-0.00949828722445998));
#37834=CARTESIAN_POINT('Ctrl Pts',(-0.210068058546121,0.0114411588154081,
-0.00946094395397156));
#37835=CARTESIAN_POINT('Ctrl Pts',(-0.210078928773307,0.011526012881933,
-0.00942021624837313));
#37836=CARTESIAN_POINT('Ctrl Pts',(-0.210091279231665,0.0116181773530369,
-0.00937391926268402));
#37837=CARTESIAN_POINT('Ctrl Pts',(-0.21011598014838,0.0118025062952446,
-0.0092813252913058));
#37838=CARTESIAN_POINT('Ctrl Pts',(-0.210146603778555,0.0120160267225188,
-0.00916637191627331));
#37839=CARTESIAN_POINT('Ctrl Pts',(-0.210182952559,0.0122509750948127,-0.0090240400549463));
#37840=CARTESIAN_POINT('Ctrl Pts',(-0.210182993958729,0.0122509825883683,
-0.00902403639013458));
#37841=CARTESIAN_POINT('Ctrl Pts',(-0.209849556732748,0.012251076389419,
-0.00901673059642433));
#37842=CARTESIAN_POINT('Ctrl Pts',(-0.209516008085114,0.012251173766512,
-0.00900942019982785));
#37843=CARTESIAN_POINT('Ctrl Pts',(-0.209182556323231,0.0122512746577035,
-0.00900210976597304));
#37844=CARTESIAN_POINT('Origin',(-0.193568907911486,0.00750000067102937,
-0.00057655143392958));
#37845=CARTESIAN_POINT('',(-0.193177238558164,0.0122676067884443,-0.00867531668264591));
#37846=CARTESIAN_POINT('',(-0.193103863223514,0.00750326208931829,-0.00997223504951149));
#37847=CARTESIAN_POINT('Ctrl Pts',(-0.193177238558164,0.0122676067884443,
-0.00867531668264591));
#37848=CARTESIAN_POINT('Ctrl Pts',(-0.193141277408561,0.0120297062798438,
-0.00881450643419947));
#37849=CARTESIAN_POINT('Ctrl Pts',(-0.193096702853472,0.0117128138412265,
-0.00898007212936678));
#37850=CARTESIAN_POINT('Ctrl Pts',(-0.193053007151483,0.0113544430299681,
-0.00914564853116907));
#37851=CARTESIAN_POINT('Ctrl Pts',(-0.193033159712931,0.011177123403759,
-0.00922315221236596));
#37852=CARTESIAN_POINT('Ctrl Pts',(-0.193005590632074,0.0108636784687834,
-0.00934989089102075));
#37853=CARTESIAN_POINT('Ctrl Pts',(-0.192982407950007,0.0104851086177235,
-0.00948721987317339));
#37854=CARTESIAN_POINT('Ctrl Pts',(-0.192968408173786,0.00996069993436876,
-0.00964846359291627));
#37855=CARTESIAN_POINT('Ctrl Pts',(-0.192975189033209,0.00950003337125401,
-0.00975833993598715));
#37856=CARTESIAN_POINT('Ctrl Pts',(-0.192989252673654,0.00912702910240768,
-0.00982891691881178));
#37857=CARTESIAN_POINT('Ctrl Pts',(-0.19299947871711,0.00891840860987315,
-0.00986296989761181));
#37858=CARTESIAN_POINT('Ctrl Pts',(-0.193010186783734,0.00873159276027399,
-0.00988956309502806));
#37859=CARTESIAN_POINT('Ctrl Pts',(-0.193015853940037,0.00864328838181661,
-0.00990071154504017));
#37860=CARTESIAN_POINT('Ctrl Pts',(-0.193027433931117,0.00847013191613375,
-0.0099211982004547));
#37861=CARTESIAN_POINT('Ctrl Pts',(-0.193051412520838,0.00814133853363067,
-0.0099528640409497));
#37862=CARTESIAN_POINT('Ctrl Pts',(-0.193080619914893,0.00777761606572264,
-0.00997163740758629));
#37863=CARTESIAN_POINT('Ctrl Pts',(-0.193103863741755,0.00750326261887232,
-0.00997223506269818));
#37864=CARTESIAN_POINT('',(-0.193178837423798,0.00273574495468982,-0.0086773204769601));
#37865=CARTESIAN_POINT('Ctrl Pts',(-0.193103863693919,0.0075032620497559,
-0.00997223506186141));
#37866=CARTESIAN_POINT('Ctrl Pts',(-0.193101982070691,0.00748087649952758,
-0.00997220214559293));
#37867=CARTESIAN_POINT('Ctrl Pts',(-0.193094992227577,0.0073973397143487,
-0.00997171707917436));
#37868=CARTESIAN_POINT('Ctrl Pts',(-0.193084786939789,0.00727362393760784,
-0.00996941923967326));
#37869=CARTESIAN_POINT('Ctrl Pts',(-0.193066650048077,0.00704999053098598,
-0.00996215274241276));
#37870=CARTESIAN_POINT('Ctrl Pts',(-0.193045003613772,0.00677035458551498,
-0.00994422576682089));
#37871=CARTESIAN_POINT('Ctrl Pts',(-0.193027940246176,0.00653410165293154,
-0.00992165651782325));
#37872=CARTESIAN_POINT('Ctrl Pts',(-0.193016479642015,0.00636065866460942,
-0.00990121037081368));
#37873=CARTESIAN_POINT('Ctrl Pts',(-0.193010824022097,0.00627131283022669,
-0.00988995406090102));
#37874=CARTESIAN_POINT('Ctrl Pts',(-0.193000398980532,0.00608661552070766,
-0.00986374663195098));
#37875=CARTESIAN_POINT('Ctrl Pts',(-0.192990329008554,0.00587750923105183,
-0.00982974235804112));
#37876=CARTESIAN_POINT('Ctrl Pts',(-0.192976630034204,0.00550500463892925,
-0.00975946406604019));
#37877=CARTESIAN_POINT('Ctrl Pts',(-0.192970301148135,0.00504236762906688,
-0.00964933948491919));
#37878=CARTESIAN_POINT('Ctrl Pts',(-0.192984713678361,0.00451957126348969,
-0.009488820974985));
#37879=CARTESIAN_POINT('Ctrl Pts',(-0.193008070991626,0.00414029891002481,
-0.00935148376040879));
#37880=CARTESIAN_POINT('Ctrl Pts',(-0.193035766744627,0.00382550828794464,
-0.00922433195482671));
#37881=CARTESIAN_POINT('Ctrl Pts',(-0.193055511987502,0.00364845234953881,
-0.00914699638297536));
#37882=CARTESIAN_POINT('Ctrl Pts',(-0.193098939509399,0.00329032861337595,
-0.00898168634553191));
#37883=CARTESIAN_POINT('Ctrl Pts',(-0.19314316987124,0.00297358087421801,
-0.00881634617994497));
#37884=CARTESIAN_POINT('Ctrl Pts',(-0.193178837423798,0.00273574495468982,
-0.0086773204769601));
#37885=CARTESIAN_POINT('',(-0.194178126336983,0.00273578034803723,-0.00869894669169024));
#37886=CARTESIAN_POINT('Ctrl Pts',(-0.193178923166509,0.00273574786287452,
-0.00867732404017732));
#37887=CARTESIAN_POINT('Ctrl Pts',(-0.193516558232873,0.00273575905641843,
-0.00868463055489243));
#37888=CARTESIAN_POINT('Ctrl Pts',(-0.19384994814426,0.00273576515675357,
-0.00869184229227085));
#37889=CARTESIAN_POINT('Ctrl Pts',(-0.194178193748642,0.00273576655198442,
-0.00869894004011713));
#37890=CARTESIAN_POINT('',(-0.194103296318277,0.00750354445494538,-0.00999384110469418));
#37891=CARTESIAN_POINT('Ctrl Pts',(-0.194178126336983,0.00273578034803723,
-0.00869894669169024));
#37892=CARTESIAN_POINT('Ctrl Pts',(-0.194142042098836,0.00297492111932904,
-0.00883872879554135));
#37893=CARTESIAN_POINT('Ctrl Pts',(-0.194097326545317,0.00329355354970724,
-0.00900492219595842));
#37894=CARTESIAN_POINT('Ctrl Pts',(-0.194053576967989,0.00365337062553203,
-0.00917080388678816));
#37895=CARTESIAN_POINT('Ctrl Pts',(-0.194033651716486,0.00383231370014839,
-0.00924877799144863));
#37896=CARTESIAN_POINT('Ctrl Pts',(-0.194006380571071,0.0041439301034018,
-0.00937441384127908));
#37897=CARTESIAN_POINT('Ctrl Pts',(-0.193983325356653,0.0045212416713753,
-0.00951094738593517));
#37898=CARTESIAN_POINT('Ctrl Pts',(-0.193969309601735,0.00504288807939639,
-0.0096710240379633));
#37899=CARTESIAN_POINT('Ctrl Pts',(-0.193975851273483,0.00550315434166333,
-0.0097806464712603));
#37900=CARTESIAN_POINT('Ctrl Pts',(-0.193989630863608,0.00587518475769505,
-0.00985093422918167));
#37901=CARTESIAN_POINT('Ctrl Pts',(-0.193999709756721,0.00608390961146259,
-0.00988494053456836));
#37902=CARTESIAN_POINT('Ctrl Pts',(-0.194010169566569,0.00626911514536853,
-0.00991126905619667));
#37903=CARTESIAN_POINT('Ctrl Pts',(-0.194015815544633,0.00635836535611191,
-0.00992254085629852));
#37904=CARTESIAN_POINT('Ctrl Pts',(-0.194027313474826,0.00653237287800241,
-0.00994305673262293));
#37905=CARTESIAN_POINT('Ctrl Pts',(-0.194044176847623,0.00676648600438274,
-0.00996570757859934));
#37906=CARTESIAN_POINT('Ctrl Pts',(-0.194071045174016,0.0071131119218024,
-0.00998731884686608));
#37907=CARTESIAN_POINT('Ctrl Pts',(-0.194090771216625,0.00735428354209366,
-0.0099936266379733));
#37908=CARTESIAN_POINT('Ctrl Pts',(-0.194103296319129,0.00750354416285038,
-0.0099938411048228));
#37909=CARTESIAN_POINT('',(-0.194177646062722,0.0122674896816452,-0.00869701042615392));
#37910=CARTESIAN_POINT('Ctrl Pts',(-0.194103296318277,0.00750354445494538,
-0.00999384110469418));
#37911=CARTESIAN_POINT('Ctrl Pts',(-0.194079958518618,0.00777941560445015,
-0.00999323250307843));
#37912=CARTESIAN_POINT('Ctrl Pts',(-0.194050661160514,0.00814497169210634,
-0.00997425522747218));
#37913=CARTESIAN_POINT('Ctrl Pts',(-0.194026644350104,0.00847534629457309,
-0.00994226043412574));
#37914=CARTESIAN_POINT('Ctrl Pts',(-0.194015080223235,0.00864898723807135,
-0.0099216166364075));
#37915=CARTESIAN_POINT('Ctrl Pts',(-0.194009390838132,0.00873816803744379,
-0.00991028930259834));
#37916=CARTESIAN_POINT('Ctrl Pts',(-0.193998842516715,0.00892342055893506,
-0.00988379830463233));
#37917=CARTESIAN_POINT('Ctrl Pts',(-0.193988741548766,0.00913090327575872,
-0.0098498322196108));
#37918=CARTESIAN_POINT('Ctrl Pts',(-0.193974878568344,0.00950167412757212,
-0.00977954635796348));
#37919=CARTESIAN_POINT('Ctrl Pts',(-0.193968222648747,0.00996018041429022,
-0.0096701523381651));
#37920=CARTESIAN_POINT('Ctrl Pts',(-0.193982176036166,0.0104821187883598,
-0.00950980282130545));
#37921=CARTESIAN_POINT('Ctrl Pts',(-0.194005272373616,0.010859398120637,
-0.00937311789949069));
#37922=CARTESIAN_POINT('Ctrl Pts',(-0.194032635572663,0.0111712397791765,
-0.00924724964660917));
#37923=CARTESIAN_POINT('Ctrl Pts',(-0.194052607422482,0.0113499762585385,
-0.00916927820776025));
#37924=CARTESIAN_POINT('Ctrl Pts',(-0.19409651347767,0.0117097359836059,
-0.00900325799596129));
#37925=CARTESIAN_POINT('Ctrl Pts',(-0.194141409034745,0.0120283418044791,
-0.00883692360353074));
#37926=CARTESIAN_POINT('Ctrl Pts',(-0.194177646062722,0.0122674896816452,
-0.00869701042615392));
#37927=CARTESIAN_POINT('Ctrl Pts',(-0.194177713311809,0.0122674988402921,
-0.0086970064915523));
#37928=CARTESIAN_POINT('Ctrl Pts',(-0.19384633828666,0.0122675305238753,
-0.00868982483646655));
#37929=CARTESIAN_POINT('Ctrl Pts',(-0.193512706876837,0.0122675670396735,
-0.00868259156414702));
#37930=CARTESIAN_POINT('Ctrl Pts',(-0.19317732938957,0.0122676084977587,
-0.00867531764039759));
#37931=CARTESIAN_POINT('Origin',(-0.213568579064389,0.00750000008594914,
-0.00135799511692069));
#37932=CARTESIAN_POINT('',(-0.21318423872705,0.0122469018747551,-0.00908490848644239));
#37933=CARTESIAN_POINT('',(-0.213095878685918,0.0075001804210207,-0.0104239546847203));
#37934=CARTESIAN_POINT('Ctrl Pts',(-0.21318423872705,0.0122469018747551,
-0.00908490848644239));
#37935=CARTESIAN_POINT('Ctrl Pts',(-0.213147967165249,0.0120126167213431,
-0.00922796055956868));
#37936=CARTESIAN_POINT('Ctrl Pts',(-0.213102062381918,0.0116929446600027,
-0.00940128351253897));
#37937=CARTESIAN_POINT('Ctrl Pts',(-0.213063926861882,0.0113964705502375,
-0.00954476979033539));
#37938=CARTESIAN_POINT('Ctrl Pts',(-0.213045448068908,0.0112396752196826,
-0.00961640605766646));
#37939=CARTESIAN_POINT('Ctrl Pts',(-0.213036119558812,0.0111569823392515,
-0.00965331518855872));
#37940=CARTESIAN_POINT('Ctrl Pts',(-0.213019513778469,0.0109934185748677,
-0.00972332629864973));
#37941=CARTESIAN_POINT('Ctrl Pts',(-0.213002795866849,0.0108031199259663,
-0.00980026058746646));
#37942=CARTESIAN_POINT('Ctrl Pts',(-0.212978010642917,0.0104566789835727,
-0.00993070195934068));
#37943=CARTESIAN_POINT('Ctrl Pts',(-0.212960929508415,0.00996624908753319,
-0.0100861135776349));
#37944=CARTESIAN_POINT('Ctrl Pts',(-0.212964587887053,0.00948339356377618,
-0.0102060491687593));
#37945=CARTESIAN_POINT('Ctrl Pts',(-0.212977231013709,0.00911548248511972,
-0.0102773844664645));
#37946=CARTESIAN_POINT('Ctrl Pts',(-0.2129868244226,0.00891006572109696,
-0.0103119301614037));
#37947=CARTESIAN_POINT('Ctrl Pts',(-0.212997018810102,0.00872854262977365,
-0.0103385981982886));
#37948=CARTESIAN_POINT('Ctrl Pts',(-0.213002708045327,0.00864034456961565,
-0.0103501327288066));
#37949=CARTESIAN_POINT('Ctrl Pts',(-0.213014457625488,0.00846865341581425,
-0.0103711386036274));
#37950=CARTESIAN_POINT('Ctrl Pts',(-0.21303947209247,0.0081405967091976,
-0.010403876123959));
#37951=CARTESIAN_POINT('Ctrl Pts',(-0.213070728457374,0.00777597269410619,
-0.0104234017023197));
#37952=CARTESIAN_POINT('Ctrl Pts',(-0.213095878685918,0.0075001804210207,
-0.0104239546847203));
#37953=CARTESIAN_POINT('',(-0.213185703211844,0.00275392014951917,-0.00908544467358939));
#37954=CARTESIAN_POINT('Ctrl Pts',(-0.213095878574979,0.0075001792078503,
-0.0104239546823292));
#37955=CARTESIAN_POINT('Ctrl Pts',(-0.213084624510229,0.00737722579854172,
-0.0104237121079522));
#37956=CARTESIAN_POINT('Ctrl Pts',(-0.213059646951704,0.00709723705871821,
-0.0104169601546021));
#37957=CARTESIAN_POINT('Ctrl Pts',(-0.213032355596658,0.006768339907401,
-0.0103945895617497));
#37958=CARTESIAN_POINT('Ctrl Pts',(-0.21301431087388,0.00653229766580737,
-0.0103712596161075));
#37959=CARTESIAN_POINT('Ctrl Pts',(-0.213002612318022,0.00636096639451181,
-0.0103502918217071));
#37960=CARTESIAN_POINT('Ctrl Pts',(-0.212996932214088,0.00627263427303648,
-0.0103387567924699));
#37961=CARTESIAN_POINT('Ctrl Pts',(-0.212986831556077,0.00609159909993886,
-0.0103121897259374));
#37962=CARTESIAN_POINT('Ctrl Pts',(-0.212977345692435,0.00588625226984478,
-0.0102776983880172));
#37963=CARTESIAN_POINT('Ctrl Pts',(-0.212964932877339,0.00551839699631466,
-0.0102064879064028));
#37964=CARTESIAN_POINT('Ctrl Pts',(-0.212961764061948,0.00503181826712215,
-0.010085595298052));
#37965=CARTESIAN_POINT('Ctrl Pts',(-0.212979242888073,0.00454450835103741,
-0.00993110843775244));
#37966=CARTESIAN_POINT('Ctrl Pts',(-0.213004229563994,0.00419793570972472,
-0.00980070684540739));
#37967=CARTESIAN_POINT('Ctrl Pts',(-0.213021037741107,0.00400755810154577,
-0.00972376773155705));
#37968=CARTESIAN_POINT('Ctrl Pts',(-0.213037718032556,0.00384368614291747,
-0.00965364519619393));
#37969=CARTESIAN_POINT('Ctrl Pts',(-0.213047047347857,0.00376108604420927,
-0.00961678428468142));
#37970=CARTESIAN_POINT('Ctrl Pts',(-0.21306553657481,0.00360429517525143,
-0.00954516870914107));
#37971=CARTESIAN_POINT('Ctrl Pts',(-0.213103652569734,0.00330787216258413,
-0.00940174125825834));
#37972=CARTESIAN_POINT('Ctrl Pts',(-0.213149495293687,0.00298820619271435,
-0.00922846437602459));
#37973=CARTESIAN_POINT('Ctrl Pts',(-0.213185703211844,0.00275392014951917,
-0.00908544467358939));
#37974=CARTESIAN_POINT('',(-0.214186413679644,0.00275332976643362,-0.0091068676959076));
#37975=CARTESIAN_POINT('Ctrl Pts',(-0.213185747109477,0.00275392392937051,
-0.00908544794936231));
#37976=CARTESIAN_POINT('Ctrl Pts',(-0.213519286834764,0.00275372517702273,
-0.00909258710293668));
#37977=CARTESIAN_POINT('Ctrl Pts',(-0.213852922274175,0.00275352290283973,
-0.00909972616793565));
#37978=CARTESIAN_POINT('Ctrl Pts',(-0.214186444847692,0.00275331723326959,
-0.00910686068007963));
#37979=CARTESIAN_POINT('',(-0.214095608114984,0.00750036597474129,-0.0104457182539273));
#37980=CARTESIAN_POINT('Ctrl Pts',(-0.214186413679644,0.00275332976643362,
-0.0091068676959076));
#37981=CARTESIAN_POINT('Ctrl Pts',(-0.214150100837136,0.00298844890012589,
-0.0092504211566524));
#37982=CARTESIAN_POINT('Ctrl Pts',(-0.214119444326417,0.00320233065924093,
-0.00936639784249271));
#37983=CARTESIAN_POINT('Ctrl Pts',(-0.214094651401162,0.00338708449027663,
-0.0094598261305769));
#37984=CARTESIAN_POINT('Ctrl Pts',(-0.214082254938534,0.00347946140579449,
-0.00950654027461899));
#37985=CARTESIAN_POINT('Ctrl Pts',(-0.214071323897576,0.00356454301339925,
-0.00954763912430158));
#37986=CARTESIAN_POINT('Ctrl Pts',(-0.214061493118068,0.00364534081995737,
-0.00958534769706394));
#37987=CARTESIAN_POINT('Ctrl Pts',(-0.214056577728313,0.00368573972323644,
-0.00960420198344512));
#37988=CARTESIAN_POINT('Ctrl Pts',(-0.214051938059047,0.00372508235601198,
-0.00962217860736835));
#37989=CARTESIAN_POINT('Ctrl Pts',(-0.214048052778835,0.00375866104194653,
-0.00963729427663179));
#37990=CARTESIAN_POINT('Ctrl Pts',(-0.214044167498623,0.00379223972788107,
-0.00965240994589524));
#37991=CARTESIAN_POINT('Ctrl Pts',(-0.214041034514651,0.00382001038131348,
-0.00966476079415632));
#37992=CARTESIAN_POINT('Ctrl Pts',(-0.214036691234293,0.00386111054867081,
-0.00968266254234618));
#37993=CARTESIAN_POINT('Ctrl Pts',(-0.214032347953934,0.00390221071602813,
-0.00970056429053603));
#37994=CARTESIAN_POINT('Ctrl Pts',(-0.214026798204625,0.00395671784545832,
-0.00972384112484572));
#37995=CARTESIAN_POINT('Ctrl Pts',(-0.214021921739019,0.0040077473839752,
-0.00974501814468437));
#37996=CARTESIAN_POINT('Ctrl Pts',(-0.214017045273413,0.00405877692249209,
-0.00976619516452301));
#37997=CARTESIAN_POINT('Ctrl Pts',(-0.214012839378027,0.00410627766752427,
-0.00978539701428086));
#37998=CARTESIAN_POINT('Ctrl Pts',(-0.21400884316301,0.00415439357417544,
-0.0098043993375676));
#37999=CARTESIAN_POINT('Ctrl Pts',(-0.214000850732976,0.00425062538747779,
-0.00984240398414109));
#38000=CARTESIAN_POINT('Ctrl Pts',(-0.213993699966926,0.00434936831381604,
-0.00987947535998419));
#38001=CARTESIAN_POINT('Ctrl Pts',(-0.213987755470683,0.00444744652452595,
-0.00991438998611061));
#38002=CARTESIAN_POINT('Ctrl Pts',(-0.213975866478195,0.00464360294594576,
-0.00998421923836345));
#38003=CARTESIAN_POINT('Ctrl Pts',(-0.213968797477862,0.00483703112941228,
-0.0100456551680694));
#38004=CARTESIAN_POINT('Ctrl Pts',(-0.213965833535144,0.00503082262064919,
-0.0101004046276131));
#38005=CARTESIAN_POINT('Ctrl Pts',(-0.213962869592426,0.00522461411188609,
-0.0101551540871568));
#38006=CARTESIAN_POINT('Ctrl Pts',(-0.213964007769243,0.00541871567763622,
-0.0102033520378653));
#38007=CARTESIAN_POINT('Ctrl Pts',(-0.213969011116721,0.00562297644438124,
-0.0102466576087607));
#38008=CARTESIAN_POINT('Ctrl Pts',(-0.21397151279046,0.00572510682775375,
-0.0102683103942083));
#38009=CARTESIAN_POINT('Ctrl Pts',(-0.213974983020484,0.00582980111776385,
-0.0102886361041918));
#38010=CARTESIAN_POINT('Ctrl Pts',(-0.213979254459626,0.00593296549140293,
-0.0103068209009627));
#38011=CARTESIAN_POINT('Ctrl Pts',(-0.213981390179197,0.00598454767822248,
-0.0103159132993481));
#38012=CARTESIAN_POINT('Ctrl Pts',(-0.21398372532838,0.00603573973725164,
-0.0103245105559012));
#38013=CARTESIAN_POINT('Ctrl Pts',(-0.213986547384677,0.00609134377532499,
-0.0103333119158729));
#38014=CARTESIAN_POINT('Ctrl Pts',(-0.213989369440973,0.00614694781339835,
-0.0103421132758447));
#38015=CARTESIAN_POINT('Ctrl Pts',(-0.213992681559152,0.00620698734528899,
-0.010350973822987));
#38016=CARTESIAN_POINT('Ctrl Pts',(-0.213995287493455,0.00625187779379209,
-0.0103572658605673));
#38017=CARTESIAN_POINT('Ctrl Pts',(-0.213997893427757,0.00629676824229519,
-0.0103635578981476));
#38018=CARTESIAN_POINT('Ctrl Pts',(-0.213999788731873,0.00632648178341135,
-0.0103674856704243));
#38019=CARTESIAN_POINT('Ctrl Pts',(-0.214002198062836,0.00636282859077894,
-0.0103721304048202));
#38020=CARTESIAN_POINT('Ctrl Pts',(-0.214004607393799,0.00639917539814654,
-0.0103767751392161));
#38021=CARTESIAN_POINT('Ctrl Pts',(-0.214007533141689,0.00644216866290085,
-0.0103820270457493));
#38022=CARTESIAN_POINT('Ctrl Pts',(-0.214010691369336,0.00648662577075809,
-0.0103870930993818));
#38023=CARTESIAN_POINT('Ctrl Pts',(-0.214017007824629,0.00657553998647256,
-0.0103972252066467));
#38024=CARTESIAN_POINT('Ctrl Pts',(-0.214024251660544,0.0066703007446929,
-0.0104067305057084));
#38025=CARTESIAN_POINT('Ctrl Pts',(-0.214032473075476,0.00677290354355626,
-0.0104151593879221));
#38026=CARTESIAN_POINT('Ctrl Pts',(-0.214040694490407,0.00687550634241962,
-0.0104235882701358));
#38027=CARTESIAN_POINT('Ctrl Pts',(-0.214049891976939,0.0069859388533199,
-0.0104310099796013));
#38028=CARTESIAN_POINT('Ctrl Pts',(-0.214060738298118,0.00711087507504844,
-0.0104366099394931));
#38029=CARTESIAN_POINT('Ctrl Pts',(-0.214071584619298,0.00723581129677699,
-0.0104422098993849));
#38030=CARTESIAN_POINT('Ctrl Pts',(-0.214084090997818,0.00737527186877879,
-0.0104454725859727));
#38031=CARTESIAN_POINT('Ctrl Pts',(-0.214095608115094,0.00750036597473118,
-0.0104457182539297));
#38032=CARTESIAN_POINT('',(-0.214184696860609,0.0122470177333751,-0.00910661628414272));
#38033=CARTESIAN_POINT('Ctrl Pts',(-0.214095608114984,0.00750036597474129,
-0.0104457182539273));
#38034=CARTESIAN_POINT('Ctrl Pts',(-0.214070334864979,0.00777590223793459,
-0.010445156937743));
#38035=CARTESIAN_POINT('Ctrl Pts',(-0.214049409271727,0.00801878429478129,
-0.010432220268336));
#38036=CARTESIAN_POINT('Ctrl Pts',(-0.214032886378828,0.00822460765478433,
-0.0104153680821803));
#38037=CARTESIAN_POINT('Ctrl Pts',(-0.214024624932379,0.00832751933478585,
-0.0104069419891024));
#38038=CARTESIAN_POINT('Ctrl Pts',(-0.214017463510113,0.008421166572945,
-0.0103975669167598));
#38039=CARTESIAN_POINT('Ctrl Pts',(-0.214011156716459,0.00850959622371078,
-0.0103875270045182));
#38040=CARTESIAN_POINT('Ctrl Pts',(-0.214008003319632,0.00855381104909367,
-0.0103825070483974));
#38041=CARTESIAN_POINT('Ctrl Pts',(-0.214005064359136,0.00859671801361874,
-0.0103772850899157));
#38042=CARTESIAN_POINT('Ctrl Pts',(-0.214002650767299,0.00863283383294724,
-0.0103726871256275));
#38043=CARTESIAN_POINT('Ctrl Pts',(-0.214000237175461,0.00866894965227573,
-0.0103680891613394));
#38044=CARTESIAN_POINT('Ctrl Pts',(-0.213998346489832,0.00869828797601001,
-0.0103642283066615));
#38045=CARTESIAN_POINT('Ctrl Pts',(-0.213995701917154,0.00874328117754318,
-0.0103579458563784));
#38046=CARTESIAN_POINT('Ctrl Pts',(-0.213993057344476,0.00878827437907636,
-0.0103516634060952));
#38047=CARTESIAN_POINT('Ctrl Pts',(-0.213989663478094,0.00884889382545365,
-0.0103427483596567));
#38048=CARTESIAN_POINT('Ctrl Pts',(-0.213986772711712,0.00890490784218023,
-0.0103339050625407));
#38049=CARTESIAN_POINT('Ctrl Pts',(-0.21398388194533,0.00896092185890681,
-0.0103250617654246));
#38050=CARTESIAN_POINT('Ctrl Pts',(-0.213981490994779,0.00901235485834678,
-0.0103164410798053));
#38051=CARTESIAN_POINT('Ctrl Pts',(-0.213979298224174,0.00906419019480051,
-0.0103073200461676));
#38052=CARTESIAN_POINT('Ctrl Pts',(-0.213974912682964,0.00916786086770796,
-0.0102890779788922));
#38053=CARTESIAN_POINT('Ctrl Pts',(-0.213971323529434,0.00927310895773648,
-0.0102686660302547));
#38054=CARTESIAN_POINT('Ctrl Pts',(-0.213968703904558,0.00937559067791705,
-0.0102469536514785));
#38055=CARTESIAN_POINT('Ctrl Pts',(-0.213963464654806,0.00958055411827819,
-0.0102035288939261));
#38056=CARTESIAN_POINT('Ctrl Pts',(-0.213962093405312,0.00977455790650294,
-0.0101553670319792));
#38057=CARTESIAN_POINT('Ctrl Pts',(-0.213964868649422,0.00996900504123913,
-0.0101004321413189));
#38058=CARTESIAN_POINT('Ctrl Pts',(-0.213967643893531,0.0101634521759753,
-0.0100454972506585));
#38059=CARTESIAN_POINT('Ctrl Pts',(-0.213974569916396,0.0103582714553616,
-0.00998359248621707));
#38060=CARTESIAN_POINT('Ctrl Pts',(-0.213986389893635,0.0105553207042468,
-0.00991337070712582));
#38061=CARTESIAN_POINT('Ctrl Pts',(-0.213992299882255,0.0106538453286895,
-0.00987825981758019));
#38062=CARTESIAN_POINT('Ctrl Pts',(-0.213999434474098,0.0107529130711297,
-0.00984101847227842));
#38063=CARTESIAN_POINT('Ctrl Pts',(-0.21400742187768,0.0108494164592589,
-0.00980285548237111));
#38064=CARTESIAN_POINT('Ctrl Pts',(-0.214011415579471,0.0108976681533235,
-0.00978377398741745));
#38065=CARTESIAN_POINT('Ctrl Pts',(-0.214015621743677,0.0109452914242763,
-0.00976449609826157));
#38066=CARTESIAN_POINT('Ctrl Pts',(-0.214020508513958,0.0109964792354597,
-0.00974322294100645));
#38067=CARTESIAN_POINT('Ctrl Pts',(-0.21402539528424,0.0110476670466431,
-0.00972194978375133));
#38068=CARTESIAN_POINT('Ctrl Pts',(-0.214030965417441,0.01110236730927,
-0.00969855471836265));
#38069=CARTESIAN_POINT('Ctrl Pts',(-0.214035309917913,0.0111434638323282,
-0.00968062761879806));
#38070=CARTESIAN_POINT('Ctrl Pts',(-0.214039654418384,0.0111845603553864,
-0.00966270051923346));
#38071=CARTESIAN_POINT('Ctrl Pts',(-0.214042769408935,0.0112121317202152,
-0.00965041949073069));
#38072=CARTESIAN_POINT('Ctrl Pts',(-0.214046641062954,0.0112455515375233,
-0.00963535490389684));
#38073=CARTESIAN_POINT('Ctrl Pts',(-0.214050512716972,0.0112789713548313,
-0.00962029031706299));
#38074=CARTESIAN_POINT('Ctrl Pts',(-0.214055143146001,0.0113181950816343,
-0.0096023451745143));
#38075=CARTESIAN_POINT('Ctrl Pts',(-0.214060047891704,0.0113584579042877,
-0.00958353178581492));
#38076=CARTESIAN_POINT('Ctrl Pts',(-0.214069857383109,0.0114389835495945,
-0.00954590500841617));
#38077=CARTESIAN_POINT('Ctrl Pts',(-0.214080761500679,0.0115237248101962,
-0.00950492654375179));
#38078=CARTESIAN_POINT('Ctrl Pts',(-0.214093129479694,0.0116157377101813,
-0.00945835647233302));
#38079=CARTESIAN_POINT('Ctrl Pts',(-0.214117865437726,0.0117997635101515,
-0.00936521632949548));
#38080=CARTESIAN_POINT('Ctrl Pts',(-0.214148458802816,0.0120128210029322,
-0.00924961966466249));
#38081=CARTESIAN_POINT('Ctrl Pts',(-0.214184696860609,0.0122470177333751,
-0.00910661628414272));
#38082=CARTESIAN_POINT('Ctrl Pts',(-0.214184729330674,0.0122470252836163,
-0.00910661235527564));
#38083=CARTESIAN_POINT('Ctrl Pts',(-0.213850288464871,0.0122469812246611,
-0.00909935897740313));
#38084=CARTESIAN_POINT('Ctrl Pts',(-0.213516684455692,0.0122469406317341,
-0.00909212168842724));
#38085=CARTESIAN_POINT('Ctrl Pts',(-0.213184287727917,0.0122469034874106,
-0.00908490856303434));
#38086=CARTESIAN_POINT('Origin',(-0.223675719604735,0.00750000372932125,
-0.00172559146420468));
#38087=CARTESIAN_POINT('',(-0.223392319497656,0.0131379432052361,-0.00865273962921209));
#38088=CARTESIAN_POINT('',(-0.223092851198727,0.00750411713615694,-0.0106501152360551));
#38089=CARTESIAN_POINT('Ctrl Pts',(-0.223392319497656,0.0131379432052361,
-0.00865273962921209));
#38090=CARTESIAN_POINT('Ctrl Pts',(-0.223319870738354,0.0128800952029135,
-0.00886095679640992));
#38091=CARTESIAN_POINT('Ctrl Pts',(-0.223230386950221,0.0125275741399707,
-0.00911169714258552));
#38092=CARTESIAN_POINT('Ctrl Pts',(-0.223144924851994,0.0121246045072842,
-0.00936277629811845));
#38093=CARTESIAN_POINT('Ctrl Pts',(-0.223105570798993,0.0119109143796109,
-0.0094873958280264));
#38094=CARTESIAN_POINT('Ctrl Pts',(-0.223059101856131,0.0115847145998169,
-0.00966392505257264));
#38095=CARTESIAN_POINT('Ctrl Pts',(-0.223024275136112,0.011255422652783,
-0.00982367547305012));
#38096=CARTESIAN_POINT('Ctrl Pts',(-0.22299626632418,0.0108976150018631,
-0.00998025904879322));
#38097=CARTESIAN_POINT('Ctrl Pts',(-0.222969189537975,0.0103675478402047,
-0.0101824958926781));
#38098=CARTESIAN_POINT('Ctrl Pts',(-0.222960837342892,0.00989357905788291,
-0.0103271516041799));
#38099=CARTESIAN_POINT('Ctrl Pts',(-0.222966854203074,0.0094544751161954,
-0.0104324699590511));
#38100=CARTESIAN_POINT('Ctrl Pts',(-0.222973927346185,0.00921413881180308,
-0.0104823626331397));
#38101=CARTESIAN_POINT('Ctrl Pts',(-0.222982423102499,0.00900963355855106,
-0.0105197667134106));
#38102=CARTESIAN_POINT('Ctrl Pts',(-0.222988265756248,0.00889796473082585,
-0.0105380791660538));
#38103=CARTESIAN_POINT('Ctrl Pts',(-0.223000296289551,0.00869011684464469,
-0.0105697181567833));
#38104=CARTESIAN_POINT('Ctrl Pts',(-0.22302756304511,0.00828858110951311,
-0.0106196678946535));
#38105=CARTESIAN_POINT('Ctrl Pts',(-0.223063364931254,0.00784225216468286,
-0.0106493264355849));
#38106=CARTESIAN_POINT('Ctrl Pts',(-0.223092851198727,0.00750411713615694,
-0.0106501152360551));
#38107=CARTESIAN_POINT('',(-0.223398276290135,0.00187668424502486,-0.00866473290108311));
#38108=CARTESIAN_POINT('Ctrl Pts',(-0.223092851083271,0.00750411580413045,
-0.0106501152341876));
#38109=CARTESIAN_POINT('Ctrl Pts',(-0.223087327232776,0.00744038676315757,
-0.0106500258777345));
#38110=CARTESIAN_POINT('Ctrl Pts',(-0.223070830151961,0.0072462764610065,
-0.0106473681726595));
#38111=CARTESIAN_POINT('Ctrl Pts',(-0.223046896389284,0.00695246582810878,
-0.0106342335993294));
#38112=CARTESIAN_POINT('Ctrl Pts',(-0.223020042570552,0.0065999218171742,
-0.0106059269867326));
#38113=CARTESIAN_POINT('Ctrl Pts',(-0.22300100412444,0.00631589831769131,
-0.0105704887939461));
#38114=CARTESIAN_POINT('Ctrl Pts',(-0.222989208447741,0.00610913959330224,
-0.0105392233303175));
#38115=CARTESIAN_POINT('Ctrl Pts',(-0.222983537274156,0.00599855057050103,
-0.0105211674311498));
#38116=CARTESIAN_POINT('Ctrl Pts',(-0.222975416165749,0.0057972222654291,
-0.0104845864027248));
#38117=CARTESIAN_POINT('Ctrl Pts',(-0.222968660064301,0.00555785014105163,
-0.0104352496583974));
#38118=CARTESIAN_POINT('Ctrl Pts',(-0.222963230580807,0.00512057842839108,
-0.0103310664826879));
#38119=CARTESIAN_POINT('Ctrl Pts',(-0.222972107074572,0.00464542086187804,
-0.0101870267964044));
#38120=CARTESIAN_POINT('Ctrl Pts',(-0.222999678112803,0.00411212165983419,
-0.00998434144011729));
#38121=CARTESIAN_POINT('Ctrl Pts',(-0.223027825900457,0.00375402649109574,
-0.00982811005214637));
#38122=CARTESIAN_POINT('Ctrl Pts',(-0.223062687117585,0.00342540405800575,
-0.00966912797513253));
#38123=CARTESIAN_POINT('Ctrl Pts',(-0.223108723891955,0.00310293757098118,
-0.0094952680541608));
#38124=CARTESIAN_POINT('Ctrl Pts',(-0.223148477674354,0.00288825845475733,
-0.00937061521761407));
#38125=CARTESIAN_POINT('Ctrl Pts',(-0.223234583481303,0.00248626659602517,
-0.0091211101373121));
#38126=CARTESIAN_POINT('Ctrl Pts',(-0.223325021475566,0.00213415979343589,
-0.00887172811568694));
#38127=CARTESIAN_POINT('Ctrl Pts',(-0.223398276290135,0.00187668424502486,
-0.00866473290108311));
#38128=CARTESIAN_POINT('',(-0.224398147996022,0.00187716923648251,-0.0086866135867605));
#38129=CARTESIAN_POINT('Ctrl Pts',(-0.223398267584606,0.0018766830097055,
-0.00866473171331845));
#38130=CARTESIAN_POINT('Ctrl Pts',(-0.223731547637729,0.00187684536702503,
-0.00867202562098763));
#38131=CARTESIAN_POINT('Ctrl Pts',(-0.224064903826057,0.00187700183853765,
-0.00867931638700321));
#38132=CARTESIAN_POINT('Ctrl Pts',(-0.224398132591523,0.00187715232727695,
-0.00868659956029552));
#38133=CARTESIAN_POINT('',(-0.224092577864133,0.00750459921737242,-0.0106715875712242));
#38134=CARTESIAN_POINT('Ctrl Pts',(-0.224398147996022,0.00187716923648251,
-0.0086866135867605));
#38135=CARTESIAN_POINT('Ctrl Pts',(-0.224324606355394,0.00213579320645476,
-0.00889450206705218));
#38136=CARTESIAN_POINT('Ctrl Pts',(-0.224233796543426,0.00248988624564132,
-0.00914510760840042));
#38137=CARTESIAN_POINT('Ctrl Pts',(-0.224147406194117,0.00289433113124562,
-0.00939577762286241));
#38138=CARTESIAN_POINT('Ctrl Pts',(-0.224107349701666,0.00311189725424205,
-0.00952178404242857));
#38139=CARTESIAN_POINT('Ctrl Pts',(-0.224061875704077,0.00343247296487068,
-0.00969417693164834));
#38140=CARTESIAN_POINT('Ctrl Pts',(-0.224027253567691,0.00376014454372357,
-0.00985239135964685));
#38141=CARTESIAN_POINT('Ctrl Pts',(-0.223999340389896,0.00411678701536448,
-0.0100076863622763));
#38142=CARTESIAN_POINT('Ctrl Pts',(-0.223971952688012,0.0046474445615379,
-0.0102091401480788));
#38143=CARTESIAN_POINT('Ctrl Pts',(-0.223963070619058,0.00512398064154051,
-0.0103535176057558));
#38144=CARTESIAN_POINT('Ctrl Pts',(-0.223968602205114,0.00556175319243944,
-0.0104576018845324));
#38145=CARTESIAN_POINT('Ctrl Pts',(-0.223975415699836,0.0058015783603966,
-0.0105069145861535));
#38146=CARTESIAN_POINT('Ctrl Pts',(-0.223983597663641,0.00600344362452778,
-0.0105434921756839));
#38147=CARTESIAN_POINT('Ctrl Pts',(-0.223989361337856,0.00611564279954052,
-0.0105617243244171));
#38148=CARTESIAN_POINT('Ctrl Pts',(-0.224001170014523,0.00632279525898115,
-0.0105929495573639));
#38149=CARTESIAN_POINT('Ctrl Pts',(-0.224020493150551,0.00661020725445457,
-0.0106281277231074));
#38150=CARTESIAN_POINT('Ctrl Pts',(-0.224046205769023,0.0069490878284383,
-0.0106560024836772));
#38151=CARTESIAN_POINT('Ctrl Pts',(-0.224072028233643,0.00726436926979324,
-0.0106689252057769));
#38152=CARTESIAN_POINT('Ctrl Pts',(-0.2240842252329,0.00740810682501627,
-0.010671457912672));
#38153=CARTESIAN_POINT('Ctrl Pts',(-0.224092577864133,0.00750459921737242,
-0.0106715875712242));
#38154=CARTESIAN_POINT('',(-0.224391717827447,0.0131382574628826,-0.00867393727785756));
#38155=CARTESIAN_POINT('Ctrl Pts',(-0.224092578003526,0.00750460082767304,
-0.0106715875733879));
#38156=CARTESIAN_POINT('Ctrl Pts',(-0.22406295489172,0.00784473299941522,
-0.010670775927101));
#38157=CARTESIAN_POINT('Ctrl Pts',(-0.224027030414954,0.00829347663740902,
-0.0106407627709499));
#38158=CARTESIAN_POINT('Ctrl Pts',(-0.223999740369017,0.008697043734868,
-0.0105902556410251));
#38159=CARTESIAN_POINT('Ctrl Pts',(-0.223987747099335,0.00890554018645671,
-0.0105583463523279));
#38160=CARTESIAN_POINT('Ctrl Pts',(-0.223981909747232,0.00901824998727424,
-0.010539746396188));
#38161=CARTESIAN_POINT('Ctrl Pts',(-0.223973591662315,0.00922104189434486,
-0.0105024653322432));
#38162=CARTESIAN_POINT('Ctrl Pts',(-0.223966650813448,0.0094600836684451,
-0.0104526716603005));
#38163=CARTESIAN_POINT('Ctrl Pts',(-0.22396082625537,0.00989692323941784,
-0.0103475911356174));
#38164=CARTESIAN_POINT('Ctrl Pts',(-0.2239690669497,0.0103666723157455,
-0.0102042766054829));
#38165=CARTESIAN_POINT('Ctrl Pts',(-0.223996160315981,0.0108988366543281,
-0.0100012575347548));
#38166=CARTESIAN_POINT('Ctrl Pts',(-0.22402419040041,0.0112571751904465,
-0.00984433623679992));
#38167=CARTESIAN_POINT('Ctrl Pts',(-0.224059042622487,0.0115869929132631,
-0.00968423835129144));
#38168=CARTESIAN_POINT('Ctrl Pts',(-0.224105611700866,0.011913804457731,
-0.00950722646718586));
#38169=CARTESIAN_POINT('Ctrl Pts',(-0.224144860648786,0.012126837978164,
-0.00938288306593188));
#38170=CARTESIAN_POINT('Ctrl Pts',(-0.224230166524884,0.012529155718252,
-0.0091320634968813));
#38171=CARTESIAN_POINT('Ctrl Pts',(-0.224319441634422,0.0128809283761845,
-0.00888175630073892));
#38172=CARTESIAN_POINT('Ctrl Pts',(-0.224391717827447,0.0131382574628826,
-0.00867393727785756));
#38173=CARTESIAN_POINT('Ctrl Pts',(-0.224391700636746,0.013138269070805,
-0.00867392746427423));
#38174=CARTESIAN_POINT('Ctrl Pts',(-0.224058345684202,0.0131381552026779,
-0.00866686423347615));
#38175=CARTESIAN_POINT('Ctrl Pts',(-0.223725131075681,0.0131380471806954,
-0.00865979925365354));
#38176=CARTESIAN_POINT('Ctrl Pts',(-0.223392308938441,0.0131379450563949,
-0.00865273789653389));
#38177=CARTESIAN_POINT('Origin',(-0.211568189915785,0.00750000024019488,
-0.00128323523926141));
#38178=CARTESIAN_POINT('',(-0.21118342070055,0.0122493195087978,-0.009043325341704));
#38179=CARTESIAN_POINT('',(-0.211096534876114,0.00750002174791387,-0.0103787794824388));
#38180=CARTESIAN_POINT('Ctrl Pts',(-0.21118342070055,0.0122493195087978,
-0.009043325341704));
#38181=CARTESIAN_POINT('Ctrl Pts',(-0.211147075853411,0.0120146153758137,
-0.00918609110004283));
#38182=CARTESIAN_POINT('Ctrl Pts',(-0.211101126056254,0.0116945334709256,
-0.00935899282289318));
#38183=CARTESIAN_POINT('Ctrl Pts',(-0.211063031695026,0.0113977919415671,
-0.00950208910682082));
#38184=CARTESIAN_POINT('Ctrl Pts',(-0.211044625840369,0.0112410518606829,
-0.0095734525507458));
#38185=CARTESIAN_POINT('Ctrl Pts',(-0.211035314537477,0.0111580846306274,
-0.00961034898322537));
#38186=CARTESIAN_POINT('Ctrl Pts',(-0.211018942999683,0.0109956430019049,
-0.00967965113480102));
#38187=CARTESIAN_POINT('Ctrl Pts',(-0.211002445396812,0.0108059307774903,
-0.00975612785596291));
#38188=CARTESIAN_POINT('Ctrl Pts',(-0.210978052341354,0.0104602185049158,
-0.00988599885738961));
#38189=CARTESIAN_POINT('Ctrl Pts',(-0.210961408558488,0.0099657835293919,
-0.0100422465505005));
#38190=CARTESIAN_POINT('Ctrl Pts',(-0.21096547560556,0.00948426681055532,
-0.0101613871041555));
#38191=CARTESIAN_POINT('Ctrl Pts',(-0.210978341736303,0.00911600746241873,
-0.0102326044618298));
#38192=CARTESIAN_POINT('Ctrl Pts',(-0.210988044352495,0.00891043600357915,
-0.0102670716292219));
#38193=CARTESIAN_POINT('Ctrl Pts',(-0.210998326477394,0.00872874261242559,
-0.0102936849955648));
#38194=CARTESIAN_POINT('Ctrl Pts',(-0.211004044914085,0.00864037334831602,
-0.0103052055025708));
#38195=CARTESIAN_POINT('Ctrl Pts',(-0.211015798923584,0.00846851034186375,
-0.0103261628486553));
#38196=CARTESIAN_POINT('Ctrl Pts',(-0.21104070236026,0.00814026567965264,
-0.0103588017271737));
#38197=CARTESIAN_POINT('Ctrl Pts',(-0.211071667771316,0.00777569081607782,
-0.0103782378584628));
#38198=CARTESIAN_POINT('Ctrl Pts',(-0.211096534876114,0.00750002174791387,
-0.0103787794824388));
#38199=CARTESIAN_POINT('',(-0.211184192776991,0.00275281494927484,-0.00904464640986752));
#38200=CARTESIAN_POINT('Ctrl Pts',(-0.211096534773062,0.00750002061052517,
-0.0103787794801929));
#38201=CARTESIAN_POINT('Ctrl Pts',(-0.211096372089148,0.00749822498476027,
-0.0103787759245625));
#38202=CARTESIAN_POINT('Ctrl Pts',(-0.211091269818405,0.00744179752197237,
-0.010378568095464));
#38203=CARTESIAN_POINT('Ctrl Pts',(-0.211086202258332,0.00738520865215235,
-0.0103778882206662));
#38204=CARTESIAN_POINT('Ctrl Pts',(-0.211075357694199,0.00726324121015861,
-0.0103757196011447));
#38205=CARTESIAN_POINT('Ctrl Pts',(-0.211062090540266,0.00711042797893358,
-0.0103702493396725));
#38206=CARTESIAN_POINT('Ctrl Pts',(-0.211047251633211,0.00693429006983655,
-0.0103606551626359));
#38207=CARTESIAN_POINT('Ctrl Pts',(-0.211029718484758,0.00671798930303775,
-0.0103446970608107));
#38208=CARTESIAN_POINT('Ctrl Pts',(-0.211015469076438,0.00653052937502733,
-0.0103260547268499));
#38209=CARTESIAN_POINT('Ctrl Pts',(-0.211003724232673,0.00635858874913573,
-0.0103050683605631));
#38210=CARTESIAN_POINT('Ctrl Pts',(-0.210998005903544,0.00626993368874563,
-0.010293494688143));
#38211=CARTESIAN_POINT('Ctrl Pts',(-0.210987839649527,0.00608916568458587,
-0.010266999569767));
#38212=CARTESIAN_POINT('Ctrl Pts',(-0.210978254538632,0.00588405688678575,
-0.0102326085786644));
#38213=CARTESIAN_POINT('Ctrl Pts',(-0.210965627361286,0.00551657670016644,
-0.0101615840585635));
#38214=CARTESIAN_POINT('Ctrl Pts',(-0.210961985602812,0.00503295150595074,
-0.0100418962433909));
#38215=CARTESIAN_POINT('Ctrl Pts',(-0.210978985441477,0.00454104539977056,
-0.00988643540233352));
#38216=CARTESIAN_POINT('Ctrl Pts',(-0.211003574831235,0.00419499500178585,
-0.00975651549375403));
#38217=CARTESIAN_POINT('Ctrl Pts',(-0.21102015926641,0.00400507401732748,
-0.00967997805343405));
#38218=CARTESIAN_POINT('Ctrl Pts',(-0.211036621559236,0.00384205348628263,
-0.00961043850454111));
#38219=CARTESIAN_POINT('Ctrl Pts',(-0.211045891149871,0.00375951174937592,
-0.00957373108287534));
#38220=CARTESIAN_POINT('Ctrl Pts',(-0.211064262875409,0.00360301705517485,
-0.00950249609276564));
#38221=CARTESIAN_POINT('Ctrl Pts',(-0.211102233289035,0.00330686034690693,
-0.009359722009264));
#38222=CARTESIAN_POINT('Ctrl Pts',(-0.211148004045778,0.00298722410298725,
-0.00918714660229151));
#38223=CARTESIAN_POINT('Ctrl Pts',(-0.211184192776991,0.00275281494927484,
-0.00904464640986752));
#38224=CARTESIAN_POINT('',(-0.212184966502507,0.00275261962744201,-0.009066300433649));
#38225=CARTESIAN_POINT('Ctrl Pts',(-0.211184242601052,0.00275281783271421,
-0.00904464925643142));
#38226=CARTESIAN_POINT('Ctrl Pts',(-0.211517534893567,0.00275275115143515,
-0.00905185979923313));
#38227=CARTESIAN_POINT('Ctrl Pts',(-0.211851205378944,0.00275268083048704,
-0.00905907634424748));
#38228=CARTESIAN_POINT('Ctrl Pts',(-0.212185002205565,0.00275260690551022,
-0.00906629343342788));
#38229=CARTESIAN_POINT('',(-0.212096215740483,0.00750006061885404,-0.0104005278051053));
#38230=CARTESIAN_POINT('Ctrl Pts',(-0.212184966502507,0.00275261962744201,
-0.009066300433649));
#38231=CARTESIAN_POINT('Ctrl Pts',(-0.212148608821063,0.00298809828782967,
-0.00920945875312566));
#38232=CARTESIAN_POINT('Ctrl Pts',(-0.212117948616956,0.00320218746771227,
-0.00932506036133119));
#38233=CARTESIAN_POINT('Ctrl Pts',(-0.212093184999995,0.00338706586627467,
-0.00941816979041781));
#38234=CARTESIAN_POINT('Ctrl Pts',(-0.212080803191514,0.00347950506555587,
-0.00946472450496112));
#38235=CARTESIAN_POINT('Ctrl Pts',(-0.212069895077993,0.00356462887386294,
-0.00950567694212421));
#38236=CARTESIAN_POINT('Ctrl Pts',(-0.212060103592096,0.00364539886507545,
-0.00954322274361884));
#38237=CARTESIAN_POINT('Ctrl Pts',(-0.212055207849147,0.0036857838606817,
-0.00956199564436615));
#38238=CARTESIAN_POINT('Ctrl Pts',(-0.212050591906104,0.00372509475974982,
-0.00957988733157869));
#38239=CARTESIAN_POINT('Ctrl Pts',(-0.21204672334139,0.00375869560595558,
-0.00959495384536575));
#38240=CARTESIAN_POINT('Ctrl Pts',(-0.212042854776675,0.00379229645216134,
-0.00961002035915281));
#38241=CARTESIAN_POINT('Ctrl Pts',(-0.212039731540024,0.00382014420653861,
-0.00962235593746418));
#38242=CARTESIAN_POINT('Ctrl Pts',(-0.21203543633928,0.0038610821910094,
-0.00964011866024805));
#38243=CARTESIAN_POINT('Ctrl Pts',(-0.212031141138537,0.00390202017548019,
-0.00965788138303192));
#38244=CARTESIAN_POINT('Ctrl Pts',(-0.212025677698956,0.00395612350844896,
-0.00968090002320027));
#38245=CARTESIAN_POINT('Ctrl Pts',(-0.212020875548343,0.0040068650364192,
-0.00970188426642679));
#38246=CARTESIAN_POINT('Ctrl Pts',(-0.21201607339773,0.00405760656438943,
-0.00972286850965331));
#38247=CARTESIAN_POINT('Ctrl Pts',(-0.212011929909662,0.00410493688815609,
-0.00974193907695546));
#38248=CARTESIAN_POINT('Ctrl Pts',(-0.212007996642503,0.00415289807641202,
-0.00976081980110558));
#38249=CARTESIAN_POINT('Ctrl Pts',(-0.212000130108185,0.00424882045292389,
-0.00979858124940582));
#38250=CARTESIAN_POINT('Ctrl Pts',(-0.211993107258692,0.00434731387725675,
-0.00983545457074571));
#38251=CARTESIAN_POINT('Ctrl Pts',(-0.21198728236806,0.00444547316953737,
-0.00987029799021983));
#38252=CARTESIAN_POINT('Ctrl Pts',(-0.211975632586797,0.00464179175409861,
-0.00993998482916808));
#38253=CARTESIAN_POINT('Ctrl Pts',(-0.211968770979782,0.00483672941011492,
-0.0100017203464364));
#38254=CARTESIAN_POINT('Ctrl Pts',(-0.211966011865899,0.00503103822754167,
-0.0100564228393022));
#38255=CARTESIAN_POINT('Ctrl Pts',(-0.211963252752017,0.00522534704496841,
-0.010111125332168));
#38256=CARTESIAN_POINT('Ctrl Pts',(-0.211964591385878,0.00541895104039878,
-0.0101590129190598));
#38257=CARTESIAN_POINT('Ctrl Pts',(-0.211969770051672,0.00562307980497558,
-0.0102021454556335));
#38258=CARTESIAN_POINT('Ctrl Pts',(-0.211972359384569,0.00572514418726399,
-0.0102237117239204));
#38259=CARTESIAN_POINT('Ctrl Pts',(-0.211975911186776,0.00582986526912701,
-0.0102439760950727));
#38260=CARTESIAN_POINT('Ctrl Pts',(-0.211980255990761,0.00593300677166175,
-0.0102620974047736));
#38261=CARTESIAN_POINT('Ctrl Pts',(-0.211982428392754,0.00598457752292912,
-0.010271158059624));
#38262=CARTESIAN_POINT('Ctrl Pts',(-0.211984798161859,0.00603574571201802,
-0.0102797235514748));
#38263=CARTESIAN_POINT('Ctrl Pts',(-0.211987658262279,0.00609135335842438,
-0.0102884971298513));
#38264=CARTESIAN_POINT('Ctrl Pts',(-0.211990518362698,0.00614696100483073,
-0.0102972707082277));
#38265=CARTESIAN_POINT('Ctrl Pts',(-0.211993871951416,0.00620703157474658,
-0.0103061072618912));
#38266=CARTESIAN_POINT('Ctrl Pts',(-0.211996503008621,0.00625191141560677,
-0.0103123775364578));
#38267=CARTESIAN_POINT('Ctrl Pts',(-0.211999134065825,0.00629679125646696,
-0.0103186478110244));
#38268=CARTESIAN_POINT('Ctrl Pts',(-0.212001038147609,0.00632645261086889,
-0.0103225560719346));
#38269=CARTESIAN_POINT('Ctrl Pts',(-0.21200345637053,0.00636279070500133,
-0.0103271848758392));
#38270=CARTESIAN_POINT('Ctrl Pts',(-0.212005874593451,0.00639912879913378,
-0.0103318136797438));
#38271=CARTESIAN_POINT('Ctrl Pts',(-0.212008809361001,0.00644215698030905,
-0.0103370525494413));
#38272=CARTESIAN_POINT('Ctrl Pts',(-0.212011958500563,0.00648652347538562,
-0.0103420922865668));
#38273=CARTESIAN_POINT('Ctrl Pts',(-0.212018256779686,0.00657525646553876,
-0.0103521717608177));
#38274=CARTESIAN_POINT('Ctrl Pts',(-0.212025409498654,0.00666932914028881,
-0.0103615948168621));
#38275=CARTESIAN_POINT('Ctrl Pts',(-0.212033655768505,0.00677269298518827,
-0.0103700605683433));
#38276=CARTESIAN_POINT('Ctrl Pts',(-0.212050148308207,0.00697942067498721,
-0.0103869920713057));
#38277=CARTESIAN_POINT('Ctrl Pts',(-0.212071017506775,0.00722331365218771,
-0.0103999814945091));
#38278=CARTESIAN_POINT('Ctrl Pts',(-0.212096215740485,0.00750006061883522,
-0.0104005278051053));
#38279=CARTESIAN_POINT('',(-0.212183785378815,0.0122487124732956,-0.0090654584774169));
#38280=CARTESIAN_POINT('Ctrl Pts',(-0.212096215740483,0.00750006061885404,
-0.0104005278051053));
#38281=CARTESIAN_POINT('Ctrl Pts',(-0.212071084803046,0.00777720907168359,
-0.0103999791884765));
#38282=CARTESIAN_POINT('Ctrl Pts',(-0.212050255631567,0.00802145530645392,
-0.0103869514333805));
#38283=CARTESIAN_POINT('Ctrl Pts',(-0.212033775329214,0.00822850316358781,
-0.0103699670068986));
#38284=CARTESIAN_POINT('Ctrl Pts',(-0.212025535178038,0.00833202709215476,
-0.0103614747936577));
#38285=CARTESIAN_POINT('Ctrl Pts',(-0.212018381635708,0.00842625156415626,
-0.0103520213798588));
#38286=CARTESIAN_POINT('Ctrl Pts',(-0.212012075565743,0.00851511137322495,
-0.0103419112432895));
#38287=CARTESIAN_POINT('Ctrl Pts',(-0.21200892253076,0.00855954127775929,
-0.0103368561750048));
#38288=CARTESIAN_POINT('Ctrl Pts',(-0.212005982124083,0.00860262662677667,
-0.0103316019817392));
#38289=CARTESIAN_POINT('Ctrl Pts',(-0.212003556482991,0.00863903890015032,
-0.010326956172219));
#38290=CARTESIAN_POINT('Ctrl Pts',(-0.212001130841899,0.00867545117352398,
-0.0103223103626988));
#38291=CARTESIAN_POINT('Ctrl Pts',(-0.211999217569435,0.00870520370405761,
-0.0103183831165034));
#38292=CARTESIAN_POINT('Ctrl Pts',(-0.211996575654735,0.00875009675291833,
-0.0103121005759226));
#38293=CARTESIAN_POINT('Ctrl Pts',(-0.211993933740034,0.00879498980177905,
-0.0103058180353417));
#38294=CARTESIAN_POINT('Ctrl Pts',(-0.211990567611169,0.00885499566654293,
-0.0102969766573737));
#38295=CARTESIAN_POINT('Ctrl Pts',(-0.211987691838397,0.00891053313075946,
-0.0102882017827607));
#38296=CARTESIAN_POINT('Ctrl Pts',(-0.211984816065626,0.00896607059497598,
-0.0102794269081478));
#38297=CARTESIAN_POINT('Ctrl Pts',(-0.211982427503353,0.00901716305253132,
-0.0102708631292185));
#38298=CARTESIAN_POINT('Ctrl Pts',(-0.211980234043084,0.00906865320441798,
-0.0102618062674016));
#38299=CARTESIAN_POINT('Ctrl Pts',(-0.211975847122544,0.00917163350819128,
-0.0102436925437678));
#38300=CARTESIAN_POINT('Ctrl Pts',(-0.211972244195427,0.00927617380797614,
-0.0102234416789181));
#38301=CARTESIAN_POINT('Ctrl Pts',(-0.211969587228889,0.00937781729810693,
-0.0102019519260732));
#38302=CARTESIAN_POINT('Ctrl Pts',(-0.211964273295813,0.00958110427836849,
-0.0101589724203835));
#38303=CARTESIAN_POINT('Ctrl Pts',(-0.211962731868439,0.00977291813170571,
-0.0101115584715891));
#38304=CARTESIAN_POINT('Ctrl Pts',(-0.211965304925825,0.00996713451424829,
-0.0100569216533234));
#38305=CARTESIAN_POINT('Ctrl Pts',(-0.211967877983211,0.0101613508967909,
-0.0100022848350576));
#38306=CARTESIAN_POINT('Ctrl Pts',(-0.211974572774418,0.0103578615668069,
-0.00994009192707719));
#38307=CARTESIAN_POINT('Ctrl Pts',(-0.211986103882925,0.010554810494706,
-0.00987017052721041));
#38308=CARTESIAN_POINT('Ctrl Pts',(-0.211991869437178,0.0106532849586555,
-0.00983520982727702));
#38309=CARTESIAN_POINT('Ctrl Pts',(-0.211998844621251,0.0107518644913665,
-0.00979829169999918));
#38310=CARTESIAN_POINT('Ctrl Pts',(-0.212006673594954,0.010847876094752,
-0.00976048395358538));
#38311=CARTESIAN_POINT('Ctrl Pts',(-0.212010588081806,0.0108958818964447,
-0.00974158008037848));
#38312=CARTESIAN_POINT('Ctrl Pts',(-0.212014715332133,0.0109432572343657,
-0.00972248524111358));
#38313=CARTESIAN_POINT('Ctrl Pts',(-0.212019502672067,0.0109940178498293,
-0.00970148646569386));
#38314=CARTESIAN_POINT('Ctrl Pts',(-0.212024290012001,0.0110447784652929,
-0.00968048769027414));
#38315=CARTESIAN_POINT('Ctrl Pts',(-0.212029740059852,0.0110988751152101,
-0.0096574646208909));
#38316=CARTESIAN_POINT('Ctrl Pts',(-0.212034028469476,0.0111398206347841,
-0.00963969316884266));
#38317=CARTESIAN_POINT('Ctrl Pts',(-0.212038316879101,0.011180766154358,
-0.00962192171679442));
#38318=CARTESIAN_POINT('Ctrl Pts',(-0.212041439931195,0.0112086355631204,
-0.00960957285060339));
#38319=CARTESIAN_POINT('Ctrl Pts',(-0.212045308690276,0.0112422548710201,
-0.00959449336407188));
#38320=CARTESIAN_POINT('Ctrl Pts',(-0.212049177449357,0.0112758741789197,
-0.00957941387754037));
#38321=CARTESIAN_POINT('Ctrl Pts',(-0.212053793964691,0.0113152003528337,
-0.00956150957010244));
#38322=CARTESIAN_POINT('Ctrl Pts',(-0.212058692181928,0.0113556016114075,
-0.00954272312340504));
#38323=CARTESIAN_POINT('Ctrl Pts',(-0.2120684886164,0.011436404128555,-0.00950515023001024));
#38324=CARTESIAN_POINT('Ctrl Pts',(-0.212079409287647,0.0115215644114706,
-0.00946416695603335));
#38325=CARTESIAN_POINT('Ctrl Pts',(-0.212091810164631,0.0116140405560105,
-0.0094175780460792));
#38326=CARTESIAN_POINT('Ctrl Pts',(-0.212116611918599,0.0117989928450904,
-0.00932440022617091));
#38327=CARTESIAN_POINT('Ctrl Pts',(-0.212147336299191,0.0120131578667162,
-0.00920871694976559));
#38328=CARTESIAN_POINT('Ctrl Pts',(-0.212183785378815,0.0122487124732956,
-0.0090654584774169));
#38329=CARTESIAN_POINT('Ctrl Pts',(-0.21218382236874,0.0122487203634196,
-0.00906545445695096));
#38330=CARTESIAN_POINT('Ctrl Pts',(-0.211850415340402,0.0122489172355382,
-0.00905808114379708));
#38331=CARTESIAN_POINT('Ctrl Pts',(-0.211516897126879,0.0122491175732441,
-0.0090507032823604));
#38332=CARTESIAN_POINT('Ctrl Pts',(-0.211183475876664,0.0122493212504455,
-0.00904332547672575));
#38333=CARTESIAN_POINT('Origin',(-0.201568762588454,0.00750000073597594,
-0.000898605665389165));
#38334=CARTESIAN_POINT('',(-0.201180432939979,0.0122595231330948,-0.00883793092373448));
#38335=CARTESIAN_POINT('',(-0.201099841269113,0.00750066886075073,-0.0101529052291387));
#38336=CARTESIAN_POINT('Ctrl Pts',(-0.201180432939979,0.0122595231330948,
-0.00883793092373448));
#38337=CARTESIAN_POINT('Ctrl Pts',(-0.201143740554226,0.0120228137257047,
-0.00897895597246862));
#38338=CARTESIAN_POINT('Ctrl Pts',(-0.20109822872155,0.0117071699584008,
-0.00914678199504796));
#38339=CARTESIAN_POINT('Ctrl Pts',(-0.20105352550923,0.0113497843899364,
-0.00931471227512171));
#38340=CARTESIAN_POINT('Ctrl Pts',(-0.201033187159162,0.0111728352939134,
-0.00939335080989536));
#38341=CARTESIAN_POINT('Ctrl Pts',(-0.201004811740894,0.0108597897901084,
-0.00952200041603991));
#38342=CARTESIAN_POINT('Ctrl Pts',(-0.200980796925748,0.0104817056607582,
-0.00966132613367734));
#38343=CARTESIAN_POINT('Ctrl Pts',(-0.200965879775637,0.00995831253814996,
-0.00982474718393346));
#38344=CARTESIAN_POINT('Ctrl Pts',(-0.200972104318261,0.00949743717135199,
-0.00993630501398072));
#38345=CARTESIAN_POINT('Ctrl Pts',(-0.200985841120966,0.00912458516838106,
-0.0100078469251149));
#38346=CARTESIAN_POINT('Ctrl Pts',(-0.200995917543769,0.00891603011605418,
-0.0100423599010609));
#38347=CARTESIAN_POINT('Ctrl Pts',(-0.201006511373127,0.00872931824135355,
-0.0100692983593163));
#38348=CARTESIAN_POINT('Ctrl Pts',(-0.201012139020932,0.00864096664753087,
-0.0100806012456826));
#38349=CARTESIAN_POINT('Ctrl Pts',(-0.201023644166776,0.00846779200223077,
-0.0101013573951201));
#38350=CARTESIAN_POINT('Ctrl Pts',(-0.201047512603945,0.00813892243805578,
-0.0101334243263926));
#38351=CARTESIAN_POINT('Ctrl Pts',(-0.201076639535349,0.00777509809593754,
-0.0101523824149227));
#38352=CARTESIAN_POINT('Ctrl Pts',(-0.20109984171623,0.00750066914084511,
-0.0101529052406882));
#38353=CARTESIAN_POINT('',(-0.201177675620458,0.00274510091024268,-0.00884063751610791));
#38354=CARTESIAN_POINT('Ctrl Pts',(-0.201099841689236,0.00750066882484645,
-0.0101529052401256));
#38355=CARTESIAN_POINT('Ctrl Pts',(-0.201097897029398,0.00747790081601996,
-0.0101528647152854));
#38356=CARTESIAN_POINT('Ctrl Pts',(-0.201090755424158,0.00739389932697868,
-0.0101523381855469));
#38357=CARTESIAN_POINT('Ctrl Pts',(-0.201080428616844,0.0072706848013662,
-0.0101499681004645));
#38358=CARTESIAN_POINT('Ctrl Pts',(-0.201062017942989,0.00704727154987918,
-0.0101425305811733));
#38359=CARTESIAN_POINT('Ctrl Pts',(-0.201040076465639,0.0067682941608778,
-0.0101242894215651));
#38360=CARTESIAN_POINT('Ctrl Pts',(-0.201022784868407,0.0065326874925701,
-0.0101013964972095));
#38361=CARTESIAN_POINT('Ctrl Pts',(-0.201011167483721,0.00635960375819356,
-0.0100806496042055));
#38362=CARTESIAN_POINT('Ctrl Pts',(-0.20100547097909,0.00627106324120422,
-0.0100693241425073));
#38363=CARTESIAN_POINT('Ctrl Pts',(-0.200994813431936,0.00608513452974621,
-0.0100425115383475));
#38364=CARTESIAN_POINT('Ctrl Pts',(-0.200984632920064,0.00587674000196599,
-0.0100080544960793));
#38365=CARTESIAN_POINT('Ctrl Pts',(-0.200970747022194,0.00550448498314526,
-0.00993669158873135));
#38366=CARTESIAN_POINT('Ctrl Pts',(-0.20096438802479,0.00504326515784926,
-0.0098251294401078));
#38367=CARTESIAN_POINT('Ctrl Pts',(-0.200979186972993,0.00452135562915181,
-0.00966231257002147));
#38368=CARTESIAN_POINT('Ctrl Pts',(-0.201003103960677,0.00414328927105012,
-0.0095231669350311));
#38369=CARTESIAN_POINT('Ctrl Pts',(-0.20103144157648,0.00382962576004159,
-0.00939437461606553));
#38370=CARTESIAN_POINT('Ctrl Pts',(-0.201051630275061,0.00365329789975121,
-0.00931606955853783));
#38371=CARTESIAN_POINT('Ctrl Pts',(-0.201096047091507,0.00329650799822964,
-0.00914858984126155));
#38372=CARTESIAN_POINT('Ctrl Pts',(-0.20114124093058,0.00298143730432313,
-0.00898125778455622));
#38373=CARTESIAN_POINT('Ctrl Pts',(-0.201177675620458,0.00274510091024268,
-0.00884063751610791));
#38374=CARTESIAN_POINT('',(-0.202178390238509,0.00274518461141551,-0.00886238765667538));
#38375=CARTESIAN_POINT('Ctrl Pts',(-0.201177763351363,0.00274510393520155,
-0.00884064122847788));
#38376=CARTESIAN_POINT('Ctrl Pts',(-0.201513793943995,0.00274513082230744,
-0.00884794399274696));
#38377=CARTESIAN_POINT('Ctrl Pts',(-0.201847555253796,0.00274515324551409,
-0.00885519487746271));
#38378=CARTESIAN_POINT('Ctrl Pts',(-0.202178455596619,0.00274517135762337,
-0.0088623811438036));
#38379=CARTESIAN_POINT('',(-0.202099486167777,0.00750048618412189,-0.0101745790373482));
#38380=CARTESIAN_POINT('Ctrl Pts',(-0.202178390238509,0.00274518461141551,
-0.00886238765667538));
#38381=CARTESIAN_POINT('Ctrl Pts',(-0.202141642700174,0.00298280250174922,
-0.00900376430935615));
#38382=CARTESIAN_POINT('Ctrl Pts',(-0.202096073383157,0.00329970770692211,
-0.00917193867634351));
#38383=CARTESIAN_POINT('Ctrl Pts',(-0.202051385104703,0.00365806649196233,
-0.00933994400439029));
#38384=CARTESIAN_POINT('Ctrl Pts',(-0.202031013291299,0.00383620024345885,
-0.00941887465041026));
#38385=CARTESIAN_POINT('Ctrl Pts',(-0.202002918010045,0.00414758988742412,
-0.0095464889586151));
#38386=CARTESIAN_POINT('Ctrl Pts',(-0.201979077837791,0.00452405425854171,
-0.00968486858469979));
#38387=CARTESIAN_POINT('Ctrl Pts',(-0.201964259756075,0.00504260003922919,
-0.00984656774115697));
#38388=CARTESIAN_POINT('Ctrl Pts',(-0.201970466218556,0.00550352850911395,
-0.00995814839597316));
#38389=CARTESIAN_POINT('Ctrl Pts',(-0.20198425173622,0.0058749187926387,
-0.0100293983289797));
#38390=CARTESIAN_POINT('Ctrl Pts',(-0.201994368236462,0.0060828133308569,
-0.0100638226599408));
#38391=CARTESIAN_POINT('Ctrl Pts',(-0.20200497764798,0.00626846786176619,
-0.0100906480095422));
#38392=CARTESIAN_POINT('Ctrl Pts',(-0.202010677229979,0.00635725597980151,
-0.0101020286816427));
#38393=CARTESIAN_POINT('Ctrl Pts',(-0.20202228103975,0.00653043393283875,
-0.0101228400557603));
#38394=CARTESIAN_POINT('Ctrl Pts',(-0.202039641458584,0.00676707384825273,
-0.0101458231096576));
#38395=CARTESIAN_POINT('Ctrl Pts',(-0.202061412767996,0.00704417286928311,
-0.0101641363102107));
#38396=CARTESIAN_POINT('Ctrl Pts',(-0.202082889000625,0.00730462260352203,
-0.0101726906059738));
#38397=CARTESIAN_POINT('Ctrl Pts',(-0.202092355332572,0.00741701669310581,
-0.0101744288378058));
#38398=CARTESIAN_POINT('Ctrl Pts',(-0.20209948616598,0.00750048592111213,
-0.0101745790373231));
#38399=CARTESIAN_POINT('',(-0.202180670184565,0.0122592735600236,-0.00885976401094108));
#38400=CARTESIAN_POINT('Ctrl Pts',(-0.202099486167777,0.00750048618412189,
-0.0101745790373482));
#38401=CARTESIAN_POINT('Ctrl Pts',(-0.202076106016961,0.00777643690849919,
-0.0101740575426325));
#38402=CARTESIAN_POINT('Ctrl Pts',(-0.202046783464256,0.00814210139549289,
-0.0101549087136242));
#38403=CARTESIAN_POINT('Ctrl Pts',(-0.202022790521316,0.00847257147790718,
-0.0101225200596911));
#38404=CARTESIAN_POINT('Ctrl Pts',(-0.202011260789241,0.00864623057456113,
-0.0101016120625616));
#38405=CARTESIAN_POINT('Ctrl Pts',(-0.202005589674707,0.00873549249903804,
-0.0100901265418475));
#38406=CARTESIAN_POINT('Ctrl Pts',(-0.201995124325738,0.0089205474429524,
-0.0100633132683614));
#38407=CARTESIAN_POINT('Ctrl Pts',(-0.201985141205441,0.00912791605188965,
-0.0100289077382085));
#38408=CARTESIAN_POINT('Ctrl Pts',(-0.201971560044696,0.0094984739199577,
-0.00995769693082072));
#38409=CARTESIAN_POINT('Ctrl Pts',(-0.201965440095476,0.00995740917196224,
-0.00984660305171449));
#38410=CARTESIAN_POINT('Ctrl Pts',(-0.201980326512632,0.0104783224757965,
-0.00968411601573794));
#38411=CARTESIAN_POINT('Ctrl Pts',(-0.202004276740897,0.0108552791705883,
-0.009545404489792));
#38412=CARTESIAN_POINT('Ctrl Pts',(-0.202032481994145,0.0111669978914189,
-0.00941752983743049));
#38413=CARTESIAN_POINT('Ctrl Pts',(-0.202052945089522,0.0113452706979188,
-0.0093384552071316));
#38414=CARTESIAN_POINT('Ctrl Pts',(-0.202097867963932,0.0117040370740209,
-0.00917008223814911));
#38415=CARTESIAN_POINT('Ctrl Pts',(-0.202143701978128,0.0120213473325891,
-0.00900150217001001));
#38416=CARTESIAN_POINT('Ctrl Pts',(-0.202180670184565,0.0122592735600236,
-0.00885976401094108));
#38417=CARTESIAN_POINT('Ctrl Pts',(-0.202180736625232,0.012259282168623,
-0.00885976029392518));
#38418=CARTESIAN_POINT('Ctrl Pts',(-0.20184764381904,0.0122593589071325,
-0.00885249339404029));
#38419=CARTESIAN_POINT('Ctrl Pts',(-0.201514155362888,0.0122594397984704,
-0.008845215427718));
#38420=CARTESIAN_POINT('Ctrl Pts',(-0.201180522815623,0.0122595247994947,
-0.00883793187370074));
#38421=CARTESIAN_POINT('Origin',(-0.199568871480718,0.0075000007634268,
-0.000819355499014377));
#38422=CARTESIAN_POINT('',(-0.199179703927896,0.0122617568640769,-0.00879700974463651));
#38423=CARTESIAN_POINT('',(-0.199100855044633,0.00750164282994255,-0.0101077379410075));
#38424=CARTESIAN_POINT('Ctrl Pts',(-0.199179703927896,0.0122617568640769,
-0.00879700974463651));
#38425=CARTESIAN_POINT('Ctrl Pts',(-0.199143204201,0.0120247611072695,-0.00893759561857762));
#38426=CARTESIAN_POINT('Ctrl Pts',(-0.199097939428168,0.0117088168372167,
-0.00910488168002557));
#38427=CARTESIAN_POINT('Ctrl Pts',(-0.199053503138609,0.0113512026808426,
-0.0092722473869251));
#38428=CARTESIAN_POINT('Ctrl Pts',(-0.199033293522739,0.0111741545475986,
-0.00935061960017856));
#38429=CARTESIAN_POINT('Ctrl Pts',(-0.199005137616745,0.0108610682528071,
-0.00947879250595618));
#38430=CARTESIAN_POINT('Ctrl Pts',(-0.198981346397536,0.0104828930260802,
-0.00961764034004101));
#38431=CARTESIAN_POINT('Ctrl Pts',(-0.198966676100586,0.00995915763679357,
-0.00978057905748434));
#38432=CARTESIAN_POINT('Ctrl Pts',(-0.198973041715815,0.00949846961319302,
-0.00989171088830268));
#38433=CARTESIAN_POINT('Ctrl Pts',(-0.198986847549745,0.00912555823936307,
-0.00996303926878747));
#38434=CARTESIAN_POINT('Ctrl Pts',(-0.198996951253955,0.00891696971379377,
-0.0099974514904745));
#38435=CARTESIAN_POINT('Ctrl Pts',(-0.199007563060688,0.00873019692801794,
-0.0100243178043377));
#38436=CARTESIAN_POINT('Ctrl Pts',(-0.199013193043944,0.00864186587218177,
-0.0100355847905736));
#38437=CARTESIAN_POINT('Ctrl Pts',(-0.199024702404667,0.00846869292596894,
-0.0100562817337783));
#38438=CARTESIAN_POINT('Ctrl Pts',(-0.199048566807395,0.00813984594312779,
-0.0100882617902053));
#38439=CARTESIAN_POINT('Ctrl Pts',(-0.199077674466065,0.00777604990432176,
-0.0101071872672199));
#38440=CARTESIAN_POINT('Ctrl Pts',(-0.199100855518735,0.00750164301569709,
-0.0101077379539484));
#38441=CARTESIAN_POINT('',(-0.199174890168764,0.00274277102513258,-0.00879960252067264));
#38442=CARTESIAN_POINT('Ctrl Pts',(-0.199100855499581,0.00750164279111966,
-0.010107737953573));
#38443=CARTESIAN_POINT('Ctrl Pts',(-0.199096512842791,0.0074507254531517,
-0.0101076528529768));
#38444=CARTESIAN_POINT('Ctrl Pts',(-0.199083134658093,0.0072923247860624,
-0.0101058783397399));
#38445=CARTESIAN_POINT('Ctrl Pts',(-0.199063642168381,0.0070548680736872,
-0.010097459801595));
#38446=CARTESIAN_POINT('Ctrl Pts',(-0.199040944663942,0.00676685079174908,
-0.0100792908277045));
#38447=CARTESIAN_POINT('Ctrl Pts',(-0.199023857146907,0.00653361641306146,
-0.0100564833735876));
#38448=CARTESIAN_POINT('Ctrl Pts',(-0.199012188872024,0.00636007042461428,
-0.0100358089039185));
#38449=CARTESIAN_POINT('Ctrl Pts',(-0.199006474143519,0.0062713629778719,
-0.010024496770625));
#38450=CARTESIAN_POINT('Ctrl Pts',(-0.19899579505426,0.00608569538297935,
-0.00999783233827452));
#38451=CARTESIAN_POINT('Ctrl Pts',(-0.198985535474748,0.00587698222152784,
-0.00996346271303501));
#38452=CARTESIAN_POINT('Ctrl Pts',(-0.198971489215569,0.00550454656573253,
-0.00989233175470144));
#38453=CARTESIAN_POINT('Ctrl Pts',(-0.198964807417977,0.0050434817823875,
-0.0097812491317302));
#38454=CARTESIAN_POINT('Ctrl Pts',(-0.198979069999859,0.00452083414037976,
-0.00961883927653868));
#38455=CARTESIAN_POINT('Ctrl Pts',(-0.199002513849818,0.0041425196065762,
-0.00948013203005093));
#38456=CARTESIAN_POINT('Ctrl Pts',(-0.199030389517277,0.00382879040644363,
-0.0093518231363092));
#38457=CARTESIAN_POINT('Ctrl Pts',(-0.19905031989914,0.00365219450905632,
-0.00927371564898574));
#38458=CARTESIAN_POINT('Ctrl Pts',(-0.199094175364824,0.00329507035401741,
-0.00910675653462751));
#38459=CARTESIAN_POINT('Ctrl Pts',(-0.199138855829589,0.00297952240380151,
-0.00893987067691832));
#38460=CARTESIAN_POINT('Ctrl Pts',(-0.199174890168764,0.00274277102513258,
-0.00879960252067264));
#38461=CARTESIAN_POINT('',(-0.200176298967052,0.00274312284324985,-0.00882151165036355));
#38462=CARTESIAN_POINT('Ctrl Pts',(-0.199174978504506,0.0027427741926983,
-0.00879960632195548));
#38463=CARTESIAN_POINT('Ctrl Pts',(-0.199508744817405,0.00274289029024272,
-0.00880690787508466));
#38464=CARTESIAN_POINT('Ctrl Pts',(-0.199842609566303,0.00274300207072459,
-0.00881420898572931));
#38465=CARTESIAN_POINT('Ctrl Pts',(-0.200176363703368,0.00274310946256466,
-0.00882150508214149));
#38466=CARTESIAN_POINT('',(-0.200100346793384,0.007501072560866,-0.0101293929847466));
#38467=CARTESIAN_POINT('Ctrl Pts',(-0.200176298967052,0.00274312284324985,
-0.00882151165036355));
#38468=CARTESIAN_POINT('Ctrl Pts',(-0.200139901624223,0.00298111288128331,
-0.00896249548311666));
#38469=CARTESIAN_POINT('Ctrl Pts',(-0.200094776359582,0.0032984278604287,
-0.00913017620506027));
#38470=CARTESIAN_POINT('Ctrl Pts',(-0.200050546122483,0.00365715840436292,
-0.00929766342399987));
#38471=CARTESIAN_POINT('Ctrl Pts',(-0.20003039577123,0.0038354058170338,
-0.00937632392915631));
#38472=CARTESIAN_POINT('Ctrl Pts',(-0.200002621185558,0.00414711815629604,
-0.00950355721699447));
#38473=CARTESIAN_POINT('Ctrl Pts',(-0.199979106616714,0.00452386327719561,
-0.00964148519218933));
#38474=CARTESIAN_POINT('Ctrl Pts',(-0.199964614173862,0.00504258778238135,
-0.00980260694896718));
#38475=CARTESIAN_POINT('Ctrl Pts',(-0.199970998844043,0.00550380760441275,
-0.00991381891727839));
#38476=CARTESIAN_POINT('Ctrl Pts',(-0.199984884909593,0.0058751987753087,
-0.00998479074790535));
#38477=CARTESIAN_POINT('Ctrl Pts',(-0.199995051830887,0.00608317809692423,
-0.0100190916632865));
#38478=CARTESIAN_POINT('Ctrl Pts',(-0.200005680160915,0.00626858618305641,
-0.0100457782626161));
#38479=CARTESIAN_POINT('Ctrl Pts',(-0.200011403384908,0.00635753841527696,
-0.0100571356838335));
#38480=CARTESIAN_POINT('Ctrl Pts',(-0.200023028068371,0.00653068785947513,
-0.0100778720223878));
#38481=CARTESIAN_POINT('Ctrl Pts',(-0.200040486090422,0.00676818059405957,
-0.0101007806890797));
#38482=CARTESIAN_POINT('Ctrl Pts',(-0.200066404696961,0.00709789506032636,
-0.010122648472979));
#38483=CARTESIAN_POINT('Ctrl Pts',(-0.200089885580134,0.00737871281159999,
-0.0101291804881323));
#38484=CARTESIAN_POINT('Ctrl Pts',(-0.200100346789817,0.00750107229631922,
-0.0101293929847));
#38485=CARTESIAN_POINT('',(-0.200180012158742,0.0122615324625992,-0.00881881320672816));
#38486=CARTESIAN_POINT('Ctrl Pts',(-0.200100346793384,0.007501072560866,
-0.0101293929847466));
#38487=CARTESIAN_POINT('Ctrl Pts',(-0.200077032371193,0.00777702625121947,
-0.0101288559212946));
#38488=CARTESIAN_POINT('Ctrl Pts',(-0.200047785351717,0.00814269793645221,
-0.0101097531678741));
#38489=CARTESIAN_POINT('Ctrl Pts',(-0.200023842556866,0.00847317582369828,
-0.0100774615819148));
#38490=CARTESIAN_POINT('Ctrl Pts',(-0.20001233035194,0.00864685470632593,
-0.0100566165239891));
#38491=CARTESIAN_POINT('Ctrl Pts',(-0.200006668220042,0.00873609402904403,
-0.0100451709625597));
#38492=CARTESIAN_POINT('Ctrl Pts',(-0.199996202196605,0.00892127235517656,
-0.0100184260680742));
#38493=CARTESIAN_POINT('Ctrl Pts',(-0.199986209497443,0.00912871922182942,
-0.00998411851683095));
#38494=CARTESIAN_POINT('Ctrl Pts',(-0.199972585062777,0.00949940521822475,
-0.00991311283795994));
#38495=CARTESIAN_POINT('Ctrl Pts',(-0.199966337977404,0.00995807776149586,
-0.00980246973164739));
#38496=CARTESIAN_POINT('Ctrl Pts',(-0.199980974423784,0.0104794470890044,
-0.00964043514661892));
#38497=CARTESIAN_POINT('Ctrl Pts',(-0.200004693306816,0.01085647907637,
-0.00950220593946975));
#38498=CARTESIAN_POINT('Ctrl Pts',(-0.200032664319952,0.0111681667330681,
-0.0093748392791198));
#38499=CARTESIAN_POINT('Ctrl Pts',(-0.200052998452224,0.0113465907494263,
-0.00929601341129254));
#38500=CARTESIAN_POINT('Ctrl Pts',(-0.200097650391265,0.0117056249071542,
-0.00912819209771724));
#38501=CARTESIAN_POINT('Ctrl Pts',(-0.200143236687151,0.0120232851406314,
-0.00896013083810101));
#38502=CARTESIAN_POINT('Ctrl Pts',(-0.200180012158742,0.0122615324625992,
-0.00881881320672816));
#38503=CARTESIAN_POINT('Ctrl Pts',(-0.200180079025303,0.0122615411987862,
-0.00881880944411998));
#38504=CARTESIAN_POINT('Ctrl Pts',(-0.199847188917382,0.0122616093237988,
-0.0088115574338891));
#38505=CARTESIAN_POINT('Ctrl Pts',(-0.199513665157781,0.0122616817788384,
-0.0088042891129262));
#38506=CARTESIAN_POINT('Ctrl Pts',(-0.199179794132942,0.012261758536906,
-0.00879701070083819));
#38507=CARTESIAN_POINT('Origin',(-0.197568936813702,0.0075000008565567,
-0.000739278552754604));
#38508=CARTESIAN_POINT('',(-0.197178898213844,0.0122639308527257,-0.00875621776386257));
#38509=CARTESIAN_POINT('',(-0.197101863217746,0.00750262246797567,-0.0100625703404307));
#38510=CARTESIAN_POINT('Ctrl Pts',(-0.197178898213844,0.0122639308527257,
-0.00875621776386257));
#38511=CARTESIAN_POINT('Ctrl Pts',(-0.19714259372659,0.0120266476840343,
-0.00889635098469014));
#38512=CARTESIAN_POINT('Ctrl Pts',(-0.197097579703726,0.0117104025483866,
-0.00906308102871975));
#38513=CARTESIAN_POINT('Ctrl Pts',(-0.197053415857518,0.0113525637018549,
-0.00922986495999574));
#38514=CARTESIAN_POINT('Ctrl Pts',(-0.197033337579018,0.0111754135137217,
-0.00930796486082764));
#38515=CARTESIAN_POINT('Ctrl Pts',(-0.197005409642325,0.0108623084455755,
-0.00943564106288338));
#38516=CARTESIAN_POINT('Ctrl Pts',(-0.196981851559973,0.0104840536183527,
-0.00957399630291121));
#38517=CARTESIAN_POINT('Ctrl Pts',(-0.196967442586391,0.00995994453949125,
-0.00973644770686073));
#38518=CARTESIAN_POINT('Ctrl Pts',(-0.196973960238896,0.00949949430987693,
-0.00984713249190998));
#38519=CARTESIAN_POINT('Ctrl Pts',(-0.196987841285996,0.00912652089145974,
-0.00991824315734064));
#38520=CARTESIAN_POINT('Ctrl Pts',(-0.196997975177209,0.00891789605014179,
-0.00995255254822396));
#38521=CARTESIAN_POINT('Ctrl Pts',(-0.197008607375973,0.00873105355572069,
-0.00997934580045198));
#38522=CARTESIAN_POINT('Ctrl Pts',(-0.197014240119431,0.00864274709212368,
-0.0099905753992407));
#38523=CARTESIAN_POINT('Ctrl Pts',(-0.197025754698584,0.00846957756916279,
-0.0100112112482997));
#38524=CARTESIAN_POINT('Ctrl Pts',(-0.197049615978027,0.00814075996848684,
-0.0100431010647813));
#38525=CARTESIAN_POINT('Ctrl Pts',(-0.197078704301286,0.0077770004044274,
-0.0100619918809788));
#38526=CARTESIAN_POINT('Ctrl Pts',(-0.19710186371798,0.00750262251022666,
-0.0100625703535652));
#38527=CARTESIAN_POINT('',(-0.19717625942921,0.00274085336740581,-0.00875899754539223));
#38528=CARTESIAN_POINT('Ctrl Pts',(-0.197101863740693,0.0075026222411284,
-0.0100625703541326));
#38529=CARTESIAN_POINT('Ctrl Pts',(-0.19710000820331,0.00748080937071407,
-0.0100625363069147));
#38530=CARTESIAN_POINT('Ctrl Pts',(-0.197092850772113,0.00739629281398418,
-0.0100620378586211));
#38531=CARTESIAN_POINT('Ctrl Pts',(-0.197082572289835,0.0072731864579776,
-0.010059714804392));
#38532=CARTESIAN_POINT('Ctrl Pts',(-0.197064196962725,0.00704941232229019,
-0.0100523810870764));
#38533=CARTESIAN_POINT('Ctrl Pts',(-0.197042298317003,0.00677016330244297,
-0.0100343141173027));
#38534=CARTESIAN_POINT('Ctrl Pts',(-0.197025003299601,0.00653407818619356,
-0.0100115858250691));
#38535=CARTESIAN_POINT('Ctrl Pts',(-0.197013366326264,0.0063606929252265,
-0.00999098123439524));
#38536=CARTESIAN_POINT('Ctrl Pts',(-0.197007634588523,0.00627164901858326,
-0.00997967976748478));
#38537=CARTESIAN_POINT('Ctrl Pts',(-0.196996967220652,0.00608618549516388,
-0.00995315170376989));
#38538=CARTESIAN_POINT('Ctrl Pts',(-0.196986666483152,0.00587700992513145,
-0.00991884864512528));
#38539=CARTESIAN_POINT('Ctrl Pts',(-0.196972560336713,0.00550427978223037,
-0.0098479158597966));
#38540=CARTESIAN_POINT('Ctrl Pts',(-0.196965721899109,0.00504399465872652,
-0.00973747933000136));
#38541=CARTESIAN_POINT('Ctrl Pts',(-0.196979841087771,0.00452005502685437,
-0.00957533456267068));
#38542=CARTESIAN_POINT('Ctrl Pts',(-0.197003260603367,0.0041416367207074,
-0.0094371187180398));
#38543=CARTESIAN_POINT('Ctrl Pts',(-0.197031131766291,0.00382819529897539,
-0.00930946168380616));
#38544=CARTESIAN_POINT('Ctrl Pts',(-0.19705114822033,0.00365125562861138,
-0.00923153950398635));
#38545=CARTESIAN_POINT('Ctrl Pts',(-0.197095163150635,0.0032939066678421,
-0.00906518924055637));
#38546=CARTESIAN_POINT('Ctrl Pts',(-0.197140051657865,0.00297795351737253,
-0.00889883295406792));
#38547=CARTESIAN_POINT('Ctrl Pts',(-0.19717625942921,0.00274085336740581,
-0.00875899754539223));
#38548=CARTESIAN_POINT('',(-0.198174032768987,0.00274096783991525,-0.00878067084834629));
#38549=CARTESIAN_POINT('Ctrl Pts',(-0.1971763502326,0.00274085635926309,
-0.00875900128602603));
#38550=CARTESIAN_POINT('Ctrl Pts',(-0.197510802105109,0.00274089373748812,
-0.00876626555074249));
#38551=CARTESIAN_POINT('Ctrl Pts',(-0.197843551375065,0.00274092638819502,
-0.0087734901437584));
#38552=CARTESIAN_POINT('Ctrl Pts',(-0.198174097223676,0.00274095441811271,
-0.00878066428407293));
#38553=CARTESIAN_POINT('',(-0.198101361533896,0.00750214622993516,-0.0100842099593931));
#38554=CARTESIAN_POINT('Ctrl Pts',(-0.198174032768987,0.00274096783991525,
-0.00878067084834629));
#38555=CARTESIAN_POINT('Ctrl Pts',(-0.198138061322491,0.00297936807682186,
-0.0089212776129119));
#38556=CARTESIAN_POINT('Ctrl Pts',(-0.198093477108618,0.00329714613090043,
-0.00908848214951006));
#38557=CARTESIAN_POINT('Ctrl Pts',(-0.198049811215033,0.0036562864094438,
-0.00925545767808787));
#38558=CARTESIAN_POINT('Ctrl Pts',(-0.198029930114142,0.00383470369580787,
-0.00933386550169443));
#38559=CARTESIAN_POINT('Ctrl Pts',(-0.198002573654122,0.00414664354364956,
-0.00946066872251577));
#38560=CARTESIAN_POINT('Ctrl Pts',(-0.197979478111198,0.00452366787372502,
-0.00959814161153211));
#38561=CARTESIAN_POINT('Ctrl Pts',(-0.19796541505455,0.0050428957774833,
-0.00975876511200693));
#38562=CARTESIAN_POINT('Ctrl Pts',(-0.197972019492495,0.0055041999955818,
-0.00986953619272144));
#38563=CARTESIAN_POINT('Ctrl Pts',(-0.197985992896418,0.00587566481187643,
-0.00994023559640718));
#38564=CARTESIAN_POINT('Ctrl Pts',(-0.197996197119194,0.00608385240141643,
-0.00997442519451085));
#38565=CARTESIAN_POINT('Ctrl Pts',(-0.198006815342193,0.00626894970105581,
-0.0100009515703469));
#38566=CARTESIAN_POINT('Ctrl Pts',(-0.198012537979335,0.00635797677696961,
-0.0100122864200635));
#38567=CARTESIAN_POINT('Ctrl Pts',(-0.198024203479145,0.00653171972941347,
-0.0100329456666756));
#38568=CARTESIAN_POINT('Ctrl Pts',(-0.198041324115801,0.00676561835599725,
-0.010055764848873));
#38569=CARTESIAN_POINT('Ctrl Pts',(-0.198064034153434,0.00705384034717996,
-0.0100739406522062));
#38570=CARTESIAN_POINT('Ctrl Pts',(-0.198083644772806,0.00729297247666229,
-0.010082361311082));
#38571=CARTESIAN_POINT('Ctrl Pts',(-0.198096918465339,0.00744974375587924,
-0.0100841258368541));
#38572=CARTESIAN_POINT('Ctrl Pts',(-0.198101361530205,0.00750214596208306,
-0.0100842099593748));
#38573=CARTESIAN_POINT('',(-0.198179287823527,0.0122637027296793,-0.00877800875605197));
#38574=CARTESIAN_POINT('Ctrl Pts',(-0.198101361533896,0.00750214622993515,
-0.0100842099593931));
#38575=CARTESIAN_POINT('Ctrl Pts',(-0.198078064760131,0.00777806953424965,
-0.0100836420027939));
#38576=CARTESIAN_POINT('Ctrl Pts',(-0.198048832502402,0.00814370089079693,
-0.0100645708158547));
#38577=CARTESIAN_POINT('Ctrl Pts',(-0.198024889911693,0.00847414328964963,
-0.010032367938066));
#38578=CARTESIAN_POINT('Ctrl Pts',(-0.198013371582161,0.00864781364955267,
-0.0100115835738566));
#38579=CARTESIAN_POINT('Ctrl Pts',(-0.19800770620434,0.00873702690890067,
-0.0100001753830021));
#38580=CARTESIAN_POINT('Ctrl Pts',(-0.197997220260069,0.00892226298464491,
-0.00997350350283401));
#38581=CARTESIAN_POINT('Ctrl Pts',(-0.197987198570751,0.0091297389651211,
-0.00993929825390304));
#38582=CARTESIAN_POINT('Ctrl Pts',(-0.197973502881743,0.009500474943299,
-0.00986851018274228));
#38583=CARTESIAN_POINT('Ctrl Pts',(-0.197967115435973,0.00995897304118631,
-0.00975829178770248));
#38584=CARTESIAN_POINT('Ctrl Pts',(-0.197981507135243,0.0104806097246969,
-0.00959676986039016));
#38585=CARTESIAN_POINT('Ctrl Pts',(-0.198005003872498,0.0108576989128222,
-0.00945904051216777));
#38586=CARTESIAN_POINT('Ctrl Pts',(-0.198032755894909,0.0111693872661804,
-0.00933217581919596));
#38587=CARTESIAN_POINT('Ctrl Pts',(-0.19805296392532,0.011347923686061,
-0.00925362054200033));
#38588=CARTESIAN_POINT('Ctrl Pts',(-0.198097354270813,0.0117071893600477,
-0.0090863808984517));
#38589=CARTESIAN_POINT('Ctrl Pts',(-0.198142699816937,0.0120251604527111,
-0.00891887465281153));
#38590=CARTESIAN_POINT('Ctrl Pts',(-0.198179287823527,0.0122637027296793,
-0.00877800875605197));
#38591=CARTESIAN_POINT('Ctrl Pts',(-0.198179354943918,0.0122637115781413,
-0.00877800495436216));
#38592=CARTESIAN_POINT('Ctrl Pts',(-0.197846468878006,0.0122637807574249,
-0.00877075785975849));
#38593=CARTESIAN_POINT('Ctrl Pts',(-0.197512916440007,0.0122638544198246,
-0.00876349367670277));
#38594=CARTESIAN_POINT('Ctrl Pts',(-0.197178988840092,0.0122639325398186,
-0.00875621872371576));
#38595=CARTESIAN_POINT('Origin',(-0.195568817432697,0.00750000072543657,
-0.000658346566684942));
#38596=CARTESIAN_POINT('',(-0.195178104730999,0.0122657318419193,-0.00871574250981778));
#38597=CARTESIAN_POINT('',(-0.195102858686147,0.00750349572610613,-0.0100174023059187));
#38598=CARTESIAN_POINT('Ctrl Pts',(-0.195178104730999,0.0122657318419193,
-0.00871574250981778));
#38599=CARTESIAN_POINT('Ctrl Pts',(-0.195141971850056,0.0120281695201214,
-0.00885539096701177));
#38600=CARTESIAN_POINT('Ctrl Pts',(-0.195097177150193,0.0117116408727372,
-0.00902152489589311));
#38601=CARTESIAN_POINT('Ctrl Pts',(-0.195053245825187,0.011353580518071,
-0.00918769379669155));
#38602=CARTESIAN_POINT('Ctrl Pts',(-0.195033282223062,0.0111763704209235,
-0.00926548967369924));
#38603=CARTESIAN_POINT('Ctrl Pts',(-0.195005529791546,0.0108631259821725,
-0.00939269413058469));
#38604=CARTESIAN_POINT('Ctrl Pts',(-0.194982154210136,0.0104847570855313,
-0.00953053190643839));
#38605=CARTESIAN_POINT('Ctrl Pts',(-0.194967940414644,0.00996059210314794,
-0.00969237054229474));
#38606=CARTESIAN_POINT('Ctrl Pts',(-0.194974581042148,0.00950004130325584,
-0.00980266786669539));
#38607=CARTESIAN_POINT('Ctrl Pts',(-0.194988548178529,0.00912711026305177,
-0.0098735158134373));
#38608=CARTESIAN_POINT('Ctrl Pts',(-0.194998725529187,0.00891852251849867,
-0.00990770057596708));
#38609=CARTESIAN_POINT('Ctrl Pts',(-0.195009393305373,0.00873173227665468,
-0.00993439713830365));
#38610=CARTESIAN_POINT('Ctrl Pts',(-0.195015042871648,0.00864343621680832,
-0.00994558943115054));
#38611=CARTESIAN_POINT('Ctrl Pts',(-0.195026589264483,0.00847029750149345,
-0.00996615649178523));
#38612=CARTESIAN_POINT('Ctrl Pts',(-0.19505050856113,0.00814153252125014,
-0.00999794766159865));
#38613=CARTESIAN_POINT('Ctrl Pts',(-0.195079656832268,0.00777783275067516,
-0.010016797998545));
#38614=CARTESIAN_POINT('Ctrl Pts',(-0.195102859197629,0.00750349576939646,
-0.0100174023200885));
#38615=CARTESIAN_POINT('',(-0.19517797993867,0.00273809386567736,-0.00871799806561756));
#38616=CARTESIAN_POINT('Ctrl Pts',(-0.195102859215766,0.00750349555493702,
-0.0100174023205609));
#38617=CARTESIAN_POINT('Ctrl Pts',(-0.195100949641578,0.00748091060552787,
-0.0100173694335902));
#38618=CARTESIAN_POINT('Ctrl Pts',(-0.195093941673867,0.00739765059757744,
-0.0100168843546768));
#38619=CARTESIAN_POINT('Ctrl Pts',(-0.195083666814497,0.00727384426413517,
-0.0100145806517102));
#38620=CARTESIAN_POINT('Ctrl Pts',(-0.195065427890217,0.00705034028650716,
-0.0100072931400613));
#38621=CARTESIAN_POINT('Ctrl Pts',(-0.195043635768285,0.00677069706287903,
-0.00998930677462411));
#38622=CARTESIAN_POINT('Ctrl Pts',(-0.195026446133143,0.00653446921995725,
-0.00996665842637773));
#38623=CARTESIAN_POINT('Ctrl Pts',(-0.195014882614189,0.00636097407782196,
-0.00994612972574996));
#38624=CARTESIAN_POINT('Ctrl Pts',(-0.19500917675081,0.00627167458992341,
-0.00993483859680917));
#38625=CARTESIAN_POINT('Ctrl Pts',(-0.194998616244289,0.00608664200750535,
-0.00990848143429438));
#38626=CARTESIAN_POINT('Ctrl Pts',(-0.194988392779268,0.00587728921639411,
-0.00987429706439239));
#38627=CARTESIAN_POINT('Ctrl Pts',(-0.194974428076451,0.00550449240298873,
-0.00980364228685664));
#38628=CARTESIAN_POINT('Ctrl Pts',(-0.194967724982329,0.00504366300959344,
-0.00969353647290735));
#38629=CARTESIAN_POINT('Ctrl Pts',(-0.194981896216006,0.00451896128129825,
-0.00953177976677903));
#38630=CARTESIAN_POINT('Ctrl Pts',(-0.195005276822889,0.00414029348230681,
-0.00939400313637884));
#38631=CARTESIAN_POINT('Ctrl Pts',(-0.195033051886066,0.00382690893110969,
-0.00926688245348259));
#38632=CARTESIAN_POINT('Ctrl Pts',(-0.195053038245836,0.00364968132354558,
-0.00918915665886015));
#38633=CARTESIAN_POINT('Ctrl Pts',(-0.19509697568046,0.00329201079149359,
-0.00902334424493648));
#38634=CARTESIAN_POINT('Ctrl Pts',(-0.195141810958693,0.00297559470165675,
-0.00885745735339972));
#38635=CARTESIAN_POINT('Ctrl Pts',(-0.19517797993867,0.00273809386567736,
-0.00871799806561756));
#38636=CARTESIAN_POINT('',(-0.196177537013878,0.00273881078232022,-0.00874004887933647));
#38637=CARTESIAN_POINT('Ctrl Pts',(-0.195178071596977,0.00273809719998608,
-0.00871800201771347));
#38638=CARTESIAN_POINT('Ctrl Pts',(-0.195511220445504,0.00273833506685321,
-0.00872535085344679));
#38639=CARTESIAN_POINT('Ctrl Pts',(-0.195844467515233,0.00273856839192212,
-0.00873269911814646));
#38640=CARTESIAN_POINT('Ctrl Pts',(-0.196177604968697,0.00273879702797085,
-0.00874004222951915));
#38641=CARTESIAN_POINT('',(-0.196102482808628,0.0075031283040999,-0.0100390287523791));
#38642=CARTESIAN_POINT('Ctrl Pts',(-0.196177537013878,0.00273881078232022,
-0.00874004887933647));
#38643=CARTESIAN_POINT('Ctrl Pts',(-0.196141077813662,0.002977546954655,
-0.00888020254352069));
#38644=CARTESIAN_POINT('Ctrl Pts',(-0.1960958943586,0.003295720706571,-0.00904686057463413));
#38645=CARTESIAN_POINT('Ctrl Pts',(-0.196051682528282,0.00365512641323152,
-0.00921323603776369));
#38646=CARTESIAN_POINT('Ctrl Pts',(-0.196031544479116,0.00383389049984808,
-0.00929145057678427));
#38647=CARTESIAN_POINT('Ctrl Pts',(-0.196003981018244,0.0041452785571844,
-0.00941749978987608));
#38648=CARTESIAN_POINT('Ctrl Pts',(-0.195980695863156,0.00452230528419756,
-0.0095544680877062));
#38649=CARTESIAN_POINT('Ctrl Pts',(-0.195966579506683,0.00504344712837199,
-0.00971501996119166));
#38650=CARTESIAN_POINT('Ctrl Pts',(-0.19597325975956,0.00550360409286807,
-0.0098250504480127));
#38651=CARTESIAN_POINT('Ctrl Pts',(-0.195987256853935,0.00587551587646132,
-0.00989558612950375));
#38652=CARTESIAN_POINT('Ctrl Pts',(-0.195997482940324,0.00608413149667644,
-0.00992970850098842));
#38653=CARTESIAN_POINT('Ctrl Pts',(-0.196008100881894,0.0062693916013721,
-0.00995614659231545));
#38654=CARTESIAN_POINT('Ctrl Pts',(-0.196013821361637,0.00635852739556059,
-0.00996744984550979));
#38655=CARTESIAN_POINT('Ctrl Pts',(-0.196025488473502,0.00653255950142857,
-0.00998803747009445));
#38656=CARTESIAN_POINT('Ctrl Pts',(-0.19604251164246,0.00676571709900968,
-0.0100107659233449));
#38657=CARTESIAN_POINT('Ctrl Pts',(-0.196070031707032,0.00711557397662451,
-0.0100324670854736));
#38658=CARTESIAN_POINT('Ctrl Pts',(-0.196089303496893,0.00734820057878708,
-0.0100387954224435));
#38659=CARTESIAN_POINT('Ctrl Pts',(-0.196102482808628,0.0075031283040999,
-0.0100390287523791));
#38660=CARTESIAN_POINT('',(-0.196178484195762,0.0122657643255281,-0.00873736329835759));
#38661=CARTESIAN_POINT('Ctrl Pts',(-0.196102482807571,0.00750312859925915,
-0.0100390287522575));
#38662=CARTESIAN_POINT('Ctrl Pts',(-0.196079156242257,0.00777902017568519,
-0.0100384318480314));
#38663=CARTESIAN_POINT('Ctrl Pts',(-0.196049879511574,0.00814460596841201,
-0.0100193964106389));
#38664=CARTESIAN_POINT('Ctrl Pts',(-0.196025889608579,0.00847500825680877,
-0.00998728738456208));
#38665=CARTESIAN_POINT('Ctrl Pts',(-0.196014343371659,0.00864865962912956,
-0.00996656810576789));
#38666=CARTESIAN_POINT('Ctrl Pts',(-0.196008663300801,0.00873785767352454,
-0.00995519720228832));
#38667=CARTESIAN_POINT('Ctrl Pts',(-0.195998141861114,0.00892308850487265,
-0.00992861152525066));
#38668=CARTESIAN_POINT('Ctrl Pts',(-0.195988075859801,0.00913055848064588,
-0.00989452055980878));
#38669=CARTESIAN_POINT('Ctrl Pts',(-0.195974288909848,0.00950129545777585,
-0.00982397494050396));
#38670=CARTESIAN_POINT('Ctrl Pts',(-0.195967760794256,0.00995982623587528,
-0.00971414472348679));
#38671=CARTESIAN_POINT('Ctrl Pts',(-0.195981926030902,0.0104815441926318,
-0.00955321072493732));
#38672=CARTESIAN_POINT('Ctrl Pts',(-0.196005215231541,0.0108587298290495,
-0.00941599040482433));
#38673=CARTESIAN_POINT('Ctrl Pts',(-0.196032767263529,0.0111705199455354,
-0.00928960083841346));
#38674=CARTESIAN_POINT('Ctrl Pts',(-0.196052849549526,0.0113491432795003,
-0.00921133497787415));
#38675=CARTESIAN_POINT('Ctrl Pts',(-0.196096982103339,0.0117086492359856,
-0.00904469186630159));
#38676=CARTESIAN_POINT('Ctrl Pts',(-0.196142085551053,0.0120269270976718,
-0.00887776111976833));
#38677=CARTESIAN_POINT('Ctrl Pts',(-0.196178484195762,0.0122657643255281,
-0.00873736329835759));
#38678=CARTESIAN_POINT('Ctrl Pts',(-0.196178551300409,0.012265773450217,
-0.00873735935601521));
#38679=CARTESIAN_POINT('Ctrl Pts',(-0.195841577142587,0.0122657554214599,
-0.00873008066191514));
#38680=CARTESIAN_POINT('Ctrl Pts',(-0.195507874037976,0.0122657421970718,
-0.00872286988639498));
#38681=CARTESIAN_POINT('Ctrl Pts',(-0.195178195187604,0.0122657335081665,
-0.00871574348158736));
#38682=CARTESIAN_POINT('Origin',(-0.221676249214976,0.00750000345182045,
-0.0016541350256873));
#38683=CARTESIAN_POINT('',(-0.221393352906395,0.0131398835301861,-0.00861356300121323));
#38684=CARTESIAN_POINT('',(-0.22109337191764,0.00750288941767847,-0.0106049432732665));
#38685=CARTESIAN_POINT('Ctrl Pts',(-0.221393352906395,0.0131398835301861,
-0.00861356300121323));
#38686=CARTESIAN_POINT('Ctrl Pts',(-0.221320888392813,0.0128815572458935,
-0.00882126869267544));
#38687=CARTESIAN_POINT('Ctrl Pts',(-0.221231380503492,0.01252852322136,
-0.00907134596473989));
#38688=CARTESIAN_POINT('Ctrl Pts',(-0.221145875567908,0.012125092174896,
-0.00932172732914744));
#38689=CARTESIAN_POINT('Ctrl Pts',(-0.221106505058042,0.0119112831655975,
-0.00944594135167501));
#38690=CARTESIAN_POINT('Ctrl Pts',(-0.221059952440027,0.0115846277870923,
-0.00962205237725879));
#38691=CARTESIAN_POINT('Ctrl Pts',(-0.221025069259206,0.0112550786873381,
-0.00978133219115847));
#38692=CARTESIAN_POINT('Ctrl Pts',(-0.220997005450521,0.0108970649444057,
-0.00993743190236953));
#38693=CARTESIAN_POINT('Ctrl Pts',(-0.220969865667947,0.0103669261135731,
-0.0101389726762554));
#38694=CARTESIAN_POINT('Ctrl Pts',(-0.220961462009027,0.00989275498375296,
-0.0102831873771524));
#38695=CARTESIAN_POINT('Ctrl Pts',(-0.22096744629676,0.00945353568132999,
-0.0103881570799034));
#38696=CARTESIAN_POINT('Ctrl Pts',(-0.220974504485159,0.00921313446131081,
-0.0104378830236523));
#38697=CARTESIAN_POINT('Ctrl Pts',(-0.220982990015517,0.00900856730165844,
-0.0104751602785334));
#38698=CARTESIAN_POINT('Ctrl Pts',(-0.220988827061368,0.00889688919602636,
-0.0104934052387218));
#38699=CARTESIAN_POINT('Ctrl Pts',(-0.221000849071749,0.00868900886590427,
-0.0105249286429414));
#38700=CARTESIAN_POINT('Ctrl Pts',(-0.221028102523713,0.00828742369692355,
-0.0105746853659743));
#38701=CARTESIAN_POINT('Ctrl Pts',(-0.221063893512024,0.00784105280531206,
-0.0106042019791774));
#38702=CARTESIAN_POINT('Ctrl Pts',(-0.22109337191764,0.00750288941767847,
-0.0106049432732665));
#38703=CARTESIAN_POINT('',(-0.22139902998639,0.00187359712117749,-0.00862457485406049));
#38704=CARTESIAN_POINT('Ctrl Pts',(-0.221093371849766,0.00750288863438198,
-0.0106049432720617));
#38705=CARTESIAN_POINT('Ctrl Pts',(-0.221091363881298,0.0074797159479151,
-0.0106049076271627));
#38706=CARTESIAN_POINT('Ctrl Pts',(-0.22108194961028,0.0073703646997039,
-0.0106041605834244));
#38707=CARTESIAN_POINT('Ctrl Pts',(-0.221069464690532,0.0072219193189083,
-0.0106005848012409));
#38708=CARTESIAN_POINT('Ctrl Pts',(-0.221046833823411,0.00694579229382263,
-0.0105891976872885));
#38709=CARTESIAN_POINT('Ctrl Pts',(-0.221021019951164,0.00660573000945973,
-0.0105611718773493));
#38710=CARTESIAN_POINT('Ctrl Pts',(-0.221001657246536,0.00631766602399646,
-0.010525847242072));
#38711=CARTESIAN_POINT('Ctrl Pts',(-0.220989834644077,0.00611007473471422,
-0.0104945212917132));
#38712=CARTESIAN_POINT('Ctrl Pts',(-0.220984064213525,0.00599749977732925,
-0.0104762053650152));
#38713=CARTESIAN_POINT('Ctrl Pts',(-0.220975914169275,0.00579574674814498,
-0.0104396178511159));
#38714=CARTESIAN_POINT('Ctrl Pts',(-0.22096913371177,0.0055560142321091,
-0.0103903121251423));
#38715=CARTESIAN_POINT('Ctrl Pts',(-0.220963685764794,0.00511849775881586,
-0.0102862894875993));
#38716=CARTESIAN_POINT('Ctrl Pts',(-0.220972608026894,0.00464366850233373,
-0.0101426368830028));
#38717=CARTESIAN_POINT('Ctrl Pts',(-0.221000259014373,0.00411210701081089,
-0.00994124950673877));
#38718=CARTESIAN_POINT('Ctrl Pts',(-0.221028553541809,0.00375413270785835,
-0.00978563731322991));
#38719=CARTESIAN_POINT('Ctrl Pts',(-0.221063591079418,0.00342517423379665,
-0.0096270942958683));
#38720=CARTESIAN_POINT('Ctrl Pts',(-0.221110019595894,0.00310085946309852,
-0.00945283986597018));
#38721=CARTESIAN_POINT('Ctrl Pts',(-0.22114970684413,0.00288660051048064,
-0.00932883343947502));
#38722=CARTESIAN_POINT('Ctrl Pts',(-0.221235749347005,0.00248406090325365,
-0.00907988578428976));
#38723=CARTESIAN_POINT('Ctrl Pts',(-0.221325971848273,0.0021315329244801,
-0.00883112553951364));
#38724=CARTESIAN_POINT('Ctrl Pts',(-0.22139902998639,0.00187359712117749,
-0.00862457485406049));
#38725=CARTESIAN_POINT('',(-0.222398601135893,0.00187304432676294,-0.00864558975234265));
#38726=CARTESIAN_POINT('Ctrl Pts',(-0.221399020810814,0.00187359579475767,
-0.00862457358681791));
#38727=CARTESIAN_POINT('Ctrl Pts',(-0.22173220220163,0.00187341250573888,
-0.00863157915856683));
#38728=CARTESIAN_POINT('Ctrl Pts',(-0.222065458410509,0.00187322296472307,
-0.00863858128083836));
#38729=CARTESIAN_POINT('Ctrl Pts',(-0.222398585769511,0.00187302728847401,
-0.00864557567262578));
#38730=CARTESIAN_POINT('',(-0.222093147561648,0.00750348224479951,-0.010626397051749));
#38731=CARTESIAN_POINT('Ctrl Pts',(-0.222398601135893,0.00187304432676294,
-0.00864558975234265));
#38732=CARTESIAN_POINT('Ctrl Pts',(-0.222325187289336,0.00213211751554539,
-0.00885308354687082));
#38733=CARTESIAN_POINT('Ctrl Pts',(-0.222234524925318,0.00248667979231716,
-0.00910316494991973));
#38734=CARTESIAN_POINT('Ctrl Pts',(-0.222148227978173,0.00289157024373901,
-0.00935329853342097));
#38735=CARTESIAN_POINT('Ctrl Pts',(-0.222108220765584,0.00310913850090322,
-0.00947892012615623));
#38736=CARTESIAN_POINT('Ctrl Pts',(-0.222062653109278,0.00343043737402986,
-0.00965117347710931));
#38737=CARTESIAN_POINT('Ctrl Pts',(-0.222027988046481,0.00375836192166522,
-0.00980902455604343));
#38738=CARTESIAN_POINT('Ctrl Pts',(-0.222000028444215,0.00411514200078309,
-0.00996391832910129));
#38739=CARTESIAN_POINT('Ctrl Pts',(-0.221972599258432,0.00464539931558352,
-0.0101646755818894));
#38740=CARTESIAN_POINT('Ctrl Pts',(-0.221963654068083,0.00512236114675374,
-0.0103088523151418));
#38741=CARTESIAN_POINT('Ctrl Pts',(-0.221969164074096,0.00556028642479754,
-0.0104127201061691));
#38742=CARTESIAN_POINT('Ctrl Pts',(-0.221975961917538,0.00580006583214543,
-0.0104619198396024));
#38743=CARTESIAN_POINT('Ctrl Pts',(-0.221984154308948,0.00600232160969846,
-0.0104984854563983));
#38744=CARTESIAN_POINT('Ctrl Pts',(-0.221989901165274,0.00611425910628736,
-0.0105166446946959));
#38745=CARTESIAN_POINT('Ctrl Pts',(-0.222001733104974,0.00632170003362734,
-0.0105478047522586));
#38746=CARTESIAN_POINT('Ctrl Pts',(-0.222020833446452,0.00660650372540828,
-0.0105829082019461));
#38747=CARTESIAN_POINT('Ctrl Pts',(-0.222047295132714,0.00695403250001243,
-0.0106107762904338));
#38748=CARTESIAN_POINT('Ctrl Pts',(-0.222068563458765,0.00721452309948346,
-0.0106220642645268));
#38749=CARTESIAN_POINT('Ctrl Pts',(-0.222083067589409,0.00738637227386414,
-0.0106256474234903));
#38750=CARTESIAN_POINT('Ctrl Pts',(-0.222088227461813,0.0074466538080066,
-0.0106263135983161));
#38751=CARTESIAN_POINT('Ctrl Pts',(-0.222093147561648,0.00750348224479952,
-0.010626397051749));
#38752=CARTESIAN_POINT('',(-0.222392883415946,0.013140228421378,-0.00863472093570934));
#38753=CARTESIAN_POINT('Ctrl Pts',(-0.222093147723645,0.00750348411589117,
-0.0106263970544966));
#38754=CARTESIAN_POINT('Ctrl Pts',(-0.222063525278338,0.00784362482559292,
-0.0106256289212465));
#38755=CARTESIAN_POINT('Ctrl Pts',(-0.222027600061407,0.00829239003459411,
-0.0105957558053965));
#38756=CARTESIAN_POINT('Ctrl Pts',(-0.222000309884482,0.00869597776263445,
-0.0105454451755359));
#38757=CARTESIAN_POINT('Ctrl Pts',(-0.221988315815748,0.00890451403744728,
-0.010513649509377));
#38758=CARTESIAN_POINT('Ctrl Pts',(-0.221982480934348,0.00901718087153725,
-0.0104951271796541));
#38759=CARTESIAN_POINT('Ctrl Pts',(-0.221974154674737,0.00922020971833267,
-0.0104579384685322));
#38760=CARTESIAN_POINT('Ctrl Pts',(-0.221967213526053,0.00945940727173018,
-0.0104082849356463));
#38761=CARTESIAN_POINT('Ctrl Pts',(-0.221961400036284,0.00989642795779487,
-0.0103035206111078));
#38762=CARTESIAN_POINT('Ctrl Pts',(-0.2219696861429,0.010366178439211,-0.0101606719072326));
#38763=CARTESIAN_POINT('Ctrl Pts',(-0.221996852716048,0.0108978547518354,
-0.0099585837497828));
#38764=CARTESIAN_POINT('Ctrl Pts',(-0.222024978452534,0.0112563342759193,
-0.00980220541016363));
#38765=CARTESIAN_POINT('Ctrl Pts',(-0.222059941847575,0.0115864713196668,
-0.0096425809766981));
#38766=CARTESIAN_POINT('Ctrl Pts',(-0.222106718095268,0.0119142299650681,
-0.00946573442095913));
#38767=CARTESIAN_POINT('Ctrl Pts',(-0.222145979109298,0.0121272431546103,
-0.00934187162863571));
#38768=CARTESIAN_POINT('Ctrl Pts',(-0.222231340004308,0.0125300857742674,
-0.00909171780656154));
#38769=CARTESIAN_POINT('Ctrl Pts',(-0.222320615693346,0.0128823903637851,
-0.00884205736930132));
#38770=CARTESIAN_POINT('Ctrl Pts',(-0.222392883415946,0.013140228421378,
-0.00863472093570934));
#38771=CARTESIAN_POINT('Ctrl Pts',(-0.222392866266696,0.0131402404723726,
-0.00863471080482401));
#38772=CARTESIAN_POINT('Ctrl Pts',(-0.22205953122811,0.0131401160464593,
-0.00862766243819364));
#38773=CARTESIAN_POINT('Ctrl Pts',(-0.221726275997956,0.0131399976615517,
-0.00862061088319733));
#38774=CARTESIAN_POINT('Ctrl Pts',(-0.221393342167719,0.0131398853792589,
-0.00861356127303571));
#38775=CARTESIAN_POINT('Origin',(-0.219678482255905,0.00750000881799777,
-0.00158211078495795));
#38776=CARTESIAN_POINT('',(-0.219329719998599,0.0129300414290672,-0.00873877355437297));
#38777=CARTESIAN_POINT('',(-0.219093932882599,0.00750191497004506,-0.0105597757686429));
#38778=CARTESIAN_POINT('Ctrl Pts',(-0.219329719998599,0.0129300414290672,
-0.00873877355437297));
#38779=CARTESIAN_POINT('Ctrl Pts',(-0.219266758960484,0.0126760187611208,
-0.00893004940303019));
#38780=CARTESIAN_POINT('Ctrl Pts',(-0.219189106959152,0.0123307812499729,
-0.00915981955588401));
#38781=CARTESIAN_POINT('Ctrl Pts',(-0.219115186308461,0.011938067343623,
-0.00938941159033229));
#38782=CARTESIAN_POINT('Ctrl Pts',(-0.21908130994182,0.0117311055603115,
-0.00950289623249571));
#38783=CARTESIAN_POINT('Ctrl Pts',(-0.219041424917209,0.011413227212336,
-0.00966452028186231));
#38784=CARTESIAN_POINT('Ctrl Pts',(-0.219002241537353,0.0109931559754825,
-0.00985732695261662));
#38785=CARTESIAN_POINT('Ctrl Pts',(-0.218968699515465,0.0103634071969913,
-0.0101006309736288));
#38786=CARTESIAN_POINT('Ctrl Pts',(-0.218962334120046,0.00978510275003089,
-0.0102674656157249));
#38787=CARTESIAN_POINT('Ctrl Pts',(-0.218970038446411,0.00936589217437247,
-0.0103626156626804));
#38788=CARTESIAN_POINT('Ctrl Pts',(-0.218977648081212,0.00913598387302089,
-0.0104078383387266));
#38789=CARTESIAN_POINT('Ctrl Pts',(-0.218986343736269,0.0089407838193126,
-0.0104416741937123));
#38790=CARTESIAN_POINT('Ctrl Pts',(-0.218992197178124,0.00883386602501995,
-0.0104582986982075));
#38791=CARTESIAN_POINT('Ctrl Pts',(-0.219004132386565,0.00863515157903343,
-0.010486974430302));
#38792=CARTESIAN_POINT('Ctrl Pts',(-0.219030846027741,0.00825129593526508,
-0.010532248951195));
#38793=CARTESIAN_POINT('Ctrl Pts',(-0.219065518877002,0.00782491766491167,
-0.0105590987246595));
#38794=CARTESIAN_POINT('Ctrl Pts',(-0.219093932882599,0.00750191497004506,
-0.0105597757686429));
#38795=CARTESIAN_POINT('',(-0.21933444621923,0.00208165094137429,-0.00874770213447828));
#38796=CARTESIAN_POINT('Ctrl Pts',(-0.219093932790715,0.00750191392014267,
-0.0105597757668944));
#38797=CARTESIAN_POINT('Ctrl Pts',(-0.219091363943786,0.00747256155481735,
-0.0105597268780573));
#38798=CARTESIAN_POINT('Ctrl Pts',(-0.219083158892815,0.00737816662329933,
-0.0105590385569155));
#38799=CARTESIAN_POINT('Ctrl Pts',(-0.219070669665003,0.00723153191317315,
-0.0105557469627765));
#38800=CARTESIAN_POINT('Ctrl Pts',(-0.219049040320226,0.00697092841451702,
-0.0105453386377339));
#38801=CARTESIAN_POINT('Ctrl Pts',(-0.219023788904892,0.00664446839385532,
-0.0105197865549645));
#38802=CARTESIAN_POINT('Ctrl Pts',(-0.219004840951088,0.00636982416329366,
-0.0104876187300696));
#38803=CARTESIAN_POINT('Ctrl Pts',(-0.218993082147653,0.00617145191753081,
-0.0104591077909951));
#38804=CARTESIAN_POINT('Ctrl Pts',(-0.218987292078664,0.00606390321575527,
-0.0104424384360514));
#38805=CARTESIAN_POINT('Ctrl Pts',(-0.218978899048671,0.00587119292257413,
-0.0104091647811685));
#38806=CARTESIAN_POINT('Ctrl Pts',(-0.218971546712785,0.00564228014000307,
-0.0103643639674548));
#38807=CARTESIAN_POINT('Ctrl Pts',(-0.218964321547142,0.00522375765311925,
-0.010269771802408));
#38808=CARTESIAN_POINT('Ctrl Pts',(-0.218969821519855,0.00476695009836949,
-0.0101384745729358));
#38809=CARTESIAN_POINT('Ctrl Pts',(-0.218991661007704,0.00425642621369877,
-0.00995497442064813));
#38810=CARTESIAN_POINT('Ctrl Pts',(-0.219014980238518,0.00391149220966936,
-0.00981293822701731));
#38811=CARTESIAN_POINT('Ctrl Pts',(-0.219044445738678,0.0035938325504786,
-0.00966808189076132));
#38812=CARTESIAN_POINT('Ctrl Pts',(-0.219084102183354,0.0032795196513945,
-0.00950851937931829));
#38813=CARTESIAN_POINT('Ctrl Pts',(-0.219118245852969,0.00307177877162768,
-0.00939505134583221));
#38814=CARTESIAN_POINT('Ctrl Pts',(-0.219192630933237,0.00268000249045626,
-0.00916667015435901));
#38815=CARTESIAN_POINT('Ctrl Pts',(-0.219270936600666,0.00233524319353199,
-0.00893798766130989));
#38816=CARTESIAN_POINT('Ctrl Pts',(-0.21933444621923,0.00208165094137429,
-0.00874770213447828));
#38817=CARTESIAN_POINT('',(-0.220398889212142,0.00187262715651618,-0.00860768688447762));
#38818=CARTESIAN_POINT('Ctrl Pts',(-0.219334462389046,0.00208158637615524,
-0.00874765368687672));
#38819=CARTESIAN_POINT('Ctrl Pts',(-0.219425793438088,0.00202206306270178,
-0.00870462918406799));
#38820=CARTESIAN_POINT('Ctrl Pts',(-0.21952774431459,0.001966817344836,
-0.00866370750595934));
#38821=CARTESIAN_POINT('Ctrl Pts',(-0.219689244178597,0.0019182609466121,
-0.00862890993327191));
#38822=CARTESIAN_POINT('Ctrl Pts',(-0.219854580810695,0.00189027043079792,
-0.00861014656253604));
#38823=CARTESIAN_POINT('Ctrl Pts',(-0.219932302779978,0.00188400419581293,
-0.00860679425156521));
#38824=CARTESIAN_POINT('Ctrl Pts',(-0.220109564738917,0.00187347457135006,
-0.00860216273510668));
#38825=CARTESIAN_POINT('Ctrl Pts',(-0.220271782826522,0.00187187244955368,
-0.00860435257401022));
#38826=CARTESIAN_POINT('Ctrl Pts',(-0.220398889374219,0.00187262610998296,
-0.00860768604747057));
#38827=CARTESIAN_POINT('',(-0.220093675868021,0.00750238722497637,-0.0105812047033426));
#38828=CARTESIAN_POINT('Ctrl Pts',(-0.220398889212142,0.00187262715651618,
-0.00860768688447762));
#38829=CARTESIAN_POINT('Ctrl Pts',(-0.220325484304193,0.00213200728749386,
-0.00881442320912016));
#38830=CARTESIAN_POINT('Ctrl Pts',(-0.220234829353635,0.00248683546590626,
-0.00906356305457854));
#38831=CARTESIAN_POINT('Ctrl Pts',(-0.220148516910183,0.00289195962917674,
-0.00931277193349481));
#38832=CARTESIAN_POINT('Ctrl Pts',(-0.220108515163862,0.00310948370060873,
-0.00943785467178893));
#38833=CARTESIAN_POINT('Ctrl Pts',(-0.220062852968177,0.00343129554586821,
-0.00960968366812658));
#38834=CARTESIAN_POINT('Ctrl Pts',(-0.220028161092074,0.00375928956199721,
-0.00976693216495996));
#38835=CARTESIAN_POINT('Ctrl Pts',(-0.2200001950355,0.00411596320034711,
-0.00992117944275958));
#38836=CARTESIAN_POINT('Ctrl Pts',(-0.219972806906522,0.00464561758738128,
-0.0101209718218955));
#38837=CARTESIAN_POINT('Ctrl Pts',(-0.219963925723449,0.00512193290843601,
-0.0102645130809962));
#38838=CARTESIAN_POINT('Ctrl Pts',(-0.219969506458366,0.00555990563946997,
-0.010368087562553));
#38839=CARTESIAN_POINT('Ctrl Pts',(-0.219976339542357,0.00579963386232449,
-0.0104171404227165));
#38840=CARTESIAN_POINT('Ctrl Pts',(-0.219984587220457,0.00600242303326202,
-0.0104536932553516));
#38841=CARTESIAN_POINT('Ctrl Pts',(-0.219990333510819,0.00611399594757277,
-0.0104717372508179));
#38842=CARTESIAN_POINT('Ctrl Pts',(-0.22000218901098,0.00632132593880884,
-0.0105027872797225));
#38843=CARTESIAN_POINT('Ctrl Pts',(-0.22002126634217,0.00660537282155696,
-0.010537762376978));
#38844=CARTESIAN_POINT('Ctrl Pts',(-0.220047872899446,0.00695409209273236,
-0.0105655599657259));
#38845=CARTESIAN_POINT('Ctrl Pts',(-0.220071923105481,0.00724852275464313,
-0.010578454459571));
#38846=CARTESIAN_POINT('Ctrl Pts',(-0.220087753192226,0.00743405295678876,
-0.0105810960015779));
#38847=CARTESIAN_POINT('Ctrl Pts',(-0.220093675868021,0.00750238722497637,
-0.0105812047033426));
#38848=CARTESIAN_POINT('',(-0.220393499421047,0.0131406655980601,-0.00859683816125004));
#38849=CARTESIAN_POINT('Ctrl Pts',(-0.220093676024769,0.00750238903348299,
-0.0105812047062192));
#38850=CARTESIAN_POINT('Ctrl Pts',(-0.220064038609195,0.0078424228712658,
-0.0105804785346465));
#38851=CARTESIAN_POINT('Ctrl Pts',(-0.220028091034243,0.00829105610092071,
-0.0105507649732036));
#38852=CARTESIAN_POINT('Ctrl Pts',(-0.22000077939978,0.00869453830083411,
-0.0105006834495053));
#38853=CARTESIAN_POINT('Ctrl Pts',(-0.219988773478308,0.00890303838725181,
-0.0104690245340275));
#38854=CARTESIAN_POINT('Ctrl Pts',(-0.219982933523342,0.00901565479908935,
-0.0104505869356331));
#38855=CARTESIAN_POINT('Ctrl Pts',(-0.219974591645721,0.00921875156863704,
-0.0104135355837661));
#38856=CARTESIAN_POINT('Ctrl Pts',(-0.219967636443395,0.00945797102713633,
-0.010364072084006));
#38857=CARTESIAN_POINT('Ctrl Pts',(-0.21996180269844,0.00989499716700375,
-0.0102597121161312));
#38858=CARTESIAN_POINT('Ctrl Pts',(-0.21997008010861,0.0103646441858166,
-0.0101174395351826));
#38859=CARTESIAN_POINT('Ctrl Pts',(-0.219997251598277,0.0108961260692111,
-0.00991623904923765));
#38860=CARTESIAN_POINT('Ctrl Pts',(-0.220025403017237,0.011254696912044,
-0.00976046818541328));
#38861=CARTESIAN_POINT('Ctrl Pts',(-0.220060403203651,0.0115850292814646,
-0.00960142209635256));
#38862=CARTESIAN_POINT('Ctrl Pts',(-0.220107259625711,0.0119132768930959,
-0.00942506124254951));
#38863=CARTESIAN_POINT('Ctrl Pts',(-0.220146529462806,0.0121263777148836,
-0.0093016756523289));
#38864=CARTESIAN_POINT('Ctrl Pts',(-0.220231925495274,0.0125296319749163,
-0.00905236487169771));
#38865=CARTESIAN_POINT('Ctrl Pts',(-0.220321219690334,0.0128823887678109,
-0.00880352703074719));
#38866=CARTESIAN_POINT('Ctrl Pts',(-0.220393499421047,0.0131406655980601,
-0.00859683816125004));
#38867=CARTESIAN_POINT('Ctrl Pts',(-0.22039358407139,0.013140991540263,
-0.00859656588824042));
#38868=CARTESIAN_POINT('Ctrl Pts',(-0.220310157492514,0.0131540633141861,
-0.00858424110404083));
#38869=CARTESIAN_POINT('Ctrl Pts',(-0.220244794120044,0.0131619399905808,
-0.00857642714207583));
#38870=CARTESIAN_POINT('Ctrl Pts',(-0.220182610404876,0.0131636989800502,
-0.00857367424019087));
#38871=CARTESIAN_POINT('Ctrl Pts',(-0.220159268269797,0.0131643592585442,
-0.0085726408730547));
#38872=CARTESIAN_POINT('Ctrl Pts',(-0.220136422298581,0.0131641674296186,
-0.00857231223501343));
#38873=CARTESIAN_POINT('Ctrl Pts',(-0.220113443370469,0.0131632181340495,
-0.00857259438936373));
#38874=CARTESIAN_POINT('Ctrl Pts',(-0.220071345066223,0.0131614789870583,
-0.00857311130728197));
#38875=CARTESIAN_POINT('Ctrl Pts',(-0.220028530403874,0.013157319506211,
-0.0085755806678843));
#38876=CARTESIAN_POINT('Ctrl Pts',(-0.219979896985917,0.0131495411313915,
-0.00858081575979762));
#38877=CARTESIAN_POINT('Ctrl Pts',(-0.219946707664722,0.0131442328682444,
-0.00858438838854329));
#38878=CARTESIAN_POINT('Ctrl Pts',(-0.219910901437945,0.0131370141276404,
-0.0085894452325124));
#38879=CARTESIAN_POINT('Ctrl Pts',(-0.219879097881105,0.0131295674172822,
-0.00859475249655793));
#38880=CARTESIAN_POINT('Ctrl Pts',(-0.21986429862666,0.0131261022148859,
-0.0085972221433152));
#38881=CARTESIAN_POINT('Ctrl Pts',(-0.21985036403865,0.013122615979583,
-0.00859972378921321));
#38882=CARTESIAN_POINT('Ctrl Pts',(-0.219837954567319,0.0131193803823998,
-0.00860205524280899));
#38883=CARTESIAN_POINT('Ctrl Pts',(-0.219798877176445,0.0131091914958259,
-0.00860939698372875));
#38884=CARTESIAN_POINT('Ctrl Pts',(-0.219774519200556,0.0131019017584804,
-0.00861468504433669));
#38885=CARTESIAN_POINT('Ctrl Pts',(-0.219741730015257,0.0130915210697872,
-0.00862222162618131));
#38886=CARTESIAN_POINT('Ctrl Pts',(-0.219708940829959,0.0130811403810939,
-0.00862975820802594));
#38887=CARTESIAN_POINT('Ctrl Pts',(-0.219667972560944,0.0130672096099914,
-0.00863991639049878));
#38888=CARTESIAN_POINT('Ctrl Pts',(-0.219624658540191,0.0130511824119699,
-0.00865158596317062));
#38889=CARTESIAN_POINT('Ctrl Pts',(-0.219538033728064,0.0130191292108723,
-0.00867492423846189));
#38890=CARTESIAN_POINT('Ctrl Pts',(-0.219442025425284,0.0129787732466052,
-0.00870422485193976));
#38891=CARTESIAN_POINT('Ctrl Pts',(-0.21932971552655,0.0129301753163333,
-0.00873889027865428));
#38892=CARTESIAN_POINT('Origin',(-0.21760795824129,0.00750000466343435,
-0.0015071771812637));
#38893=CARTESIAN_POINT('',(-0.217213394097559,0.0124661280854866,-0.0090257192728346));
#38894=CARTESIAN_POINT('',(-0.217094603491324,0.00750113103643811,-0.0105144286907592));
#38895=CARTESIAN_POINT('Ctrl Pts',(-0.217213394097559,0.0124661280854866,
-0.0090257192728346));
#38896=CARTESIAN_POINT('Ctrl Pts',(-0.21717041116494,0.0122246593680101,
-0.00918417758179821));
#38897=CARTESIAN_POINT('Ctrl Pts',(-0.217117057284765,0.0119007341084134,
-0.0093732488499977));
#38898=CARTESIAN_POINT('Ctrl Pts',(-0.21706465598238,0.0115324288885954,
-0.00956270965111247));
#38899=CARTESIAN_POINT('Ctrl Pts',(-0.217040698371939,0.0113484579716673,
-0.00965206989281391));
#38900=CARTESIAN_POINT('Ctrl Pts',(-0.217007713187453,0.0110273071878711,
-0.00979619168030236));
#38901=CARTESIAN_POINT('Ctrl Pts',(-0.216979134587681,0.0106353061403178,
-0.00995398193963724));
#38902=CARTESIAN_POINT('Ctrl Pts',(-0.216960102400533,0.0100812880088519,
-0.0101420606778224));
#38903=CARTESIAN_POINT('Ctrl Pts',(-0.216964970234854,0.00960681098718408,
-0.0102666718666015));
#38904=CARTESIAN_POINT('Ctrl Pts',(-0.216978302680794,0.00921416448670835,
-0.0103486251961947));
#38905=CARTESIAN_POINT('Ctrl Pts',(-0.21698838211439,0.00899401757483317,
-0.01038817297612));
#38906=CARTESIAN_POINT('Ctrl Pts',(-0.216999139916386,0.00879594563401397,
-0.010419159692913));
#38907=CARTESIAN_POINT('Ctrl Pts',(-0.217004856243495,0.00870275409322374,
-0.0104320663215466));
#38908=CARTESIAN_POINT('Ctrl Pts',(-0.217016574597487,0.00851987098217247,
-0.0104557992732465));
#38909=CARTESIAN_POINT('Ctrl Pts',(-0.217040946256797,0.00817310207656308,
-0.0104923571850839));
#38910=CARTESIAN_POINT('Ctrl Pts',(-0.217070785262386,0.00778990612293632,
-0.0105138775080055));
#38911=CARTESIAN_POINT('Ctrl Pts',(-0.217094604240616,0.00750113159837561,
-0.010514428709891));
#38912=CARTESIAN_POINT('',(-0.217217196076401,0.00253915440696052,-0.00902927251451939));
#38913=CARTESIAN_POINT('Ctrl Pts',(-0.217094604204801,0.00750113097791163,
-0.0105144287091931));
#38914=CARTESIAN_POINT('Ctrl Pts',(-0.217084161848402,0.00737376523387638,
-0.0105142185903619));
#38915=CARTESIAN_POINT('Ctrl Pts',(-0.217060477387662,0.00707794301303083,
-0.01050688284421));
#38916=CARTESIAN_POINT('Ctrl Pts',(-0.217034564919892,0.00673221457752508,
-0.0104821172122667));
#38917=CARTESIAN_POINT('Ctrl Pts',(-0.217017123930288,0.00648242698557118,
-0.0104560964710192));
#38918=CARTESIAN_POINT('Ctrl Pts',(-0.217005554768794,0.00629995272480641,
-0.0104324364268733));
#38919=CARTESIAN_POINT('Ctrl Pts',(-0.216999885759004,0.00620651112707121,
-0.0104195265524636));
#38920=CARTESIAN_POINT('Ctrl Pts',(-0.216989325922178,0.00600939813741562,
-0.0103887567565715));
#38921=CARTESIAN_POINT('Ctrl Pts',(-0.216979430273025,0.00578936969628363,
-0.0103493264841639));
#38922=CARTESIAN_POINT('Ctrl Pts',(-0.216966473873743,0.00539729869136527,
-0.0102676831160186));
#38923=CARTESIAN_POINT('Ctrl Pts',(-0.216962156491798,0.00492156112687701,
-0.0101429282776497));
#38924=CARTESIAN_POINT('Ctrl Pts',(-0.216981833480707,0.00436966098887771,
-0.00995584505032058));
#38925=CARTESIAN_POINT('Ctrl Pts',(-0.217010842686626,0.00397750116182149,
-0.0097983012137332));
#38926=CARTESIAN_POINT('Ctrl Pts',(-0.217044214738291,0.00365555388525719,
-0.00965402891301301));
#38927=CARTESIAN_POINT('Ctrl Pts',(-0.217068262983783,0.00347186850781422,
-0.00956491767776186));
#38928=CARTESIAN_POINT('Ctrl Pts',(-0.21712081802361,0.00310386192693681,
-0.0093758711515526));
#38929=CARTESIAN_POINT('Ctrl Pts',(-0.217174218047225,0.00278029120291905,
-0.00918727068287094));
#38930=CARTESIAN_POINT('Ctrl Pts',(-0.217217196076401,0.00253915440696052,
-0.00902927251451939));
#38931=CARTESIAN_POINT('',(-0.218253133349592,0.00235141795600442,-0.00892454475911964));
#38932=CARTESIAN_POINT('Ctrl Pts',(-0.217217809477599,0.00253896772880568,
-0.0090293011698677));
#38933=CARTESIAN_POINT('Ctrl Pts',(-0.217290041369587,0.00250069176491746,
-0.00900556706915477));
#38934=CARTESIAN_POINT('Ctrl Pts',(-0.217368407052876,0.0024671494138073,
-0.00898467489825882));
#38935=CARTESIAN_POINT('Ctrl Pts',(-0.217450359266991,0.00244089398796864,
-0.00896864143762584));
#38936=CARTESIAN_POINT('Ctrl Pts',(-0.217491335374049,0.0024277662750493,
-0.00896062470730935));
#38937=CARTESIAN_POINT('Ctrl Pts',(-0.217533055849,0.00241628436709229,
-0.00895369982738143));
#38938=CARTESIAN_POINT('Ctrl Pts',(-0.217580470128854,0.00240565996459356,
-0.00894744657919007));
#38939=CARTESIAN_POINT('Ctrl Pts',(-0.217627884408709,0.00239503556209484,
-0.00894119333099871));
#38940=CARTESIAN_POINT('Ctrl Pts',(-0.21768122272973,0.00238589707961749,
-0.00893604813963404));
#38941=CARTESIAN_POINT('Ctrl Pts',(-0.217720667840838,0.00238036482543931,
-0.00893308565286313));
#38942=CARTESIAN_POINT('Ctrl Pts',(-0.21772785791221,0.00237935640383077,
-0.00893254564953383));
#38943=CARTESIAN_POINT('Ctrl Pts',(-0.217734589088163,0.00237845246471081,
-0.00893206729807201));
#38944=CARTESIAN_POINT('Ctrl Pts',(-0.217740992213186,0.00237762157144803,
-0.00893163189219981));
#38945=CARTESIAN_POINT('Ctrl Pts',(-0.217769716970056,0.00237389414040906,
-0.0089296786384724));
#38946=CARTESIAN_POINT('Ctrl Pts',(-0.217791731404344,0.00237149849359442,
-0.00892849060637797));
#38947=CARTESIAN_POINT('Ctrl Pts',(-0.217819659624921,0.00236886316801429,
-0.00892726140202061));
#38948=CARTESIAN_POINT('Ctrl Pts',(-0.217853813412136,0.0023656403938008,
-0.00892575819189133));
#38949=CARTESIAN_POINT('Ctrl Pts',(-0.21789677874394,0.00236237522790454,
-0.0089244180371867));
#38950=CARTESIAN_POINT('Ctrl Pts',(-0.217942798021502,0.00235987579789025,
-0.0089236782831972));
#38951=CARTESIAN_POINT('Ctrl Pts',(-0.218032838016481,0.00235498548500703,
-0.00892223090181643));
#38952=CARTESIAN_POINT('Ctrl Pts',(-0.218134518988832,0.00235293450087632,
-0.00892302018243319));
#38953=CARTESIAN_POINT('Ctrl Pts',(-0.218253133349592,0.00235141795600442,
-0.00892454475911964));
#38954=CARTESIAN_POINT('',(-0.218094235237686,0.00750143446742459,-0.0105360562554827));
#38955=CARTESIAN_POINT('Ctrl Pts',(-0.218253133066283,0.00235141263875458,
-0.00892455212338305));
#38956=CARTESIAN_POINT('Ctrl Pts',(-0.218214219872793,0.00253247183269533,
-0.00904968294283068));
#38957=CARTESIAN_POINT('Ctrl Pts',(-0.218179081459859,0.00271867387981424,
-0.00916861222376044));
#38958=CARTESIAN_POINT('Ctrl Pts',(-0.21803449218446,0.00360160792485018,
-0.00968787065959727));
#38959=CARTESIAN_POINT('Ctrl Pts',(-0.217972979168045,0.00434860675246558,
-0.0100034645917515));
#38960=CARTESIAN_POINT('Ctrl Pts',(-0.217957033748206,0.00590729686837615,
-0.0104276715988628));
#38961=CARTESIAN_POINT('Ctrl Pts',(-0.218001909352134,0.00670430387980213,
-0.0105340609659123));
#38962=CARTESIAN_POINT('Ctrl Pts',(-0.218097813131851,0.00750001270663325,
-0.0105361337811779));
#38963=CARTESIAN_POINT('',(-0.2182565110078,0.0126543573605341,-0.00892058764987726));
#38964=CARTESIAN_POINT('Ctrl Pts',(-0.218094235237686,0.00750143446742459,
-0.0105360562554827));
#38965=CARTESIAN_POINT('Ctrl Pts',(-0.218067105154875,0.00780677055571136,
-0.0105354203113047));
#38966=CARTESIAN_POINT('Ctrl Pts',(-0.218033831405312,0.00820961502316317,
-0.0105114742256329));
#38967=CARTESIAN_POINT('Ctrl Pts',(-0.218007882474728,0.00857238380872824,
-0.0104711475163477));
#38968=CARTESIAN_POINT('Ctrl Pts',(-0.217996152558159,0.00875980809131382,
-0.0104456876420246));
#38969=CARTESIAN_POINT('Ctrl Pts',(-0.217990313058703,0.00886144379089272,
-0.0104307972172058));
#38970=CARTESIAN_POINT('Ctrl Pts',(-0.217981597968648,0.00904302164651337,
-0.0104011947822263));
#38971=CARTESIAN_POINT('Ctrl Pts',(-0.217973528732665,0.00925803386380941,
-0.0103615120623033));
#38972=CARTESIAN_POINT('Ctrl Pts',(-0.217964102590318,0.0096505431499046,
-0.010278050687789));
#38973=CARTESIAN_POINT('Ctrl Pts',(-0.217965530958217,0.0101943339463829,
-0.0101316150791819));
#38974=CARTESIAN_POINT('Ctrl Pts',(-0.217989853133676,0.0107921989301394,
-0.00991655019287694));
#38975=CARTESIAN_POINT('Ctrl Pts',(-0.218020475341655,0.0111925938083483,
-0.0097457526023216));
#38976=CARTESIAN_POINT('Ctrl Pts',(-0.218052426173444,0.0114968851846426,
-0.00960217923509529));
#38977=CARTESIAN_POINT('Ctrl Pts',(-0.218079973263592,0.0116953987503668,
-0.00950129475060471));
#38978=CARTESIAN_POINT('Ctrl Pts',(-0.218140496279061,0.0120732358289631,
-0.00929682365052865));
#38979=CARTESIAN_POINT('Ctrl Pts',(-0.218204497408712,0.0124072068218569,
-0.00909170879414502));
#38980=CARTESIAN_POINT('Ctrl Pts',(-0.2182565110078,0.0126543573605341,
-0.00892058764987726));
#38981=CARTESIAN_POINT('Ctrl Pts',(-0.218256501705708,0.0126543585852145,
-0.00892058659399183));
#38982=CARTESIAN_POINT('Ctrl Pts',(-0.218154525997755,0.0126678026917317,
-0.00890901246260343));
#38983=CARTESIAN_POINT('Ctrl Pts',(-0.218078194794121,0.0126730947409307,
-0.00890364142665837));
#38984=CARTESIAN_POINT('Ctrl Pts',(-0.217909752747571,0.0126633106168309,
-0.00890684541098475));
#38985=CARTESIAN_POINT('Ctrl Pts',(-0.217821972872918,0.0126501072829163,
-0.00891420792415138));
#38986=CARTESIAN_POINT('Ctrl Pts',(-0.21754967081416,0.0125870145067814,
-0.00895194276125938));
#38987=CARTESIAN_POINT('Ctrl Pts',(-0.217380015618932,0.0125265412057645,
-0.00898944383847723));
#38988=CARTESIAN_POINT('Ctrl Pts',(-0.217213440148644,0.0124661800217875,
-0.009025685986326));
#38989=CARTESIAN_POINT('Origin',(-0.215572945664865,0.00750000047003143,
-0.00143236497997678));
#38990=CARTESIAN_POINT('',(-0.215184743945676,0.012323689646171,-0.00907719137595261));
#38991=CARTESIAN_POINT('',(-0.215095211258851,0.00750052176516078,-0.010469157777843));
#38992=CARTESIAN_POINT('Ctrl Pts',(-0.215184743945676,0.012323689646171,
-0.00907719137595261));
#38993=CARTESIAN_POINT('Ctrl Pts',(-0.21514648660725,0.0120862670790848,
-0.00922607274352441));
#38994=CARTESIAN_POINT('Ctrl Pts',(-0.215099018442826,0.0117687123887809,
-0.00940346464373393));
#38995=CARTESIAN_POINT('Ctrl Pts',(-0.215052369462544,0.0114082657322194,
-0.00958112131941231));
#38996=CARTESIAN_POINT('Ctrl Pts',(-0.215031100534081,0.0112292263444702,
-0.00966451563804252));
#38997=CARTESIAN_POINT('Ctrl Pts',(-0.21500151205561,0.0109134744577964,
-0.00980042007136559));
#38998=CARTESIAN_POINT('Ctrl Pts',(-0.214976322453243,0.0105309593786002,
-0.00994796510360923));
#38999=CARTESIAN_POINT('Ctrl Pts',(-0.214960394330003,0.00999902377695271,
-0.0101215370958852));
#39000=CARTESIAN_POINT('Ctrl Pts',(-0.214966324260738,0.00953215587950937,
-0.0102394787165332));
#39001=CARTESIAN_POINT('Ctrl Pts',(-0.214980033976025,0.00915301666182799,
-0.0103153885509512));
#39002=CARTESIAN_POINT('Ctrl Pts',(-0.214990161391655,0.00894081415800363,
-0.0103520081134918));
#39003=CARTESIAN_POINT('Ctrl Pts',(-0.215000843349877,0.0087507069385728,
-0.0103805993488392));
#39004=CARTESIAN_POINT('Ctrl Pts',(-0.215006529173423,0.00866069457107862,
-0.0103925976782496));
#39005=CARTESIAN_POINT('Ctrl Pts',(-0.215018149652307,0.00848438866324892,
-0.0104146108210603));
#39006=CARTESIAN_POINT('Ctrl Pts',(-0.215042272034264,0.00814969066011635,
-0.0104485878385499));
#39007=CARTESIAN_POINT('Ctrl Pts',(-0.215071730086938,0.00777959042738062,
-0.0104686311967555));
#39008=CARTESIAN_POINT('Ctrl Pts',(-0.215095211712589,0.00750052238910928,
-0.0104691577890294));
#39009=CARTESIAN_POINT('',(-0.215187317923645,0.00267870325034433,-0.00907875410590838));
#39010=CARTESIAN_POINT('Ctrl Pts',(-0.215095211657488,0.00750052173172372,
-0.0104691577878692));
#39011=CARTESIAN_POINT('Ctrl Pts',(-0.215093348816256,0.0074782969939577,
-0.0104691185637939));
#39012=CARTESIAN_POINT('Ctrl Pts',(-0.215086094585673,0.00739134142684377,
-0.0104685644526724));
#39013=CARTESIAN_POINT('Ctrl Pts',(-0.215075843703081,0.00726661667161012,
-0.0104660613626304));
#39014=CARTESIAN_POINT('Ctrl Pts',(-0.215057434122424,0.00703872552940382,
-0.0104581862817437));
#39015=CARTESIAN_POINT('Ctrl Pts',(-0.215035586165921,0.00675491463768686,
-0.0104388446803273));
#39016=CARTESIAN_POINT('Ctrl Pts',(-0.215018376650014,0.00651490499106983,
-0.0104145485250919));
#39017=CARTESIAN_POINT('Ctrl Pts',(-0.215006844975634,0.00633859231783919,
-0.01039251067607));
#39018=CARTESIAN_POINT('Ctrl Pts',(-0.215001196968655,0.00624840215077872,
-0.0103804808191619));
#39019=CARTESIAN_POINT('Ctrl Pts',(-0.214990660376026,0.00605883545559521,
-0.0103519593738021));
#39020=CARTESIAN_POINT('Ctrl Pts',(-0.214980672161886,0.00584665249207341,
-0.0103153399439608));
#39021=CARTESIAN_POINT('Ctrl Pts',(-0.214967245748183,0.00546782162430372,
-0.0102394950560305));
#39022=CARTESIAN_POINT('Ctrl Pts',(-0.214961732355427,0.00500012678372268,
-0.0101213055392285));
#39023=CARTESIAN_POINT('Ctrl Pts',(-0.214978156077839,0.00446989750802472,
-0.00994828915619471));
#39024=CARTESIAN_POINT('Ctrl Pts',(-0.215003681155038,0.00408735391033809,
-0.00980081329302173));
#39025=CARTESIAN_POINT('Ctrl Pts',(-0.215033590721385,0.00377091209053468,
-0.00966463271638572));
#39026=CARTESIAN_POINT('Ctrl Pts',(-0.215054895180567,0.00359250015699713,
-0.00958153380973349));
#39027=CARTESIAN_POINT('Ctrl Pts',(-0.215101625155304,0.00323264763109776,
-0.0094042312271201));
#39028=CARTESIAN_POINT('Ctrl Pts',(-0.21514908525396,0.00291571044311647,
-0.00922727046007243));
#39029=CARTESIAN_POINT('Ctrl Pts',(-0.215187317923645,0.00267870325034433,
-0.00907875410590838));
#39030=CARTESIAN_POINT('',(-0.216194991836357,0.00264076678978001,-0.00907662738373749));
#39031=CARTESIAN_POINT('Ctrl Pts',(-0.215187406628623,0.00267868409859472,
-0.00907874392743814));
#39032=CARTESIAN_POINT('Ctrl Pts',(-0.21552326791646,0.00266602963457283,
-0.00907807250913494));
#39033=CARTESIAN_POINT('Ctrl Pts',(-0.215859129663761,0.00265338920072677,
-0.0090773662716867));
#39034=CARTESIAN_POINT('Ctrl Pts',(-0.21619499193747,0.00264076476354384,
-0.00907662607383746));
#39035=CARTESIAN_POINT('',(-0.216094920727691,0.00750081535589013,-0.0104908925867836));
#39036=CARTESIAN_POINT('Ctrl Pts',(-0.216194991836357,0.00264076678978001,
-0.00907662738373749));
#39037=CARTESIAN_POINT('Ctrl Pts',(-0.216155366004592,0.00288037027759099,
-0.00922841667383286));
#39038=CARTESIAN_POINT('Ctrl Pts',(-0.216106174921698,0.00320114029982177,
-0.00940926923509961));
#39039=CARTESIAN_POINT('Ctrl Pts',(-0.216057819495052,0.00356499889891992,
-0.009590150528347));
#39040=CARTESIAN_POINT('Ctrl Pts',(-0.216035682401327,0.00374666276300005,
-0.00967541861388872));
#39041=CARTESIAN_POINT('Ctrl Pts',(-0.21600516202416,0.00406273234928654,
-0.0098125207512195));
#39042=CARTESIAN_POINT('Ctrl Pts',(-0.215978862788875,0.00444643562956339,
-0.00996170720449533));
#39043=CARTESIAN_POINT('Ctrl Pts',(-0.215961627981838,0.00497762456890586,
-0.0101366227379806));
#39044=CARTESIAN_POINT('Ctrl Pts',(-0.215966673091261,0.00544925004400758,
-0.0102570027663552));
#39045=CARTESIAN_POINT('Ctrl Pts',(-0.215979918232889,0.00583091044504249,
-0.010334140462034));
#39046=CARTESIAN_POINT('Ctrl Pts',(-0.21598984730753,0.00604476982194863,
-0.0103714130964631));
#39047=CARTESIAN_POINT('Ctrl Pts',(-0.216000365432515,0.00623593452875368,
-0.0104004595092437));
#39048=CARTESIAN_POINT('Ctrl Pts',(-0.216006025580804,0.00632705052741814,
-0.0104127398163461));
#39049=CARTESIAN_POINT('Ctrl Pts',(-0.216017604486095,0.00650523993901912,
-0.0104352082840549));
#39050=CARTESIAN_POINT('Ctrl Pts',(-0.21604165432455,0.00684284821730302,
-0.0104699298205827));
#39051=CARTESIAN_POINT('Ctrl Pts',(-0.216071599729952,0.00722182610486624,
-0.0104904107732437));
#39052=CARTESIAN_POINT('Ctrl Pts',(-0.216094920728811,0.00750081502625171,
-0.0104908925868377));
#39053=CARTESIAN_POINT('',(-0.216191681155669,0.0123629325401175,-0.00907419422952278));
#39054=CARTESIAN_POINT('Ctrl Pts',(-0.216094920727691,0.00750081535589013,
-0.0104908925867836));
#39055=CARTESIAN_POINT('Ctrl Pts',(-0.21607114795769,0.00778396749876566,
-0.0104903501412173));
#39056=CARTESIAN_POINT('Ctrl Pts',(-0.216041367011789,0.00815931797022712,
-0.0104697259238784));
#39057=CARTESIAN_POINT('Ctrl Pts',(-0.216017038090091,0.00849870004219069,
-0.0104347690624456));
#39058=CARTESIAN_POINT('Ctrl Pts',(-0.216005363149858,0.00867711965280929,
-0.0104121793506864));
#39059=CARTESIAN_POINT('Ctrl Pts',(-0.21599962253345,0.00876887272456124,
-0.0103997619303256));
#39060=CARTESIAN_POINT('Ctrl Pts',(-0.215989057163612,0.0089590976354752,
-0.0103707564576226));
#39061=CARTESIAN_POINT('Ctrl Pts',(-0.215979036512872,0.00917200431861489,
-0.0103335666094436));
#39062=CARTESIAN_POINT('Ctrl Pts',(-0.215965573411188,0.00955218224306641,
-0.01025658134513));
#39063=CARTESIAN_POINT('Ctrl Pts',(-0.215959983300432,0.0100198628373282,
-0.0101373332269741));
#39064=CARTESIAN_POINT('Ctrl Pts',(-0.215976608750281,0.0105552916003265,
-0.00996109009686354));
#39065=CARTESIAN_POINT('Ctrl Pts',(-0.216002575783096,0.0109398514635131,
-0.00981140744813802));
#39066=CARTESIAN_POINT('Ctrl Pts',(-0.216032886151583,0.0112567101897491,
-0.00967382351912691));
#39067=CARTESIAN_POINT('Ctrl Pts',(-0.216054884878806,0.0114382008550471,
-0.00958853634620765));
#39068=CARTESIAN_POINT('Ctrl Pts',(-0.216103051979017,0.0118022669367451,
-0.00940736798328436));
#39069=CARTESIAN_POINT('Ctrl Pts',(-0.216152125740651,0.0121231895976479,
-0.00922623781176936));
#39070=CARTESIAN_POINT('Ctrl Pts',(-0.216191681155669,0.0123629325401175,
-0.00907419422952278));
#39071=CARTESIAN_POINT('Ctrl Pts',(-0.216191679984792,0.0123629610678733,
-0.00907417531574932));
#39072=CARTESIAN_POINT('Ctrl Pts',(-0.215856063870635,0.0123498846849188,
-0.00907522003451906));
#39073=CARTESIAN_POINT('Ctrl Pts',(-0.215520448246673,0.0123367926637154,
-0.00907622680850737));
#39074=CARTESIAN_POINT('Ctrl Pts',(-0.215184833018176,0.0123236876257974,
-0.00907719458563817));
#39075=CARTESIAN_POINT('Origin',(-0.191548193502062,0.0075000009419683,
-0.000492621109443556));
#39076=CARTESIAN_POINT('',(-0.192104402373237,0.00750389176243192,-0.00994933158139058));
#39077=CARTESIAN_POINT('',(-0.192122530472206,0.0119802570120685,-0.00881815091622089));
#39078=CARTESIAN_POINT('Ctrl Pts',(-0.192108734077425,0.00750469088463491,
-0.00994879424709136));
#39079=CARTESIAN_POINT('Ctrl Pts',(-0.192103207711712,0.0075509068388887,
-0.00994865116432292));
#39080=CARTESIAN_POINT('Ctrl Pts',(-0.192097845739629,0.00759714834567246,
-0.00994817223080437));
#39081=CARTESIAN_POINT('Ctrl Pts',(-0.191980221684322,0.00864423060253309,
-0.00992970587840616));
#39082=CARTESIAN_POINT('Ctrl Pts',(-0.191946432880569,0.00963929255173959,
-0.00975446086017676));
#39083=CARTESIAN_POINT('Ctrl Pts',(-0.192015568180551,0.0110713112592102,
-0.00926000378799105));
#39084=CARTESIAN_POINT('Ctrl Pts',(-0.192059160699483,0.0115364242758858,
-0.00905610534302461));
#39085=CARTESIAN_POINT('Ctrl Pts',(-0.192122341662653,0.0119805125490225,
-0.00881800902404164));
#39086=CARTESIAN_POINT('',(-0.191053645153712,0.0113981655634775,-0.00908339543415031));
#39087=CARTESIAN_POINT('Ctrl Pts',(-0.192122530472206,0.0119802570120685,
-0.00881815091622089));
#39088=CARTESIAN_POINT('Ctrl Pts',(-0.19199161678884,0.0119322240752818,
-0.0088412067577884));
#39089=CARTESIAN_POINT('Ctrl Pts',(-0.191879939462572,0.0118894807233055,
-0.00886131310476818));
#39090=CARTESIAN_POINT('Ctrl Pts',(-0.191781985634829,0.0118492817294659,
-0.00888005248158014));
#39091=CARTESIAN_POINT('Ctrl Pts',(-0.191732121208329,0.011828818008753,
-0.00888959195848701));
#39092=CARTESIAN_POINT('Ctrl Pts',(-0.191685813361322,0.0118090078712822,
-0.00889876632261227));
#39093=CARTESIAN_POINT('Ctrl Pts',(-0.191648874008136,0.0117929042881476,
-0.00890618640190862));
#39094=CARTESIAN_POINT('Ctrl Pts',(-0.191611934654949,0.0117768007050129,
-0.00891360648120497));
#39095=CARTESIAN_POINT('Ctrl Pts',(-0.191584363162224,0.0117644186426757,
-0.00891930142696703));
#39096=CARTESIAN_POINT('Ctrl Pts',(-0.19154291056778,0.0117435795925307,
-0.00892888798659096));
#39097=CARTESIAN_POINT('Ctrl Pts',(-0.191501457973336,0.0117227405423857,
-0.00893847454621488));
#39098=CARTESIAN_POINT('Ctrl Pts',(-0.191446125407219,0.0116934182420501,
-0.00895190070791356));
#39099=CARTESIAN_POINT('Ctrl Pts',(-0.191397663363911,0.0116652096291388,
-0.00896471741532005));
#39100=CARTESIAN_POINT('Ctrl Pts',(-0.191349201320603,0.0116370010162275,
-0.00897753412272655));
#39101=CARTESIAN_POINT('Ctrl Pts',(-0.191307608992891,0.0116099242324839,
-0.0089897785286841));
#39102=CARTESIAN_POINT('Ctrl Pts',(-0.191267699831175,0.0115815575659545,
-0.00900251346495063));
#39103=CARTESIAN_POINT('Ctrl Pts',(-0.1911878850761,0.0115248267692159,
-0.00902798219882765));
#39104=CARTESIAN_POINT('Ctrl Pts',(-0.191114803398555,0.0114629153130397,
-0.00905536613897805));
#39105=CARTESIAN_POINT('Ctrl Pts',(-0.191053645153712,0.0113981655634775,
-0.00908339543415031));
#39106=CARTESIAN_POINT('',(-0.191102317990465,0.00750205528623176,-0.00992689696933848));
#39107=CARTESIAN_POINT('Ctrl Pts',(-0.191053667625411,0.0113981565442571,
-0.00908340001178101));
#39108=CARTESIAN_POINT('Ctrl Pts',(-0.191051193363694,0.0113718165320938,
-0.00909528900497808));
#39109=CARTESIAN_POINT('Ctrl Pts',(-0.191048779622539,0.0113454205791333,
-0.0091070587574167));
#39110=CARTESIAN_POINT('Ctrl Pts',(-0.190954175177597,0.0102820119819883,
-0.00957542619835343));
#39111=CARTESIAN_POINT('Ctrl Pts',(-0.190955921046233,0.00917583914081459,
-0.00984130463999999));
#39112=CARTESIAN_POINT('Ctrl Pts',(-0.191064314723308,0.0078705269708081,
-0.00992065058137066));
#39113=CARTESIAN_POINT('Ctrl Pts',(-0.191082145256522,0.00768562531559786,
-0.00992646114623245));
#39114=CARTESIAN_POINT('Ctrl Pts',(-0.191102363522027,0.00750132035680661,
-0.00992692622707289));
#39115=CARTESIAN_POINT('',(-0.191055938690558,0.00361094738279529,-0.00908764566835488));
#39116=CARTESIAN_POINT('Ctrl Pts',(-0.191104123278973,0.00750132061311004,
-0.00992696446771463));
#39117=CARTESIAN_POINT('Ctrl Pts',(-0.19106845003887,0.00717518850570648,
-0.00992623479437091));
#39118=CARTESIAN_POINT('Ctrl Pts',(-0.191040610403852,0.00685082501865862,
-0.0099087736553339));
#39119=CARTESIAN_POINT('Ctrl Pts',(-0.190956197985429,0.00550729994350422,
-0.0097680742307451));
#39120=CARTESIAN_POINT('Ctrl Pts',(-0.190969527586036,0.00452315153618091,
-0.00949802905279705));
#39121=CARTESIAN_POINT('Ctrl Pts',(-0.191054063007182,0.00361171883661926,
-0.00908787631838634));
#39122=CARTESIAN_POINT('',(-0.192132222592215,0.00302368985652182,-0.0088204938392334));
#39123=CARTESIAN_POINT('Ctrl Pts',(-0.191056694227376,0.00361001886952257,
-0.00908716487649774));
#39124=CARTESIAN_POINT('Ctrl Pts',(-0.191117646682474,0.00354507577298782,
-0.00905911829100523));
#39125=CARTESIAN_POINT('Ctrl Pts',(-0.191190576613973,0.003482977172259,
-0.00903171364009081));
#39126=CARTESIAN_POINT('Ctrl Pts',(-0.191270285221213,0.00342607672119435,
-0.00900622453480157));
#39127=CARTESIAN_POINT('Ctrl Pts',(-0.191310139525385,0.00339762649526841,
-0.00899347998198063));
#39128=CARTESIAN_POINT('Ctrl Pts',(-0.191351688242736,0.00337047038354003,
-0.00898122608515244));
#39129=CARTESIAN_POINT('Ctrl Pts',(-0.19140012564909,0.00334217558575491,
-0.0089683974383084));
#39130=CARTESIAN_POINT('Ctrl Pts',(-0.191448563055443,0.00331388078796979,
-0.00895556879146436));
#39131=CARTESIAN_POINT('Ctrl Pts',(-0.191503889964036,0.00328446553423945,
-0.00894212797770866));
#39132=CARTESIAN_POINT('Ctrl Pts',(-0.191545324948472,0.00326357080218557,
-0.00893253552891437));
#39133=CARTESIAN_POINT('Ctrl Pts',(-0.191586759932908,0.00324267607013168,
-0.00892294308012008));
#39134=CARTESIAN_POINT('Ctrl Pts',(-0.191614301855269,0.00323027547924158,
-0.00891725135146682));
#39135=CARTESIAN_POINT('Ctrl Pts',(-0.191651228210345,0.00321413808329353,
-0.00890983105241841));
#39136=CARTESIAN_POINT('Ctrl Pts',(-0.191688154565421,0.00319800068734548,
-0.00890241075337));
#39137=CARTESIAN_POINT('Ctrl Pts',(-0.1917344659906,0.00317814151164943,
-0.00889323255797904));
#39138=CARTESIAN_POINT('Ctrl Pts',(-0.191784343440197,0.00315762666347515,
-0.00888368869751462));
#39139=CARTESIAN_POINT('Ctrl Pts',(-0.19188409833939,0.0031165969671266,
-0.00886460097658579));
#39140=CARTESIAN_POINT('Ctrl Pts',(-0.191998116385108,0.00307292140876782,
-0.00884409435676829));
#39141=CARTESIAN_POINT('Ctrl Pts',(-0.192132222764199,0.00302369025826422,
-0.00882049405934325));
#39142=CARTESIAN_POINT('Ctrl Pts',(-0.192132222592215,0.00302368985652182,
-0.0088204938392334));
#39143=CARTESIAN_POINT('Ctrl Pts',(-0.192103791504356,0.00325082082607522,
-0.00894220488147181));
#39144=CARTESIAN_POINT('Ctrl Pts',(-0.192068646087494,0.00355203440365802,
-0.00908672318139968));
#39145=CARTESIAN_POINT('Ctrl Pts',(-0.192034396050521,0.00389166889704801,
-0.00923113586730494));
#39146=CARTESIAN_POINT('Ctrl Pts',(-0.19201895526882,0.00405874480199876,
-0.00929842428009787));
#39147=CARTESIAN_POINT('Ctrl Pts',(-0.191997619334613,0.0043567261598758,
-0.0094095168730219));
#39148=CARTESIAN_POINT('Ctrl Pts',(-0.191980450765341,0.00471410316628912,
-0.00952906101135592));
#39149=CARTESIAN_POINT('Ctrl Pts',(-0.191971848059539,0.00520369664809944,
-0.00966821105761361));
#39150=CARTESIAN_POINT('Ctrl Pts',(-0.191980537392393,0.00563814596492265,
-0.00976411773704245));
#39151=CARTESIAN_POINT('Ctrl Pts',(-0.191994962083258,0.00598633526148447,
-0.00982505229803761));
#39152=CARTESIAN_POINT('Ctrl Pts',(-0.192005079326421,0.00618120430706718,
-0.00985448438518454));
#39153=CARTESIAN_POINT('Ctrl Pts',(-0.192015400395759,0.00635425493589708,
-0.00987729266943201));
#39154=CARTESIAN_POINT('Ctrl Pts',(-0.19202086841947,0.00643706239649949,
-0.00988698789097493));
#39155=CARTESIAN_POINT('Ctrl Pts',(-0.192031975743343,0.0065989007730196,
-0.0099047027533171));
#39156=CARTESIAN_POINT('Ctrl Pts',(-0.192048185086397,0.00681719200235256,
-0.00992426365281129));
#39157=CARTESIAN_POINT('Ctrl Pts',(-0.192069332648122,0.0070838409743984,
-0.00993985662063671));
#39158=CARTESIAN_POINT('Ctrl Pts',(-0.192085638344594,0.00728158938794661,
-0.00994618972545213));
#39159=CARTESIAN_POINT('Ctrl Pts',(-0.192096778314419,0.00741407240370789,
-0.009948236681352));
#39160=CARTESIAN_POINT('Ctrl Pts',(-0.192100401188873,0.00745684365403462,
-0.00994862837396258));
#39161=CARTESIAN_POINT('Ctrl Pts',(-0.192104337739042,0.00750296369756609,
-0.00994869941298362));
#39162=CARTESIAN_POINT('Origin',(-0.22657497719928,0.0105076883533885,0.00733431533838148));
#39163=CARTESIAN_POINT('Ctrl Pts',(-0.225970553562738,0.0102603089488576,
0.0102745179149678));
#39164=CARTESIAN_POINT('Ctrl Pts',(-0.225969704710384,0.010270943438745,
0.0103064390545693));
#39165=CARTESIAN_POINT('Ctrl Pts',(-0.225968879295254,0.0102817420965276,
0.0103382186548783));
#39166=CARTESIAN_POINT('Ctrl Pts',(-0.225968077478529,0.0102926941256055,
0.0103698341560209));
#39167=CARTESIAN_POINT('Ctrl Pts',(-0.226088480400989,0.00749337594554441,
0.0108173434082515));
#39168=CARTESIAN_POINT('Ctrl Pts',(-0.226091023274651,0.00749377529304714,
0.0107836282080371));
#39169=CARTESIAN_POINT('Ctrl Pts',(-0.226093596038501,0.00749416765923866,
0.0107499145846004));
#39170=CARTESIAN_POINT('Ctrl Pts',(-0.226096198745771,0.00749455297790887,
0.0107162215195238));
#39171=CARTESIAN_POINT('Origin',(-0.226550254959384,0.00452042011638252,
0.00737614095179629));
#39172=CARTESIAN_POINT('Origin',(-0.203567794470365,0.00749999935701362,
0.000977046461186483));
#39173=CARTESIAN_POINT('',(-0.203099755569153,0.00751239992371187,0.0102033423261815));
#39174=CARTESIAN_POINT('',(-0.203180925911572,0.00274255958650594,0.00887885017805646));
#39175=CARTESIAN_POINT('Ctrl Pts',(-0.203180925911572,0.00274255958650594,
0.00887885017805646));
#39176=CARTESIAN_POINT('Ctrl Pts',(-0.203144430180515,0.00297855990713514,
0.00902006318418588));
#39177=CARTESIAN_POINT('Ctrl Pts',(-0.203099100468265,0.00329328958382362,
0.00918815539817035));
#39178=CARTESIAN_POINT('Ctrl Pts',(-0.203054332460607,0.00365027651704815,
0.00935661910300519));
#39179=CARTESIAN_POINT('Ctrl Pts',(-0.203033957671154,0.00382624548473899,
0.00943519574639222));
#39180=CARTESIAN_POINT('Ctrl Pts',(-0.203004894631343,0.0041419656001032,
0.00956548767658879));
#39181=CARTESIAN_POINT('Ctrl Pts',(-0.202980280894576,0.00452088750482505,
0.00970547640495058));
#39182=CARTESIAN_POINT('Ctrl Pts',(-0.202964648697527,0.00503857041836433,
0.00986783483593268));
#39183=CARTESIAN_POINT('Ctrl Pts',(-0.20297036150819,0.00550510267309646,
0.00998125540777899));
#39184=CARTESIAN_POINT('Ctrl Pts',(-0.202983860319937,0.00587653496273335,
0.0100526595036212));
#39185=CARTESIAN_POINT('Ctrl Pts',(-0.202993842688538,0.00608408581120754,
0.010087118293265));
#39186=CARTESIAN_POINT('Ctrl Pts',(-0.203004352694453,0.00626908343786698,
0.0101139235131616));
#39187=CARTESIAN_POINT('Ctrl Pts',(-0.203010023447602,0.00635758963013911,
0.0101253105115554));
#39188=CARTESIAN_POINT('Ctrl Pts',(-0.203021614388977,0.00653051337351625,
0.0101461407131562));
#39189=CARTESIAN_POINT('Ctrl Pts',(-0.203045798331806,0.00685963984035563,
0.0101784216117505));
#39190=CARTESIAN_POINT('Ctrl Pts',(-0.203075452970359,0.00722429942668557,
0.0101975556471434));
#39191=CARTESIAN_POINT('Ctrl Pts',(-0.203099127134863,0.00749962060040461,
0.0101980805626216));
#39192=CARTESIAN_POINT('',(-0.203173150554077,0.0122530887858704,0.00888129623516349));
#39193=CARTESIAN_POINT('Ctrl Pts',(-0.203103859230808,0.00751546179966354,
0.0101981702831522));
#39194=CARTESIAN_POINT('Ctrl Pts',(-0.203056775223463,0.00789820782417455,
0.0101965072528155));
#39195=CARTESIAN_POINT('Ctrl Pts',(-0.203021238778556,0.00828462825544898,
0.0101712805771079));
#39196=CARTESIAN_POINT('Ctrl Pts',(-0.202934392060027,0.00973750097566171,
0.00998326665784201));
#39197=CARTESIAN_POINT('Ctrl Pts',(-0.20296540424907,0.0107807607669583,
0.00966106303167944));
#39198=CARTESIAN_POINT('Ctrl Pts',(-0.203118299904493,0.0119203561347129,
0.00907304555521591));
#39199=CARTESIAN_POINT('Ctrl Pts',(-0.203144199565202,0.0120881563723461,
0.00897978675739302));
#39200=CARTESIAN_POINT('Ctrl Pts',(-0.203173149226216,0.0122530889570464,
0.00888129613151275));
#39201=CARTESIAN_POINT('',(-0.204179780874563,0.012253032433249,0.00890317356958328));
#39202=CARTESIAN_POINT('Ctrl Pts',(-0.203173153192913,0.0122530883967066,
0.00888129655433334));
#39203=CARTESIAN_POINT('Ctrl Pts',(-0.203511932509764,0.0122530694823888,
0.00888865928521167));
#39204=CARTESIAN_POINT('Ctrl Pts',(-0.203847729433473,0.0122530549450459,
0.00889595466893973));
#39205=CARTESIAN_POINT('Ctrl Pts',(-0.204179836434326,0.0122530445711258,
0.00890316748087414));
#39206=CARTESIAN_POINT('',(-0.204098748533723,0.00749980191224963,0.0102197690721754));
#39207=CARTESIAN_POINT('Ctrl Pts',(-0.204179780874563,0.012253032433249,
0.00890317356958328));
#39208=CARTESIAN_POINT('Ctrl Pts',(-0.204143461050771,0.0120171892546894,
0.00904411661106718));
#39209=CARTESIAN_POINT('Ctrl Pts',(-0.204098317379387,0.0117026096193404,
0.00921193526686398));
#39210=CARTESIAN_POINT('Ctrl Pts',(-0.204053625025722,0.011345447823741,
0.00938026087496657));
#39211=CARTESIAN_POINT('Ctrl Pts',(-0.204033257590342,0.011169438898885,
0.00945875526541203));
#39212=CARTESIAN_POINT('Ctrl Pts',(-0.20400400644035,0.0108526182110254,
0.0095892955380159));
#39213=CARTESIAN_POINT('Ctrl Pts',(-0.203979232931866,0.010473412739609,
0.00972905581782053));
#39214=CARTESIAN_POINT('Ctrl Pts',(-0.203963398504837,0.00995938769060063,
0.00989005736630761));
#39215=CARTESIAN_POINT('Ctrl Pts',(-0.203968966224995,0.00948972602499641,
0.0100040791989076));
#39216=CARTESIAN_POINT('Ctrl Pts',(-0.203982474968269,0.00911908695810915,
0.0100751001999791));
#39217=CARTESIAN_POINT('Ctrl Pts',(-0.203992485231315,0.00891210336567303,
0.0101093719543023));
#39218=CARTESIAN_POINT('Ctrl Pts',(-0.204003028710727,0.00872797162306478,
0.0101359840652107));
#39219=CARTESIAN_POINT('Ctrl Pts',(-0.20400874394351,0.00863961277180208,
0.0101473278130879));
#39220=CARTESIAN_POINT('Ctrl Pts',(-0.204020424813096,0.00846714164179978,
0.0101680546246225));
#39221=CARTESIAN_POINT('Ctrl Pts',(-0.204044836153723,0.00813870113222504,
0.0102001979821628));
#39222=CARTESIAN_POINT('Ctrl Pts',(-0.204074808586391,0.00777469146557797,
0.0102192556370909));
#39223=CARTESIAN_POINT('Ctrl Pts',(-0.204098748532138,0.00749980199044204,
0.0102197690721427));
#39224=CARTESIAN_POINT('',(-0.204181203653622,0.00274295112565268,0.00890078565278145));
#39225=CARTESIAN_POINT('Ctrl Pts',(-0.204098748533723,0.00749980191224963,
0.0102197690721754));
#39226=CARTESIAN_POINT('Ctrl Pts',(-0.204074880929372,0.00722376251075426,
0.0102192452129123));
#39227=CARTESIAN_POINT('Ctrl Pts',(-0.204045011657587,0.0068582828311219,
0.0102000235115584));
#39228=CARTESIAN_POINT('Ctrl Pts',(-0.204020697069231,0.00652849968391289,
0.0101676045847285));
#39229=CARTESIAN_POINT('Ctrl Pts',(-0.204009076078799,0.00635546295071101,
0.0101467226518613));
#39230=CARTESIAN_POINT('Ctrl Pts',(-0.204003375631308,0.00626651305530474,
0.0101352488071801));
#39231=CARTESIAN_POINT('Ctrl Pts',(-0.20399294897216,0.00608271596521517,
0.0101085755847959));
#39232=CARTESIAN_POINT('Ctrl Pts',(-0.203983037889796,0.00587591892958034,
0.0100742185056347));
#39233=CARTESIAN_POINT('Ctrl Pts',(-0.203969676391244,0.0055058961751446,
0.0100031125965096));
#39234=CARTESIAN_POINT('Ctrl Pts',(-0.203964190242521,0.00503729302673557,
0.00988910976652827));
#39235=CARTESIAN_POINT('Ctrl Pts',(-0.203979910998399,0.00452522540899178,
0.00972857991125269));
#39236=CARTESIAN_POINT('Ctrl Pts',(-0.204004528322486,0.00414749332803605,
0.00958931999877319));
#39237=CARTESIAN_POINT('Ctrl Pts',(-0.204033478477464,0.00383291015267278,
0.00945976525310406));
#39238=CARTESIAN_POINT('Ctrl Pts',(-0.204053978965976,0.00365549874924138,
0.00938071761359606));
#39239=CARTESIAN_POINT('Ctrl Pts',(-0.204098931566298,0.00329690411269798,
0.00921173427308648));
#39240=CARTESIAN_POINT('Ctrl Pts',(-0.204144505573565,0.00298031101002354,
0.00904279652424585));
#39241=CARTESIAN_POINT('Ctrl Pts',(-0.204181203653622,0.00274295112565268,
0.00890078565278145));
#39242=CARTESIAN_POINT('Ctrl Pts',(-0.204181260022187,0.00274294282639214,
0.00890078188239789));
#39243=CARTESIAN_POINT('Ctrl Pts',(-0.203847886509956,0.00274281850013204,
0.00889347492067281));
#39244=CARTESIAN_POINT('Ctrl Pts',(-0.203514399366426,0.00274269020994476,
0.00888616310506232));
#39245=CARTESIAN_POINT('Ctrl Pts',(-0.203181006275248,0.00274255803686494,
0.00887885098901425));
#39246=CARTESIAN_POINT('Origin',(-0.205569658041737,0.00749999947180197,
0.00105479137718579));
#39247=CARTESIAN_POINT('',(-0.205098436723926,0.00749984710325509,0.0102432567628741));
#39248=CARTESIAN_POINT('',(-0.205181476923035,0.00274471358820867,0.00891990256930596));
#39249=CARTESIAN_POINT('Ctrl Pts',(-0.205181476923035,0.00274471358820867,
0.00891990256930596));
#39250=CARTESIAN_POINT('Ctrl Pts',(-0.205144999435084,0.00298046276772295,
0.0090615603243642));
#39251=CARTESIAN_POINT('Ctrl Pts',(-0.205099653927717,0.00329494512090687,
0.00923020959913407));
#39252=CARTESIAN_POINT('Ctrl Pts',(-0.205054727115499,0.00365205955154019,
0.00939936791908314));
#39253=CARTESIAN_POINT('Ctrl Pts',(-0.205034265565039,0.00382779147629106,
0.00947814183092217));
#39254=CARTESIAN_POINT('Ctrl Pts',(-0.20500474207185,0.00414512155714752,
0.0096095461180496));
#39255=CARTESIAN_POINT('Ctrl Pts',(-0.204979716812682,0.00452455957091514,
0.00975004056260158));
#39256=CARTESIAN_POINT('Ctrl Pts',(-0.204963626367347,0.00503777155002916,
0.00991158317344809));
#39257=CARTESIAN_POINT('Ctrl Pts',(-0.204969004327107,0.00550889290724541,
0.0100265106819687));
#39258=CARTESIAN_POINT('Ctrl Pts',(-0.20498237769071,0.00587963241517032,
0.010097851465535));
#39259=CARTESIAN_POINT('Ctrl Pts',(-0.204992318269195,0.00608664949133323,
0.0101322804306265));
#39260=CARTESIAN_POINT('Ctrl Pts',(-0.20500279780342,0.00627066364792692,
0.010158996492799));
#39261=CARTESIAN_POINT('Ctrl Pts',(-0.205008498650806,0.00635916355663372,
0.0101704121841367));
#39262=CARTESIAN_POINT('Ctrl Pts',(-0.205020149004397,0.00653174744369742,
0.010191247580515));
#39263=CARTESIAN_POINT('Ctrl Pts',(-0.205044527128556,0.00686045861570371,
0.0102235677823509));
#39264=CARTESIAN_POINT('Ctrl Pts',(-0.20507449102882,0.00722474579493575,
0.010242732314049));
#39265=CARTESIAN_POINT('Ctrl Pts',(-0.205098436838663,0.00749984638114644,
0.0102432567656874));
#39266=CARTESIAN_POINT('',(-0.205180383787346,0.0122514622743969,0.0089221865607949));
#39267=CARTESIAN_POINT('Ctrl Pts',(-0.205098436789953,0.0074998471090431,
0.0102432567646418));
#39268=CARTESIAN_POINT('Ctrl Pts',(-0.205074354603187,0.00777471924233373,
0.0102427384211593));
#39269=CARTESIAN_POINT('Ctrl Pts',(-0.205044224088182,0.00813868908844073,
0.0102236143681364));
#39270=CARTESIAN_POINT('Ctrl Pts',(-0.205019718722386,0.00846712890458327,
0.0101913547215864));
#39271=CARTESIAN_POINT('Ctrl Pts',(-0.205008014898611,0.00863952563124892,
0.010170565224802));
#39272=CARTESIAN_POINT('Ctrl Pts',(-0.205002283639176,0.00872803405528101,
0.0101591583475927));
#39273=CARTESIAN_POINT('Ctrl Pts',(-0.204991783191973,0.00891153024400615,
0.0101325492799381));
#39274=CARTESIAN_POINT('Ctrl Pts',(-0.204981823379621,0.00911820648575059,
0.0100982161433639));
#39275=CARTESIAN_POINT('Ctrl Pts',(-0.204968402235169,0.00948813798704052,
0.0100272030886554));
#39276=CARTESIAN_POINT('Ctrl Pts',(-0.204963285734911,0.00996204771265651,
0.0099113204303612));
#39277=CARTESIAN_POINT('Ctrl Pts',(-0.204978679135674,0.0104671708457599,
0.0097533572650039));
#39278=CARTESIAN_POINT('Ctrl Pts',(-0.205001872942925,0.0108105532641061,
0.00962546665935062));
#39279=CARTESIAN_POINT('Ctrl Pts',(-0.205017674322944,0.0109985928831329,
0.00955044853206125));
#39280=CARTESIAN_POINT('Ctrl Pts',(-0.205033320565654,0.0111580504126392,
0.00948319462115217));
#39281=CARTESIAN_POINT('Ctrl Pts',(-0.20504249987871,0.0112415438927982,
0.00944652284227898));
#39282=CARTESIAN_POINT('Ctrl Pts',(-0.205060574645265,0.0113979299630055,
0.00937617119624099));
#39283=CARTESIAN_POINT('Ctrl Pts',(-0.205098289295843,0.0116949803514041,
0.00923470790117257));
#39284=CARTESIAN_POINT('Ctrl Pts',(-0.205144065972417,0.012015827840092,
0.00906362218301645));
#39285=CARTESIAN_POINT('Ctrl Pts',(-0.205180383787346,0.0122514622743969,
0.0089221865607949));
#39286=CARTESIAN_POINT('',(-0.206180937657661,0.0122515141026534,0.00894388147634254));
#39287=CARTESIAN_POINT('Ctrl Pts',(-0.205180453611888,0.0122514588177548,
0.00892219016333599));
#39288=CARTESIAN_POINT('Ctrl Pts',(-0.205511148871274,0.0122514771336389,
0.00892935988179134));
#39289=CARTESIAN_POINT('Ctrl Pts',(-0.205844866014664,0.0122514995001858,
0.00893659277298742));
#39290=CARTESIAN_POINT('Ctrl Pts',(-0.206180987661044,0.0122515260700969,
0.00894387533870355));
#39291=CARTESIAN_POINT('',(-0.206098158559683,0.00749989366550756,0.0102649624274855));
#39292=CARTESIAN_POINT('Ctrl Pts',(-0.206180937657661,0.0122515141026534,
0.00894388147634254));
#39293=CARTESIAN_POINT('Ctrl Pts',(-0.206144660866419,0.0120160183041278,
0.009085236259632));
#39294=CARTESIAN_POINT('Ctrl Pts',(-0.206098899870945,0.01169524993866,
0.00925629857313019));
#39295=CARTESIAN_POINT('Ctrl Pts',(-0.206061132361365,0.0113980780373007,
0.00939782966776102));
#39296=CARTESIAN_POINT('Ctrl Pts',(-0.20604299822031,0.0112415087259796,
0.00946826283096089));
#39297=CARTESIAN_POINT('Ctrl Pts',(-0.206033784421152,0.0111579602868827,
0.00950495948634835));
#39298=CARTESIAN_POINT('Ctrl Pts',(-0.20601801307969,0.0109979583047259,
0.00957243326902137));
#39299=CARTESIAN_POINT('Ctrl Pts',(-0.206002083351523,0.0108095769841854,
0.00964756592446938));
#39300=CARTESIAN_POINT('Ctrl Pts',(-0.205978663196826,0.0104657148947248,
0.0097755526521527));
#39301=CARTESIAN_POINT('Ctrl Pts',(-0.205962991007194,0.00996284049211284,
0.00993280311124859));
#39302=CARTESIAN_POINT('Ctrl Pts',(-0.205967866525693,0.00948672058736224,
0.010049230644559));
#39303=CARTESIAN_POINT('Ctrl Pts',(-0.205981177868757,0.00911719678861053,
0.0101200908184433));
#39304=CARTESIAN_POINT('Ctrl Pts',(-0.205991090210523,0.00891083408445435,
0.0101543521708114));
#39305=CARTESIAN_POINT('Ctrl Pts',(-0.206001553448915,0.00872784553293601,
0.010180878134153));
#39306=CARTESIAN_POINT('Ctrl Pts',(-0.206007285858683,0.0086394365338037,
0.0101922726253234));
#39307=CARTESIAN_POINT('Ctrl Pts',(-0.206019006109483,0.00846724868623852,
0.0102130367903869));
#39308=CARTESIAN_POINT('Ctrl Pts',(-0.206043602684669,0.00813897561664646,
0.0102452907826911));
#39309=CARTESIAN_POINT('Ctrl Pts',(-0.206073911555016,0.00777492913360827,
0.0102644392378273));
#39310=CARTESIAN_POINT('Ctrl Pts',(-0.206098158559595,0.00749989366551524,
0.0102649624274836));
#39311=CARTESIAN_POINT('',(-0.206181705500482,0.00274489174553523,0.00894172441120622));
#39312=CARTESIAN_POINT('Ctrl Pts',(-0.206098158559683,0.00749989366550756,
0.0102649624274855));
#39313=CARTESIAN_POINT('Ctrl Pts',(-0.206073959098662,0.00722364355886157,
0.0102644337474957));
#39314=CARTESIAN_POINT('Ctrl Pts',(-0.206043716980217,0.00685803736171764,
0.0102451182414761));
#39315=CARTESIAN_POINT('Ctrl Pts',(-0.206019177562163,0.00652833493064124,
0.0102125773260753));
#39316=CARTESIAN_POINT('Ctrl Pts',(-0.206007493409607,0.00635553275105125,
0.0101916493844423));
#39317=CARTESIAN_POINT('Ctrl Pts',(-0.206001762741477,0.00626650822424718,
0.010180120236742));
#39318=CARTESIAN_POINT('Ctrl Pts',(-0.205991386078031,0.00608379417233497,
0.0101535194432339));
#39319=CARTESIAN_POINT('Ctrl Pts',(-0.20598153359865,0.00587762722169114,
0.0101191755144898));
#39320=CARTESIAN_POINT('Ctrl Pts',(-0.205968325976292,0.00550849646880288,
0.0100481105257598));
#39321=CARTESIAN_POINT('Ctrl Pts',(-0.205963195332645,0.00503604973694923,
0.00993274520514876));
#39322=CARTESIAN_POINT('Ctrl Pts',(-0.205979390899299,0.00452804773636262,
0.00977287900430854));
#39323=CARTESIAN_POINT('Ctrl Pts',(-0.20600443701926,0.00414976611457223,
0.00963305573502386));
#39324=CARTESIAN_POINT('Ctrl Pts',(-0.20603386541523,0.0038335282789123,
0.00950233649648007));
#39325=CARTESIAN_POINT('Ctrl Pts',(-0.206054458420243,0.00365634684123214,
0.0094230617805734));
#39326=CARTESIAN_POINT('Ctrl Pts',(-0.20609954285163,0.00329779903994257,
0.00925341710486629));
#39327=CARTESIAN_POINT('Ctrl Pts',(-0.206145078217534,0.00298174438244053,
0.00908403851963943));
#39328=CARTESIAN_POINT('Ctrl Pts',(-0.206181705500482,0.00274489174553523,
0.00894172441120622));
#39329=CARTESIAN_POINT('Ctrl Pts',(-0.206181756662732,0.00274488347523256,
0.00894172052487549));
#39330=CARTESIAN_POINT('Ctrl Pts',(-0.205849126200276,0.00274483042692363,
0.00893446732041925));
#39331=CARTESIAN_POINT('Ctrl Pts',(-0.205515617123526,0.00274477344911426,
0.00892719266697236));
#39332=CARTESIAN_POINT('Ctrl Pts',(-0.205181550495496,0.00274471254920856,
0.00891990353869956));
#39333=CARTESIAN_POINT('Origin',(-0.207569521557474,0.00749999958288434,
0.00113169766824726));
#39334=CARTESIAN_POINT('',(-0.20709777676797,0.00750000074588895,0.0102884318050736));
#39335=CARTESIAN_POINT('',(-0.207182008644929,0.00274682078388386,0.0089610216724757));
#39336=CARTESIAN_POINT('Ctrl Pts',(-0.207182008644929,0.00274682078388386,
0.0089610216724757));
#39337=CARTESIAN_POINT('Ctrl Pts',(-0.207145575477217,0.00298221862702531,
0.00910305394454891));
#39338=CARTESIAN_POINT('Ctrl Pts',(-0.207114932447028,0.00319598750884428,
0.00921768338570113));
#39339=CARTESIAN_POINT('Ctrl Pts',(-0.20709026641563,0.00338043799469262,
0.00930998443979783));
#39340=CARTESIAN_POINT('Ctrl Pts',(-0.207077933399932,0.00347266323761681,
0.00935613496684619));
#39341=CARTESIAN_POINT('Ctrl Pts',(-0.207067094216487,0.0035575471412094,
0.0093967226125637));
#39342=CARTESIAN_POINT('Ctrl Pts',(-0.207057405036147,0.0036379865399805,
0.00943389841659064));
#39343=CARTESIAN_POINT('Ctrl Pts',(-0.207052560445977,0.00367820623936605,
0.00945248631860411));
#39344=CARTESIAN_POINT('Ctrl Pts',(-0.20704800397913,0.00371732864609859,
0.00947019260412138));
#39345=CARTESIAN_POINT('Ctrl Pts',(-0.20704418523739,0.00375081558048865,
0.00948512581363911));
#39346=CARTESIAN_POINT('Ctrl Pts',(-0.20704036649565,0.00378430251487872,
0.00950005902315684));
#39347=CARTESIAN_POINT('Ctrl Pts',(-0.207037283499954,0.00381211261975297,
0.00951231025313473));
#39348=CARTESIAN_POINT('Ctrl Pts',(-0.207033092445885,0.00385268931337077,
0.00952982555512431));
#39349=CARTESIAN_POINT('Ctrl Pts',(-0.207028901391817,0.00389326600698857,
0.0095473408571139));
#39350=CARTESIAN_POINT('Ctrl Pts',(-0.20702360583578,0.00394668069240661,
0.00956995652994313));
#39351=CARTESIAN_POINT('Ctrl Pts',(-0.207018954045241,0.00399696732814934,
0.00959066061121586));
#39352=CARTESIAN_POINT('Ctrl Pts',(-0.207014302254701,0.00404725396389208,
0.0096113646924886));
#39353=CARTESIAN_POINT('Ctrl Pts',(-0.207010291748562,0.00409436609404158,
0.00963027138650139));
#39354=CARTESIAN_POINT('Ctrl Pts',(-0.207006494295823,0.00414215515037163,
0.00964901097839348));
#39355=CARTESIAN_POINT('Ctrl Pts',(-0.206998899390345,0.00423773326303174,
0.00968649016217763));
#39356=CARTESIAN_POINT('Ctrl Pts',(-0.206992159164313,0.00433605953714399,
0.00972318743619733));
#39357=CARTESIAN_POINT('Ctrl Pts',(-0.206986611713382,0.00443508121932275,
0.00975821336343698));
#39358=CARTESIAN_POINT('Ctrl Pts',(-0.20697551681152,0.00463312458368026,
0.00982826521791629));
#39359=CARTESIAN_POINT('Ctrl Pts',(-0.206969194341382,0.00483399433937503,
0.00989157040197803));
#39360=CARTESIAN_POINT('Ctrl Pts',(-0.20696699998225,0.00502987816024672,
0.00994635944260401));
#39361=CARTESIAN_POINT('Ctrl Pts',(-0.206964805623117,0.00522576198111841,
0.01000114848323));
#39362=CARTESIAN_POINT('Ctrl Pts',(-0.206966726835597,0.0054164844159352,
0.0100479985563706));
#39363=CARTESIAN_POINT('Ctrl Pts',(-0.206972408255633,0.00562088128514229,
0.0100909504821526));
#39364=CARTESIAN_POINT('Ctrl Pts',(-0.206975248965651,0.00572307971974584,
0.0101124264450436));
#39365=CARTESIAN_POINT('Ctrl Pts',(-0.206979033308164,0.00582873120607272,
0.0101327630618226));
#39366=CARTESIAN_POINT('Ctrl Pts',(-0.206983588792974,0.00593280052031057,
0.0101509283408082));
#39367=CARTESIAN_POINT('Ctrl Pts',(-0.206985866535379,0.0059848351774295,
0.010160010980301));
#39368=CARTESIAN_POINT('Ctrl Pts',(-0.206988336095,0.00603646618332007,
0.0101685953570537));
#39369=CARTESIAN_POINT('Ctrl Pts',(-0.206991307383632,0.00609278624748642,
0.0101774134158557));
#39370=CARTESIAN_POINT('Ctrl Pts',(-0.206994278672263,0.00614910631165276,
0.0101862314746577));
#39371=CARTESIAN_POINT('Ctrl Pts',(-0.206997755000619,0.00621013982597531,
0.0101951308300653));
#39372=CARTESIAN_POINT('Ctrl Pts',(-0.207000448457267,0.00625541611911697,
0.0102013968217338));
#39373=CARTESIAN_POINT('Ctrl Pts',(-0.207003141913915,0.00630069241225863,
0.0102076628134023));
#39374=CARTESIAN_POINT('Ctrl Pts',(-0.207005047888527,0.00633018297254175,
0.0102115076445645));
#39375=CARTESIAN_POINT('Ctrl Pts',(-0.207007462395225,0.00636646234232639,
0.0102160830445708));
#39376=CARTESIAN_POINT('Ctrl Pts',(-0.207009876901922,0.00640274171211104,
0.0102206584445771));
#39377=CARTESIAN_POINT('Ctrl Pts',(-0.207012802402609,0.00644582342611286,
0.0102258510976829));
#39378=CARTESIAN_POINT('Ctrl Pts',(-0.207015923228053,0.00649018925995671,
0.0102308383765914));
#39379=CARTESIAN_POINT('Ctrl Pts',(-0.207022164878943,0.00657892092764439,
0.0102408129344084));
#39380=CARTESIAN_POINT('Ctrl Pts',(-0.207029184722482,0.00667277538880603,
0.0102501089745481));
#39381=CARTESIAN_POINT('Ctrl Pts',(-0.20703723126043,0.00677582274945741,
0.0102584537446242));
#39382=CARTESIAN_POINT('Ctrl Pts',(-0.207053324334665,0.00698191744947961,
0.010275143283053));
#39383=CARTESIAN_POINT('Ctrl Pts',(-0.20707352685292,0.00722478486283655,
0.0102879049777361));
#39384=CARTESIAN_POINT('Ctrl Pts',(-0.207097776722938,0.00749999991179089,
0.0102884318038818));
#39385=CARTESIAN_POINT('',(-0.20718151084421,0.0122499348362438,0.00896297700837428));
#39386=CARTESIAN_POINT('Ctrl Pts',(-0.207097776664925,0.00750000073675634,
0.0102884318026212));
#39387=CARTESIAN_POINT('Ctrl Pts',(-0.207073415449424,0.00777501615170926,
0.0102879024570678));
#39388=CARTESIAN_POINT('Ctrl Pts',(-0.207042984455933,0.00813902360000427,
0.0102686867749524));
#39389=CARTESIAN_POINT('Ctrl Pts',(-0.207018325616829,0.00846728489363423,
0.0102363188518694));
#39390=CARTESIAN_POINT('Ctrl Pts',(-0.207006597174583,0.00863941228212482,
0.0102154905383654));
#39391=CARTESIAN_POINT('Ctrl Pts',(-0.207000859433949,0.00872792628559308,
0.0102040402212881));
#39392=CARTESIAN_POINT('Ctrl Pts',(-0.206990444167153,0.00891044623298851,
0.0101774926917494));
#39393=CARTESIAN_POINT('Ctrl Pts',(-0.206980584381931,0.00911656578521641,
0.0101431628687521));
#39394=CARTESIAN_POINT('Ctrl Pts',(-0.206967386735522,0.00948571707073339,
0.0100721765704815));
#39395=CARTESIAN_POINT('Ctrl Pts',(-0.20696272620052,0.00996376203546202,
0.00995482693936122));
#39396=CARTESIAN_POINT('Ctrl Pts',(-0.206978636730251,0.0104642557690517,
0.00979773389759007));
#39397=CARTESIAN_POINT('Ctrl Pts',(-0.207002273125407,0.0108084189656327,
0.00966921478300733));
#39398=CARTESIAN_POINT('Ctrl Pts',(-0.207018324368728,0.0109970008490617,
0.00959372828534347));
#39399=CARTESIAN_POINT('Ctrl Pts',(-0.207034226461458,0.0111575074984121,
0.00952578095182555));
#39400=CARTESIAN_POINT('Ctrl Pts',(-0.207043446318233,0.0112407737564283,
0.00948906068501107));
#39401=CARTESIAN_POINT('Ctrl Pts',(-0.207061625861014,0.0113972450779469,
0.00941839667616617));
#39402=CARTESIAN_POINT('Ctrl Pts',(-0.207099440341916,0.0116941168274847,
0.00927644448342378));
#39403=CARTESIAN_POINT('Ctrl Pts',(-0.207145227178358,0.0120146497717542,
0.00910481081580588));
#39404=CARTESIAN_POINT('Ctrl Pts',(-0.20718151084421,0.0122499348362438,
0.00896297700837428));
#39405=CARTESIAN_POINT('',(-0.208182029839437,0.0122499766833686,0.0089846914473168));
#39406=CARTESIAN_POINT('Ctrl Pts',(-0.207181573897133,0.0122499313680481,
0.00896298048072855));
#39407=CARTESIAN_POINT('Ctrl Pts',(-0.207511997686088,0.0122499464756022,
0.00897015094572272));
#39408=CARTESIAN_POINT('Ctrl Pts',(-0.207845716051498,0.0122499654803498,
0.0089773906346182));
#39409=CARTESIAN_POINT('Ctrl Pts',(-0.208182074796062,0.0122499885499931,
0.00898468523090216));
#39410=CARTESIAN_POINT('',(-0.208097511648441,0.0075000000097323,0.0103101525084975));
#39411=CARTESIAN_POINT('Ctrl Pts',(-0.208182029839437,0.0122499766833686,
0.0089846914473168));
#39412=CARTESIAN_POINT('Ctrl Pts',(-0.208145792855726,0.0120148330456536,
0.00912644211787466));
#39413=CARTESIAN_POINT('Ctrl Pts',(-0.208115282833245,0.0118012225403462,
0.00924089818765459));
#39414=CARTESIAN_POINT('Ctrl Pts',(-0.208090691592793,0.0116168440875562,
0.0093330878093222));
#39415=CARTESIAN_POINT('Ctrl Pts',(-0.208078395972566,0.0115246548611613,
0.00937918262015601));
#39416=CARTESIAN_POINT('Ctrl Pts',(-0.208067579614742,0.01143978576553,
0.00941973075151924));
#39417=CARTESIAN_POINT('Ctrl Pts',(-0.208057894473467,0.0113593052267618,
0.00945689384554209));
#39418=CARTESIAN_POINT('Ctrl Pts',(-0.208053051902829,0.0113190649573777,
0.00947547539255351));
#39419=CARTESIAN_POINT('Ctrl Pts',(-0.208048492764793,0.0112799078747642,
0.00949318175625101));
#39420=CARTESIAN_POINT('Ctrl Pts',(-0.208044672538954,0.0112464177413264,
0.00950810304976068));
#39421=CARTESIAN_POINT('Ctrl Pts',(-0.208040852313116,0.0112129276078887,
0.00952302434327035));
#39422=CARTESIAN_POINT('Ctrl Pts',(-0.208037768998231,0.011185146207607,
0.0095352526709192));
#39423=CARTESIAN_POINT('Ctrl Pts',(-0.208033554813732,0.0111444421187781,
0.0095528062343153));
#39424=CARTESIAN_POINT('Ctrl Pts',(-0.208029340629233,0.0111037380299492,
0.00957035979771141));
#39425=CARTESIAN_POINT('Ctrl Pts',(-0.208023999188475,0.0110500387683215,
0.00959307229688317));
#39426=CARTESIAN_POINT('Ctrl Pts',(-0.20801930739809,0.0109995533354734,
0.00961383345579642));
#39427=CARTESIAN_POINT('Ctrl Pts',(-0.208014615607705,0.0109490679026253,
0.00963459461470967));
#39428=CARTESIAN_POINT('Ctrl Pts',(-0.208010570935794,0.0109018436683241,
0.00965352096117992));
#39429=CARTESIAN_POINT('Ctrl Pts',(-0.208006738138096,0.0108539525564452,
0.00967227472359561));
#39430=CARTESIAN_POINT('Ctrl Pts',(-0.207999072542699,0.0107581703326874,
0.009709782248427));
#39431=CARTESIAN_POINT('Ctrl Pts',(-0.207992257022405,0.0106596778635927,
0.00974648077505833));
#39432=CARTESIAN_POINT('Ctrl Pts',(-0.20798663414025,0.0105608119821825,
0.00978139682654719));
#39433=CARTESIAN_POINT('Ctrl Pts',(-0.207975388375939,0.0103630802193621,
0.00985122892952491));
#39434=CARTESIAN_POINT('Ctrl Pts',(-0.207968912875204,0.0101638391044602,
0.00991394443523984));
#39435=CARTESIAN_POINT('Ctrl Pts',(-0.207966563520788,0.00996813660690527,
0.00996863187517243));
#39436=CARTESIAN_POINT('Ctrl Pts',(-0.207964214166371,0.00977243410935032,
0.010023319315105));
#39437=CARTESIAN_POINT('Ctrl Pts',(-0.207965981064406,0.00958041158679767,
0.0100704340503291));
#39438=CARTESIAN_POINT('Ctrl Pts',(-0.207971550318033,0.00937594739075353,
0.0101133221912404));
#39439=CARTESIAN_POINT('Ctrl Pts',(-0.207974334944846,0.00927371529273146,
0.0101347662616961));
#39440=CARTESIAN_POINT('Ctrl Pts',(-0.207978073340098,0.00916834167558793,
0.0101550073443192));
#39441=CARTESIAN_POINT('Ctrl Pts',(-0.207982591228724,0.00906458569967766,
0.0101730864752584));
#39442=CARTESIAN_POINT('Ctrl Pts',(-0.207984850173036,0.00901270771172253,
0.010182126040728));
#39443=CARTESIAN_POINT('Ctrl Pts',(-0.207987303053134,0.0089612420508267,
0.0101906682698402));
#39444=CARTESIAN_POINT('Ctrl Pts',(-0.207990257022641,0.00890517318126005,
0.0101994339730368));
#39445=CARTESIAN_POINT('Ctrl Pts',(-0.207993210992147,0.0088491043116934,
0.0102081996762335));
#39446=CARTESIAN_POINT('Ctrl Pts',(-0.207996669304785,0.00878840827953629,
0.0102170390987288));
#39447=CARTESIAN_POINT('Ctrl Pts',(-0.20799935633465,0.00874331456968449,
0.0102232734971157));
#39448=CARTESIAN_POINT('Ctrl Pts',(-0.208002043364514,0.0086982208598327,
0.0102295078955026));
#39449=CARTESIAN_POINT('Ctrl Pts',(-0.208003954567205,0.00866875755870705,
0.0102333464296309));
#39450=CARTESIAN_POINT('Ctrl Pts',(-0.208006377063033,0.00863253933496215,
0.0102379103435317));
#39451=CARTESIAN_POINT('Ctrl Pts',(-0.208008799558861,0.00859632111121726,
0.0102424742574324));
#39452=CARTESIAN_POINT('Ctrl Pts',(-0.208011735782999,0.00855333458415877,
0.010247651469918));
#39453=CARTESIAN_POINT('Ctrl Pts',(-0.208014872254183,0.00850905162177827,
0.0102526261647438));
#39454=CARTESIAN_POINT('Ctrl Pts',(-0.208021145196552,0.00842048569701728,
0.0102625755543955));
#39455=CARTESIAN_POINT('Ctrl Pts',(-0.208028216050051,0.00832674758329316,
0.0102718564983692));
#39456=CARTESIAN_POINT('Ctrl Pts',(-0.208036331741941,0.00822380066238706,
0.0102801905377563));
#39457=CARTESIAN_POINT('Ctrl Pts',(-0.208052563125722,0.00801790682057488,
0.0102968586165304));
#39458=CARTESIAN_POINT('Ctrl Pts',(-0.208072976460898,0.00777517677190799,
0.01030961950719));
#39459=CARTESIAN_POINT('Ctrl Pts',(-0.208097511648349,0.0075000000097405,
0.0103101525084955));
#39460=CARTESIAN_POINT('',(-0.208182216877932,0.00274693029866322,0.00898281703864054));
#39461=CARTESIAN_POINT('Ctrl Pts',(-0.208097511648441,0.0075000000097323,
0.0103101525084975));
#39462=CARTESIAN_POINT('Ctrl Pts',(-0.208072993965045,0.00722356118992073,
0.0103096197641003));
#39463=CARTESIAN_POINT('Ctrl Pts',(-0.208042400274024,0.00685784507416209,
0.0102902147042539));
#39464=CARTESIAN_POINT('Ctrl Pts',(-0.208017662771516,0.00652823631150515,
0.0102575584516077));
#39465=CARTESIAN_POINT('Ctrl Pts',(-0.208005930920095,0.00635564877914102,
0.0102365846017781));
#39466=CARTESIAN_POINT('Ctrl Pts',(-0.208000182777587,0.00626659133857995,
0.0102250079709892));
#39467=CARTESIAN_POINT('Ctrl Pts',(-0.207989865689244,0.00608477119043111,
0.0101984552495345));
#39468=CARTESIAN_POINT('Ctrl Pts',(-0.20798008310499,0.00587913141808675,
0.0101641066168629));
#39469=CARTESIAN_POINT('Ctrl Pts',(-0.20796704329005,0.00551077955137498,
0.0100930537471372));
#39470=CARTESIAN_POINT('Ctrl Pts',(-0.207962271325726,0.00503494827512439,
0.00997642711268012));
#39471=CARTESIAN_POINT('Ctrl Pts',(-0.207978920836864,0.00453114766412443,
0.00981730821500114));
#39472=CARTESIAN_POINT('Ctrl Pts',(-0.208004383855489,0.00415229827421602,
0.00967694145303679));
#39473=CARTESIAN_POINT('Ctrl Pts',(-0.208034293916788,0.00383415769731894,
0.00954496308351629));
#39474=CARTESIAN_POINT('Ctrl Pts',(-0.208054940986263,0.00365745017531619,
0.00946557676160163));
#39475=CARTESIAN_POINT('Ctrl Pts',(-0.208100143499718,0.00329896113401496,
0.00929530510330588));
#39476=CARTESIAN_POINT('Ctrl Pts',(-0.208145646094477,0.00298337772013156,
0.00912547875455556));
#39477=CARTESIAN_POINT('Ctrl Pts',(-0.208182216877932,0.00274693029866322,
0.00898281703864054));
#39478=CARTESIAN_POINT('Ctrl Pts',(-0.208182263102175,0.00274692209240819,
0.00898281306397055));
#39479=CARTESIAN_POINT('Ctrl Pts',(-0.207850589804928,0.00274689181898717,
0.00897558929414468));
#39480=CARTESIAN_POINT('Ctrl Pts',(-0.207517041324408,0.00274685772814941,
0.00896832247078491));
#39481=CARTESIAN_POINT('Ctrl Pts',(-0.207182075713153,0.00274681975932118,
0.00896102250785583));
#39482=CARTESIAN_POINT('Origin',(-0.209569669966458,0.0074999996646916,
0.00120787420876588));
#39483=CARTESIAN_POINT('',(-0.209097173739288,0.00750003250879847,0.0103336083052934));
#39484=CARTESIAN_POINT('',(-0.209182480741977,0.00274873233260506,0.00900211047042567));
#39485=CARTESIAN_POINT('Ctrl Pts',(-0.209182480741977,0.00274873233260506,
0.00900211047042567));
#39486=CARTESIAN_POINT('Ctrl Pts',(-0.209146100632164,0.00298377716177745,
0.0091445129836625));
#39487=CARTESIAN_POINT('Ctrl Pts',(-0.209115469242561,0.00319733244281788,
0.00925948736122651));
#39488=CARTESIAN_POINT('Ctrl Pts',(-0.209090780763169,0.00338164312408276,
0.00935207775087));
#39489=CARTESIAN_POINT('Ctrl Pts',(-0.209078436523473,0.00347379846471521,
0.00939837294569175));
#39490=CARTESIAN_POINT('Ctrl Pts',(-0.209067577573349,0.00355863035290946,
0.00943909229052956));
#39491=CARTESIAN_POINT('Ctrl Pts',(-0.209057852718374,0.00363908113506117,
0.00947641386394267));
#39492=CARTESIAN_POINT('Ctrl Pts',(-0.209052990290886,0.00367930652613703,
0.00949507465064922));
#39493=CARTESIAN_POINT('Ctrl Pts',(-0.209048412020849,0.00371845076690064,
0.00951285684655249));
#39494=CARTESIAN_POINT('Ctrl Pts',(-0.209044577592333,0.00375191008281231,
0.00952783315673602));
#39495=CARTESIAN_POINT('Ctrl Pts',(-0.209040743163818,0.00378536939872397,
0.00954280946691956));
#39496=CARTESIAN_POINT('Ctrl Pts',(-0.209037650558984,0.00381310148600916,
0.0095550727096917));
#39497=CARTESIAN_POINT('Ctrl Pts',(-0.209033414786212,0.00385381876556008,
0.00957271270229389));
#39498=CARTESIAN_POINT('Ctrl Pts',(-0.209029179013441,0.00389453604511099,
0.00959035269489609));
#39499=CARTESIAN_POINT('Ctrl Pts',(-0.20902380372181,0.00394831201896141,
0.00961320158436462));
#39500=CARTESIAN_POINT('Ctrl Pts',(-0.209019083848898,0.00399885026944767,
0.00963407810398663));
#39501=CARTESIAN_POINT('Ctrl Pts',(-0.209014363975986,0.00404938851993394,
0.00965495462360864));
#39502=CARTESIAN_POINT('Ctrl Pts',(-0.209010296961274,0.00409664094942468,
0.00967397655360619));
#39503=CARTESIAN_POINT('Ctrl Pts',(-0.20900644299565,0.00414455930228565,
0.00969282408903857));
#39504=CARTESIAN_POINT('Ctrl Pts',(-0.208998735064402,0.00424039600800758,
0.00973051915990333));
#39505=CARTESIAN_POINT('Ctrl Pts',(-0.20899188194532,0.00433893998899708,
0.00976739632961011));
#39506=CARTESIAN_POINT('Ctrl Pts',(-0.208986231409264,0.00443780727573967,
0.00980246391163614));
#39507=CARTESIAN_POINT('Ctrl Pts',(-0.208974930337152,0.00463554184922485,
0.00987259907568821));
#39508=CARTESIAN_POINT('Ctrl Pts',(-0.208968439083203,0.00483458168125401,
0.00993551952661447));
#39509=CARTESIAN_POINT('Ctrl Pts',(-0.208966086654309,0.00503022581632468,
0.00999043002591778));
#39510=CARTESIAN_POINT('Ctrl Pts',(-0.208963734225416,0.00522586995139535,
0.0100453405252211));
#39511=CARTESIAN_POINT('Ctrl Pts',(-0.208965510899781,0.0054179784984252,
0.010092688255882));
#39512=CARTESIAN_POINT('Ctrl Pts',(-0.208971085353274,0.00562259743052403,
0.0101357952616566));
#39513=CARTESIAN_POINT('Ctrl Pts',(-0.208973872580021,0.00572490689657345,
0.0101573487645439));
#39514=CARTESIAN_POINT('Ctrl Pts',(-0.208977612437784,0.00583037530970805,
0.0101776955278211));
#39515=CARTESIAN_POINT('Ctrl Pts',(-0.208982132048375,0.005934240640779,
0.0101958705541318));
#39516=CARTESIAN_POINT('Ctrl Pts',(-0.208984391853671,0.00598617330631448,
0.0102049580672871));
#39517=CARTESIAN_POINT('Ctrl Pts',(-0.20898684565277,0.00603769719115068,
0.010213546086111));
#39518=CARTESIAN_POINT('Ctrl Pts',(-0.208989800847266,0.00609384162467977,
0.0102223601272953));
#39519=CARTESIAN_POINT('Ctrl Pts',(-0.208992756041762,0.00614998605820886,
0.0102311741684797));
#39520=CARTESIAN_POINT('Ctrl Pts',(-0.208996215912591,0.00621077528232891,
0.0102400633187187));
#39521=CARTESIAN_POINT('Ctrl Pts',(-0.208998903301093,0.00625592035494135,
0.0102463300512141));
#39522=CARTESIAN_POINT('Ctrl Pts',(-0.209001590689595,0.00630106542755378,
0.0102525967837096));
#39523=CARTESIAN_POINT('Ctrl Pts',(-0.209003501015202,0.00633053794223429,
0.0102564517903237));
#39524=CARTESIAN_POINT('Ctrl Pts',(-0.209005923797116,0.00636677733471289,
0.0102610367039119));
#39525=CARTESIAN_POINT('Ctrl Pts',(-0.209008346579031,0.00640301672719149,
0.0102656216175002));
#39526=CARTESIAN_POINT('Ctrl Pts',(-0.209011284270186,0.00644603652114672,
0.0102708236109892));
#39527=CARTESIAN_POINT('Ctrl Pts',(-0.209014422806348,0.00649035160598153,
0.0102758217619476));
#39528=CARTESIAN_POINT('Ctrl Pts',(-0.209020699878673,0.00657898177565117,
0.0102858180638643));
#39529=CARTESIAN_POINT('Ctrl Pts',(-0.209027777232078,0.00667277941439591,
0.0102951415368914));
#39530=CARTESIAN_POINT('Ctrl Pts',(-0.209035902314636,0.00677579123680547,
0.0103035135477044));
#39531=CARTESIAN_POINT('Ctrl Pts',(-0.209052152478095,0.00698181486062926,
0.0103202575676242));
#39532=CARTESIAN_POINT('Ctrl Pts',(-0.209072596182764,0.00722469622862829,
0.0103330749790414));
#39533=CARTESIAN_POINT('Ctrl Pts',(-0.209097173739288,0.00750003250879847,
0.0103336083052934));
#39534=CARTESIAN_POINT('',(-0.209182595670359,0.0122484553035031,0.00900382443876613));
#39535=CARTESIAN_POINT('Ctrl Pts',(-0.209097173663308,0.00750003352365617,
0.0103336083036377));
#39536=CARTESIAN_POINT('Ctrl Pts',(-0.209072487387346,0.0077752027295915,
0.0103330705552668));
#39537=CARTESIAN_POINT('Ctrl Pts',(-0.20904170611148,0.00813926656432189,
0.0103137660496164));
#39538=CARTESIAN_POINT('Ctrl Pts',(-0.209016870020302,0.00846736255900025,
0.0102812931650683));
#39539=CARTESIAN_POINT('Ctrl Pts',(-0.209005112436531,0.00863924123692276,
0.0102604258946952));
#39540=CARTESIAN_POINT('Ctrl Pts',(-0.208999371395027,0.00872773998646285,
0.0102489367160665));
#39541=CARTESIAN_POINT('Ctrl Pts',(-0.208989042716632,0.00890940175348926,
0.0102224367002035));
#39542=CARTESIAN_POINT('Ctrl Pts',(-0.208979287054889,0.00911503344528391,
0.0101880995138537));
#39543=CARTESIAN_POINT('Ctrl Pts',(-0.20896632173186,0.00948348192094728,
0.0101171239430875));
#39544=CARTESIAN_POINT('Ctrl Pts',(-0.208962145860431,0.00996543922381415,
0.00999835162461839));
#39545=CARTESIAN_POINT('Ctrl Pts',(-0.208978582898474,0.0104611459243631,
0.00984221246132182));
#39546=CARTESIAN_POINT('Ctrl Pts',(-0.209002670041753,0.010806151365008,
0.00971305719239442));
#39547=CARTESIAN_POINT('Ctrl Pts',(-0.209018974214673,0.0109953313838264,
0.00963708637988462));
#39548=CARTESIAN_POINT('Ctrl Pts',(-0.209035136938378,0.0111569767219068,
0.00956840910744746));
#39549=CARTESIAN_POINT('Ctrl Pts',(-0.2090443919497,0.0112400061477328,
0.00953164701243018));
#39550=CARTESIAN_POINT('Ctrl Pts',(-0.2090626715537,0.0113965822320191,
0.00946066576998285));
#39551=CARTESIAN_POINT('Ctrl Pts',(-0.209100573807665,0.0116932888722541,
0.00931822603645342));
#39552=CARTESIAN_POINT('Ctrl Pts',(-0.209146357132706,0.0120135168800619,
0.00914604905715582));
#39553=CARTESIAN_POINT('Ctrl Pts',(-0.209182595670359,0.0122484553035031,
0.00900382443876613));
#39554=CARTESIAN_POINT('',(-0.210183354865266,0.0122485335158607,0.00902553609473393));
#39555=CARTESIAN_POINT('Ctrl Pts',(-0.209182651576042,0.0122484518533258,
0.00900382775451287));
#39556=CARTESIAN_POINT('Ctrl Pts',(-0.209514352353559,0.0122484795677455,
0.00901102297423394));
#39557=CARTESIAN_POINT('Ctrl Pts',(-0.209848095210384,0.0122485111023429,
0.00901826026877957));
#39558=CARTESIAN_POINT('Ctrl Pts',(-0.210183395177975,0.0122485465320611,
0.00902552904778905));
#39559=CARTESIAN_POINT('',(-0.21009684684534,0.00750005508728801,0.0103553421922863));
#39560=CARTESIAN_POINT('Ctrl Pts',(-0.210183354865266,0.0122485335158607,
0.00902553609473393));
#39561=CARTESIAN_POINT('Ctrl Pts',(-0.21014698672904,0.0120127163893144,
0.00916829590243412));
#39562=CARTESIAN_POINT('Ctrl Pts',(-0.210116347665497,0.0117983968347776,
0.00928354689096572));
#39563=CARTESIAN_POINT('Ctrl Pts',(-0.210091629427547,0.0116133305266073,
0.00937637517010963));
#39564=CARTESIAN_POINT('Ctrl Pts',(-0.210079270308572,0.0115207973725221,
0.00942278930968159));
#39565=CARTESIAN_POINT('Ctrl Pts',(-0.210068390961519,0.0114355897376177,
0.0094636177544873));
#39566=CARTESIAN_POINT('Ctrl Pts',(-0.210058641871792,0.0113547868889098,
0.00950103016538221));
#39567=CARTESIAN_POINT('Ctrl Pts',(-0.210053767326929,0.0113143854645558,
0.00951973637082966));
#39568=CARTESIAN_POINT('Ctrl Pts',(-0.210049175979292,0.0112750711533674,
0.00953755945900945));
#39569=CARTESIAN_POINT('Ctrl Pts',(-0.210045325081173,0.0112414204036042,
0.00955258917223236));
#39570=CARTESIAN_POINT('Ctrl Pts',(-0.210041474183053,0.0112077696538411,
0.00956761888545526));
#39571=CARTESIAN_POINT('Ctrl Pts',(-0.210038361718855,0.0111798246297253,
0.00957994792756669));
#39572=CARTESIAN_POINT('Ctrl Pts',(-0.210034112592833,0.0111389858803094,
0.0095975987918489));
#39573=CARTESIAN_POINT('Ctrl Pts',(-0.21002986346681,0.0110981471308936,
0.00961524965613112));
#39574=CARTESIAN_POINT('Ctrl Pts',(-0.210024481319256,0.0110443415114109,
0.00963805491322707));
#39575=CARTESIAN_POINT('Ctrl Pts',(-0.210019750328922,0.0109937885568437,
0.00965888559117742));
#39576=CARTESIAN_POINT('Ctrl Pts',(-0.210015019338587,0.0109432356022766,
0.00967971626912777));
#39577=CARTESIAN_POINT('Ctrl Pts',(-0.210010936953547,0.010895983133197,
0.00969868974003685));
#39578=CARTESIAN_POINT('Ctrl Pts',(-0.210007065948202,0.0108480896648573,
0.00971747917026967));
#39579=CARTESIAN_POINT('Ctrl Pts',(-0.209999323937511,0.010752302728178,
0.00975505803073532));
#39580=CARTESIAN_POINT('Ctrl Pts',(-0.20999243008157,0.0106539077570024,
0.00979177949000212));
#39581=CARTESIAN_POINT('Ctrl Pts',(-0.209986729913038,0.0105554038508432,
0.00982662910691118));
#39582=CARTESIAN_POINT('Ctrl Pts',(-0.209975329575974,0.0103583960385248,
0.00989632834072931));
#39583=CARTESIAN_POINT('Ctrl Pts',(-0.20996870266948,0.0101609552771156,
0.00995860087647994));
#39584=CARTESIAN_POINT('Ctrl Pts',(-0.209966181083884,0.0099663565756417,
0.0100131324078234));
#39585=CARTESIAN_POINT('Ctrl Pts',(-0.209963659498287,0.0097717578741678,
0.010067663939167));
#39586=CARTESIAN_POINT('Ctrl Pts',(-0.20996523499344,0.0095801214325255,
0.0101148334644337));
#39587=CARTESIAN_POINT('Ctrl Pts',(-0.209970581938221,0.00937693500919795,
0.0101576234975028));
#39588=CARTESIAN_POINT('Ctrl Pts',(-0.209973255410611,0.00927534179753417,
0.0101790185140374));
#39589=CARTESIAN_POINT('Ctrl Pts',(-0.209976874657855,0.00917083217192017,
0.0101991847003489));
#39590=CARTESIAN_POINT('Ctrl Pts',(-0.209981275808507,0.00906791018342924,
0.0102172183293223));
#39591=CARTESIAN_POINT('Ctrl Pts',(-0.209983476383833,0.00901644918918377,
0.010226235143809));
#39592=CARTESIAN_POINT('Ctrl Pts',(-0.209985871541067,0.00896539272474216,
0.0102347599358926));
#39593=CARTESIAN_POINT('Ctrl Pts',(-0.209988753927672,0.00890990792081734,
0.0102434932168294));
#39594=CARTESIAN_POINT('Ctrl Pts',(-0.209991636314278,0.00885442311689252,
0.0102522264977662));
#39595=CARTESIAN_POINT('Ctrl Pts',(-0.209995009051587,0.00879448684103273,
0.0102610247017059));
#39596=CARTESIAN_POINT('Ctrl Pts',(-0.209997655872122,0.00874962140646036,
0.0102672801053472));
#39597=CARTESIAN_POINT('Ctrl Pts',(-0.210000302692657,0.00870475597188798,
0.0102735355089885));
#39598=CARTESIAN_POINT('Ctrl Pts',(-0.210002219201085,0.00867498878986495,
0.0102774502766726));
#39599=CARTESIAN_POINT('Ctrl Pts',(-0.210004644701109,0.00863857556372592,
0.0102820788410741));
#39600=CARTESIAN_POINT('Ctrl Pts',(-0.210007070201132,0.0086021623375869,
0.0102867074054757));
#39601=CARTESIAN_POINT('Ctrl Pts',(-0.210010007073723,0.00855908986493375,
0.0102919402530651));
#39602=CARTESIAN_POINT('Ctrl Pts',(-0.210013153594257,0.00851467298255937,
0.010296974800606));
#39603=CARTESIAN_POINT('Ctrl Pts',(-0.210019446635327,0.00842583921781061,
0.0103070438956879));
#39604=CARTESIAN_POINT('Ctrl Pts',(-0.210026575247729,0.00833164123919009,
0.0103164587172962));
#39605=CARTESIAN_POINT('Ctrl Pts',(-0.210034778165727,0.00822815474954129,
0.0103249153303143));
#39606=CARTESIAN_POINT('Ctrl Pts',(-0.210051184001722,0.00802118177024369,
0.0103418285563504));
#39607=CARTESIAN_POINT('Ctrl Pts',(-0.210071889472725,0.00777705421800207,
0.0103547979768471));
#39608=CARTESIAN_POINT('Ctrl Pts',(-0.210096846845341,0.00750005508730573,
0.0103553421922863));
#39609=CARTESIAN_POINT('',(-0.210182935446423,0.00274902832065848,0.0090240398964221));
#39610=CARTESIAN_POINT('Ctrl Pts',(-0.21009684684534,0.00750005508728801,
0.0103553421922863));
#39611=CARTESIAN_POINT('Ctrl Pts',(-0.210072031529707,0.00722345799301737,
0.0103548042976559));
#39612=CARTESIAN_POINT('Ctrl Pts',(-0.210051420859798,0.00697958369651794,
0.0103418734782538));
#39613=CARTESIAN_POINT('Ctrl Pts',(-0.210035067604621,0.00677277347393194,
0.0103249955737702));
#39614=CARTESIAN_POINT('Ctrl Pts',(-0.210026890977033,0.00666936836263893,
0.0103165566215284));
#39615=CARTESIAN_POINT('Ctrl Pts',(-0.210019778074828,0.00657522908219787,
0.0103071597973542));
#39616=CARTESIAN_POINT('Ctrl Pts',(-0.210013486125652,0.00648637336607246,
0.0102970986183953));
#39617=CARTESIAN_POINT('Ctrl Pts',(-0.210010340151064,0.00644194550800976,
0.0102920680289159));
#39618=CARTESIAN_POINT('Ctrl Pts',(-0.210007400180234,0.00639884193886295,
0.0102868361402636));
#39619=CARTESIAN_POINT('Ctrl Pts',(-0.210004973587317,0.00636245780845583,
0.0102822154131323));
#39620=CARTESIAN_POINT('Ctrl Pts',(-0.2100025469944,0.00632607367804871,
0.010277594686001));
#39621=CARTESIAN_POINT('Ctrl Pts',(-0.210000631361163,0.00629639559480933,
0.0102736963514528));
#39622=CARTESIAN_POINT('Ctrl Pts',(-0.209997964377369,0.00625135134602337,
0.0102674207308797));
#39623=CARTESIAN_POINT('Ctrl Pts',(-0.209995297393576,0.00620630709723741,
0.0102611451103067));
#39624=CARTESIAN_POINT('Ctrl Pts',(-0.209991883546243,0.00614592463301405,
0.0102522858149151));
#39625=CARTESIAN_POINT('Ctrl Pts',(-0.209988966602404,0.00609008632608619,
0.0102434964886858));
#39626=CARTESIAN_POINT('Ctrl Pts',(-0.209986049658564,0.00603424801915834,
0.0102347071624564));
#39627=CARTESIAN_POINT('Ctrl Pts',(-0.209983626420324,0.00598293016518101,
0.0102261348990641));
#39628=CARTESIAN_POINT('Ctrl Pts',(-0.209981397477455,0.00593121358005969,
0.010217067716942));
#39629=CARTESIAN_POINT('Ctrl Pts',(-0.209976939591716,0.00582778040981704,
0.0101989333526979));
#39630=CARTESIAN_POINT('Ctrl Pts',(-0.209973262537477,0.00572278351867268,
0.0101786514229577));
#39631=CARTESIAN_POINT('Ctrl Pts',(-0.209970535541532,0.00562077092014045,
0.0101571397893884));
#39632=CARTESIAN_POINT('Ctrl Pts',(-0.209965081549642,0.00541674572307599,
0.0101141165222497));
#39633=CARTESIAN_POINT('Ctrl Pts',(-0.209963416125406,0.00522454125933521,
0.0100667110234108));
#39634=CARTESIAN_POINT('Ctrl Pts',(-0.209965850832377,0.00502978892616377,
0.0100120423326667));
#39635=CARTESIAN_POINT('Ctrl Pts',(-0.209968285539348,0.00483503659299233,
0.00995737364192262));
#39636=CARTESIAN_POINT('Ctrl Pts',(-0.209974828395779,0.00463785411534847,
0.00989507293553626));
#39637=CARTESIAN_POINT('Ctrl Pts',(-0.209986151081867,0.00444115623501538,
0.00982539340942192));
#39638=CARTESIAN_POINT('Ctrl Pts',(-0.209991812424911,0.00434280729484884,
0.00979055364636475));
#39639=CARTESIAN_POINT('Ctrl Pts',(-0.209998669097466,0.00424458096669036,
0.00975385206320209));
#39640=CARTESIAN_POINT('Ctrl Pts',(-0.210006377134424,0.00414898659058324,
0.0097163102825907));
#39641=CARTESIAN_POINT('Ctrl Pts',(-0.210010231152903,0.00410118940252968,
0.009697539392285));
#39642=CARTESIAN_POINT('Ctrl Pts',(-0.210014297357555,0.00405403923554369,
0.00967858857821047));
#39643=CARTESIAN_POINT('Ctrl Pts',(-0.210019009898115,0.00400361901395296,
0.00965779428064045));
#39644=CARTESIAN_POINT('Ctrl Pts',(-0.210023722438676,0.00395319879236224,
0.00963699998307044));
#39645=CARTESIAN_POINT('Ctrl Pts',(-0.210029083843341,0.00389955594149032,
0.00961424590868889));
#39646=CARTESIAN_POINT('Ctrl Pts',(-0.210033322718555,0.00385880004226566,
0.00959661798140514));
#39647=CARTESIAN_POINT('Ctrl Pts',(-0.210037561593769,0.003818044143041,
0.00957899005412139));
#39648=CARTESIAN_POINT('Ctrl Pts',(-0.210040674328065,0.00379010257233756,
0.00956665439685066));
#39649=CARTESIAN_POINT('Ctrl Pts',(-0.21004452606445,0.00375646787301374,
0.00955162163910428));
#39650=CARTESIAN_POINT('Ctrl Pts',(-0.210048377800834,0.00372283317368993,
0.00953658888135791));
#39651=CARTESIAN_POINT('Ctrl Pts',(-0.210052970542858,0.00368354728906639,
0.00951876686204021));
#39652=CARTESIAN_POINT('Ctrl Pts',(-0.210057849482595,0.00364316443446752,
0.00950005720653822));
#39653=CARTESIAN_POINT('Ctrl Pts',(-0.210067607362068,0.00356239872526979,
0.00946263789553426));
#39654=CARTESIAN_POINT('Ctrl Pts',(-0.210078507512784,0.00347718902812302,
0.009421783939139));
#39655=CARTESIAN_POINT('Ctrl Pts',(-0.210090897724529,0.0033846321571345,
0.00937532941205294));
#39656=CARTESIAN_POINT('Ctrl Pts',(-0.210115678148019,0.00319951841515747,
0.00928242035788084));
#39657=CARTESIAN_POINT('Ctrl Pts',(-0.210146420514204,0.00298506387705781,
0.00916703088647436));
#39658=CARTESIAN_POINT('Ctrl Pts',(-0.210182935446423,0.00274902832065848,
0.0090240398964221));
#39659=CARTESIAN_POINT('Ctrl Pts',(-0.210182976903937,0.00274902032469847,
0.00902403592680517));
#39660=CARTESIAN_POINT('Ctrl Pts',(-0.20984954026572,0.00274892753071286,
0.00901673074474417));
#39661=CARTESIAN_POINT('Ctrl Pts',(-0.209515992344277,0.00274883116012269,
0.00900942096250049));
#39662=CARTESIAN_POINT('Ctrl Pts',(-0.209182541425264,0.00274873127424957,
0.00900211114486483));
#39663=CARTESIAN_POINT('Origin',(-0.193569723895743,0.00749999928673165,
0.000576601746083541));
#39664=CARTESIAN_POINT('',(-0.193103855785931,0.00749669634329043,0.00997223704509611));
#39665=CARTESIAN_POINT('',(-0.193177238560899,0.00273223379907955,0.00867522024057621));
#39666=CARTESIAN_POINT('Ctrl Pts',(-0.193177238560899,0.00273223379907955,
0.00867522024057621));
#39667=CARTESIAN_POINT('Ctrl Pts',(-0.193141338548451,0.00296984836335153,
0.00881424998266486));
#39668=CARTESIAN_POINT('Ctrl Pts',(-0.193096834920356,0.00328633988174973,
0.00897964130725951));
#39669=CARTESIAN_POINT('Ctrl Pts',(-0.193053183912405,0.00364435066138988,
0.00914510567071404));
#39670=CARTESIAN_POINT('Ctrl Pts',(-0.193033364102516,0.00382132177014467,
0.00922249602324718));
#39671=CARTESIAN_POINT('Ctrl Pts',(-0.193005741650242,0.00413502514833468,
0.00934940056504819));
#39672=CARTESIAN_POINT('Ctrl Pts',(-0.192982517471961,0.00451365419336154,
0.00948680984862821));
#39673=CARTESIAN_POINT('Ctrl Pts',(-0.192968455245345,0.00503817115554176,
0.00964815811736775));
#39674=CARTESIAN_POINT('Ctrl Pts',(-0.192975186509652,0.00549854166420586,
0.00975802728443494));
#39675=CARTESIAN_POINT('Ctrl Pts',(-0.19298920675885,0.00587143281971192,
0.00982864698119864));
#39676=CARTESIAN_POINT('Ctrl Pts',(-0.192999409086713,0.0060799974385049,
0.00986272641220591));
#39677=CARTESIAN_POINT('Ctrl Pts',(-0.193010093679397,0.00626674437952322,
0.00988934301760898));
#39678=CARTESIAN_POINT('Ctrl Pts',(-0.193015756303844,0.00635510160385565,
0.00990051431842612));
#39679=CARTESIAN_POINT('Ctrl Pts',(-0.193027331983661,0.00652836366928688,
0.00992104290850712));
#39680=CARTESIAN_POINT('Ctrl Pts',(-0.193051322868053,0.00685751684410879,
0.00995279515838206));
#39681=CARTESIAN_POINT('Ctrl Pts',(-0.193080570759728,0.00722182594281122,
0.00997163711061381));
#39682=CARTESIAN_POINT('Ctrl Pts',(-0.193103856303716,0.00749669585242133,
0.0099722370582992));
#39683=CARTESIAN_POINT('',(-0.193178778898313,0.0122641846768735,0.00867735780753799));
#39684=CARTESIAN_POINT('Ctrl Pts',(-0.193103856259104,0.00749669638308835,
0.00997223705752114));
#39685=CARTESIAN_POINT('Ctrl Pts',(-0.193080779856104,0.00777118576984942,
0.00997183458338455));
#39686=CARTESIAN_POINT('Ctrl Pts',(-0.193051800859628,0.00813509755822241,
0.0099533036309153));
#39687=CARTESIAN_POINT('Ctrl Pts',(-0.193028037317639,0.00846412037883092,
0.00992183479932284));
#39688=CARTESIAN_POINT('Ctrl Pts',(-0.193016578366468,0.00863735206193072,
0.00990145478660238));
#39689=CARTESIAN_POINT('Ctrl Pts',(-0.193010965599083,0.00872584131090312,
0.0098903385279732));
#39690=CARTESIAN_POINT('Ctrl Pts',(-0.193000420585326,0.00891232900027939,
0.00986391558070171));
#39691=CARTESIAN_POINT('Ctrl Pts',(-0.192990369106261,0.00912085072542072,
0.00983002353592887));
#39692=CARTESIAN_POINT('Ctrl Pts',(-0.192976617902903,0.00949374270917578,
0.00975975040781575));
#39693=CARTESIAN_POINT('Ctrl Pts',(-0.19297025631144,0.00995631925037694,
0.00964969128851549));
#39694=CARTESIAN_POINT('Ctrl Pts',(-0.192984612054924,0.010479251557637,
0.00948921247306322));
#39695=CARTESIAN_POINT('Ctrl Pts',(-0.193007926010543,0.0108584095631401,
0.00935197207317474));
#39696=CARTESIAN_POINT('Ctrl Pts',(-0.193035575544608,0.0111730562205009,
0.00922493533851728));
#39697=CARTESIAN_POINT('Ctrl Pts',(-0.193055315395668,0.0113502096335574,
0.00914759534273209));
#39698=CARTESIAN_POINT('Ctrl Pts',(-0.193098792555964,0.0117089358444973,
0.00898206393295022));
#39699=CARTESIAN_POINT('Ctrl Pts',(-0.193143069638179,0.0120260667690436,
0.00881654618530351));
#39700=CARTESIAN_POINT('Ctrl Pts',(-0.193178778898313,0.0122641846768735,
0.00867735780753799));
#39701=CARTESIAN_POINT('',(-0.194178078842629,0.0122641623067804,0.00869897679015584));
#39702=CARTESIAN_POINT('Ctrl Pts',(-0.193178864680093,0.0122641819069075,
0.00867736129034749));
#39703=CARTESIAN_POINT('Ctrl Pts',(-0.193463836609973,0.0122641761777926,
0.00868352602731349));
#39704=CARTESIAN_POINT('Ctrl Pts',(-0.193745328838661,0.0122641740469773,
0.0086896134147566));
#39705=CARTESIAN_POINT('Ctrl Pts',(-0.194074393693453,0.0122641754661562,
0.00869672728191949));
#39706=CARTESIAN_POINT('Ctrl Pts',(-0.194126196785175,0.0122641758053938,
0.00869784711561093));
#39707=CARTESIAN_POINT('Ctrl Pts',(-0.194178146257402,0.0122641762630964,
0.00869897004455999));
#39708=CARTESIAN_POINT('',(-0.194103293745545,0.00749642396384868,0.00999384323056315));
#39709=CARTESIAN_POINT('Ctrl Pts',(-0.194178078842629,0.0122641623067804,
0.00869897679015584));
#39710=CARTESIAN_POINT('Ctrl Pts',(-0.194141973426115,0.0120248709868358,
0.00883884524871636));
#39711=CARTESIAN_POINT('Ctrl Pts',(-0.194097233107932,0.0117060242318462,
0.00900513658754215));
#39712=CARTESIAN_POINT('Ctrl Pts',(-0.194053464891725,0.011345942522752,
0.00917111002034425));
#39713=CARTESIAN_POINT('Ctrl Pts',(-0.194033531058898,0.0111668482859879,
0.0092491326416897));
#39714=CARTESIAN_POINT('Ctrl Pts',(-0.19400626338759,0.0108549923204777,
0.00937482374371128));
#39715=CARTESIAN_POINT('Ctrl Pts',(-0.193983223778424,0.0104774717474761,
0.0095113892130402));
#39716=CARTESIAN_POINT('Ctrl Pts',(-0.193969272664656,0.00995468087707124,
0.00967167132788243));
#39717=CARTESIAN_POINT('Ctrl Pts',(-0.193975843094312,0.00949639281041089,
0.00978072143137081));
#39718=CARTESIAN_POINT('Ctrl Pts',(-0.193989589072645,0.00912520255875588,
0.00985085735588398));
#39719=CARTESIAN_POINT('Ctrl Pts',(-0.193999610986714,0.00891747787109268,
0.00988472745515668));
#39720=CARTESIAN_POINT('Ctrl Pts',(-0.194010085577249,0.00873187890670615,
0.00991114102178041));
#39721=CARTESIAN_POINT('Ctrl Pts',(-0.194015720554619,0.00864278840341037,
0.0099223937624794));
#39722=CARTESIAN_POINT('Ctrl Pts',(-0.1940271920793,0.00846906395058688,
0.0099429287560856));
#39723=CARTESIAN_POINT('Ctrl Pts',(-0.194051023711656,0.00813851336097762,
0.00997471124740048));
#39724=CARTESIAN_POINT('Ctrl Pts',(-0.194080113956685,0.00777260055205324,
0.00999344724325746));
#39725=CARTESIAN_POINT('Ctrl Pts',(-0.194103293745545,0.00749642396384868,
0.00999384323056315));
#39726=CARTESIAN_POINT('',(-0.194177625723629,0.0027323178355601,0.00869689395108569));
#39727=CARTESIAN_POINT('Ctrl Pts',(-0.194103293744492,0.00749642367320619,
0.00999384323042973));
#39728=CARTESIAN_POINT('Ctrl Pts',(-0.194079985850101,0.00722088152225355,
0.00999323445983037));
#39729=CARTESIAN_POINT('Ctrl Pts',(-0.194050722774099,0.0068557531252023,
0.00997429687100921));
#39730=CARTESIAN_POINT('Ctrl Pts',(-0.194026735405087,0.00652587479550234,
0.00994239080627125));
#39731=CARTESIAN_POINT('Ctrl Pts',(-0.194015177153977,0.00635238376057256,
0.00992178766320044));
#39732=CARTESIAN_POINT('Ctrl Pts',(-0.194009508832243,0.00626361512406841,
0.00991053211974325));
#39733=CARTESIAN_POINT('Ctrl Pts',(-0.193998907820037,0.00607757541380027,
0.00988395901128883));
#39734=CARTESIAN_POINT('Ctrl Pts',(-0.193988775979243,0.00586949907587681,
0.00984990969528716));
#39735=CARTESIAN_POINT('Ctrl Pts',(-0.193974870892261,0.00549767136340122,
0.00977943757151345));
#39736=CARTESIAN_POINT('Ctrl Pts',(-0.193968261065726,0.0050373352232251,
0.0096694859417466));
#39737=CARTESIAN_POINT('Ctrl Pts',(-0.193982282452568,0.00451653356420576,
0.00950934180685302));
#39738=CARTESIAN_POINT('Ctrl Pts',(-0.194005392087704,0.00413945225215935,
0.009372680210967));
#39739=CARTESIAN_POINT('Ctrl Pts',(-0.194032753971147,0.00382781295525132,
0.00924684759490062));
#39740=CARTESIAN_POINT('Ctrl Pts',(-0.194052709819781,0.00364922188115017,
0.00916891841726741));
#39741=CARTESIAN_POINT('Ctrl Pts',(-0.194096578993025,0.00328971244232934,
0.0090029756844143));
#39742=CARTESIAN_POINT('Ctrl Pts',(-0.194141428072699,0.00297131658783776,
0.00883672851200297));
#39743=CARTESIAN_POINT('Ctrl Pts',(-0.194177625723629,0.0027323178355601,
0.00869689395108569));
#39744=CARTESIAN_POINT('Ctrl Pts',(-0.194177692817492,0.00273230882489036,
0.00869689009986668));
#39745=CARTESIAN_POINT('Ctrl Pts',(-0.193847122383193,0.00273228814490392,
0.00868973235595818));
#39746=CARTESIAN_POINT('Ctrl Pts',(-0.193513460240482,0.00273226267284877,
0.00868250496244904));
#39747=CARTESIAN_POINT('Ctrl Pts',(-0.193177329099023,0.00273223222473439,
0.00867522127133823));
#39748=CARTESIAN_POINT('Origin',(-0.213570493936196,0.00749999991453831,
0.00135810061113277));
#39749=CARTESIAN_POINT('',(-0.213095879900848,0.00749981038892108,0.0104239596070259));
#39750=CARTESIAN_POINT('',(-0.213184217082503,0.00275309087589512,0.00908489825530902));
#39751=CARTESIAN_POINT('Ctrl Pts',(-0.213184217082503,0.00275309087589512,
0.00908489825530902));
#39752=CARTESIAN_POINT('Ctrl Pts',(-0.213147946013642,0.00298738821182737,
0.00922795940497672));
#39753=CARTESIAN_POINT('Ctrl Pts',(-0.213102043822126,0.00330706237473753,
0.00940128400476012));
#39754=CARTESIAN_POINT('Ctrl Pts',(-0.213063912983746,0.00360352093124194,
0.00954476365425644));
#39755=CARTESIAN_POINT('Ctrl Pts',(-0.213045438975613,0.00376028588544419,
0.00961638748972627));
#39756=CARTESIAN_POINT('Ctrl Pts',(-0.21303611057467,0.00384298953821337,
0.00965330164747907));
#39757=CARTESIAN_POINT('Ctrl Pts',(-0.213019519962499,0.00400641619864203,
0.0097232562400473));
#39758=CARTESIAN_POINT('Ctrl Pts',(-0.213002812612574,0.00419655873439527,
0.00980013519929093));
#39759=CARTESIAN_POINT('Ctrl Pts',(-0.212978040034831,0.00454275981693908,
0.00993049491628299));
#39760=CARTESIAN_POINT('Ctrl Pts',(-0.212960945692762,0.00503202112932064,
0.0100856322688812));
#39761=CARTESIAN_POINT('Ctrl Pts',(-0.212964569057503,0.00551635865886951,
0.0102060183120711));
#39762=CARTESIAN_POINT('Ctrl Pts',(-0.212977236919282,0.00588477353496685,
0.0102774366800835));
#39763=CARTESIAN_POINT('Ctrl Pts',(-0.212986849121923,0.00609047891122502,
0.0103120226917365));
#39764=CARTESIAN_POINT('Ctrl Pts',(-0.212997070713013,0.00627230341138433,
0.0103387200016791));
#39765=CARTESIAN_POINT('Ctrl Pts',(-0.213002759777912,0.00636041695190613,
0.0103502342952264));
#39766=CARTESIAN_POINT('Ctrl Pts',(-0.213014513644883,0.0065320872202858,
0.0103712237365575));
#39767=CARTESIAN_POINT('Ctrl Pts',(-0.213039521035394,0.00685995861526675,
0.0104039161017014));
#39768=CARTESIAN_POINT('Ctrl Pts',(-0.213070754183437,0.00722428790289929,
0.0104234068834067));
#39769=CARTESIAN_POINT('Ctrl Pts',(-0.213095879900848,0.00749981038892108,
0.0104239596070259));
#39770=CARTESIAN_POINT('',(-0.213185690986499,0.0122460699114039,0.00908544519816533));
#39771=CARTESIAN_POINT('Ctrl Pts',(-0.213095879800977,0.00749981164463391,
0.0104239596048778));
#39772=CARTESIAN_POINT('Ctrl Pts',(-0.21307066098287,0.00777532698194311,
0.0104234163142761));
#39773=CARTESIAN_POINT('Ctrl Pts',(-0.213039345087209,0.00813961477500167,
0.0104039423501419));
#39774=CARTESIAN_POINT('Ctrl Pts',(-0.213014332410071,0.00846746144496389,
0.0103712668864278));
#39775=CARTESIAN_POINT('Ctrl Pts',(-0.213002611006837,0.00863903521304472,
0.0103503010215217));
#39776=CARTESIAN_POINT('Ctrl Pts',(-0.212996938122665,0.00872728047684472,
0.0103387717522634));
#39777=CARTESIAN_POINT('Ctrl Pts',(-0.212986830556453,0.00890843702918285,
0.0103121890710692));
#39778=CARTESIAN_POINT('Ctrl Pts',(-0.212977345913122,0.00911377178123675,
0.0102776975483701));
#39779=CARTESIAN_POINT('Ctrl Pts',(-0.212964930987284,0.00948166907831092,
0.0102064767184181));
#39780=CARTESIAN_POINT('Ctrl Pts',(-0.212961762283236,0.00996812097797597,
0.0100856145356055));
#39781=CARTESIAN_POINT('Ctrl Pts',(-0.212979243563552,0.010455543907438,
0.00993109274363753));
#39782=CARTESIAN_POINT('Ctrl Pts',(-0.213004227851109,0.0108020944666052,
0.00980069536728062));
#39783=CARTESIAN_POINT('Ctrl Pts',(-0.213021034374403,0.010992458373273,
0.00972376062269633));
#39784=CARTESIAN_POINT('Ctrl Pts',(-0.213037712034966,0.0111563039303219,
0.00965364877306718));
#39785=CARTESIAN_POINT('Ctrl Pts',(-0.213047042089263,0.0112389114824525,
0.00961678452581526));
#39786=CARTESIAN_POINT('Ctrl Pts',(-0.213065532800899,0.011395719129502,
0.00954516055025792));
#39787=CARTESIAN_POINT('Ctrl Pts',(-0.213103648549054,0.011692151249117,
0.00940172652220947));
#39788=CARTESIAN_POINT('Ctrl Pts',(-0.213149487437096,0.0120118029750531,
0.00922845413600301));
#39789=CARTESIAN_POINT('Ctrl Pts',(-0.213185690986499,0.0122460699114039,
0.00908544519816533));
#39790=CARTESIAN_POINT('',(-0.21418640254952,0.0122466617247526,0.00910686742116922));
#39791=CARTESIAN_POINT('Ctrl Pts',(-0.2131857349772,0.0122460667524225,
0.00908544809488056));
#39792=CARTESIAN_POINT('Ctrl Pts',(-0.213519274711084,0.0122462654086515,
0.00909258732591442));
#39793=CARTESIAN_POINT('Ctrl Pts',(-0.213852910436955,0.0122464675875923,
0.00909972647388659));
#39794=CARTESIAN_POINT('Ctrl Pts',(-0.214186433624517,0.0122466731629066,
0.00910686107552119));
#39795=CARTESIAN_POINT('',(-0.214095609529152,0.00749962227619371,0.0104457232276635));
#39796=CARTESIAN_POINT('Ctrl Pts',(-0.21418640254952,0.0122466617247526,
0.00910686742116922));
#39797=CARTESIAN_POINT('Ctrl Pts',(-0.214150242333865,0.0120125218227116,
0.00924982396327141));
#39798=CARTESIAN_POINT('Ctrl Pts',(-0.214119695946351,0.0117994816513621,
0.00936540572011131));
#39799=CARTESIAN_POINT('Ctrl Pts',(-0.214094978666479,0.0116154403154175,
0.00945854637191276));
#39800=CARTESIAN_POINT('Ctrl Pts',(-0.214082620026543,0.0115234196474453,
0.00950511669781349));
#39801=CARTESIAN_POINT('Ctrl Pts',(-0.214071718166771,0.0114386625650815,
0.00954609956536755));
#39802=CARTESIAN_POINT('Ctrl Pts',(-0.214061901531328,0.0113580994422348,
0.00958373978635917));
#39803=CARTESIAN_POINT('Ctrl Pts',(-0.214056993213607,0.0113178178808115,
0.00960255989685498));
#39804=CARTESIAN_POINT('Ctrl Pts',(-0.214052356864697,0.0112785699444597,
0.00962051390331013));
#39805=CARTESIAN_POINT('Ctrl Pts',(-0.214048480156471,0.011245138655905,
0.00963558167760563));
#39806=CARTESIAN_POINT('Ctrl Pts',(-0.214044603448246,0.0112117073673503,
0.00965064945190114));
#39807=CARTESIAN_POINT('Ctrl Pts',(-0.214041484259469,0.0111841374694742,
0.00966292843300825));
#39808=CARTESIAN_POINT('Ctrl Pts',(-0.214037123296481,0.0111429803313046,
0.00968087903102329));
#39809=CARTESIAN_POINT('Ctrl Pts',(-0.214032762333493,0.0111018231931349,
0.00969882962903835));
#39810=CARTESIAN_POINT('Ctrl Pts',(-0.2140271634979,0.0110469997465657,
0.00972227262366574));
#39811=CARTESIAN_POINT('Ctrl Pts',(-0.214022249173218,0.0109957218446917,
0.00974357751472393));
#39812=CARTESIAN_POINT('Ctrl Pts',(-0.214017334848535,0.0109444439428178,
0.00976488240578211));
#39813=CARTESIAN_POINT('Ctrl Pts',(-0.21401310225623,0.0108967640800364,
0.00978417682540769));
#39814=CARTESIAN_POINT('Ctrl Pts',(-0.214009080069515,0.0108484579449649,
0.00980327310576939));
#39815=CARTESIAN_POINT('Ctrl Pts',(-0.214001035696085,0.0107518456748219,
0.00984146566649278));
#39816=CARTESIAN_POINT('Ctrl Pts',(-0.213993835957383,0.0106526766076716,
0.00987872729674494));
#39817=CARTESIAN_POINT('Ctrl Pts',(-0.213987853556733,0.0105541854242721,
0.00991381013011468));
#39818=CARTESIAN_POINT('Ctrl Pts',(-0.213975888755433,0.0103572030574731,
0.00998397579685417));
#39819=CARTESIAN_POINT('Ctrl Pts',(-0.213968788113749,0.0101630030187667,
0.0100456647992242));
#39820=CARTESIAN_POINT('Ctrl Pts',(-0.213965822435937,0.00996845937459876,
0.0101006100729016));
#39821=CARTESIAN_POINT('Ctrl Pts',(-0.213962856758125,0.00977391573043078,
0.010155555346579));
#39822=CARTESIAN_POINT('Ctrl Pts',(-0.213964023065156,0.00957908264351894,
0.0102038937335934));
#39823=CARTESIAN_POINT('Ctrl Pts',(-0.21396908446874,0.00937400127475314,
0.0102473014551026));
#39824=CARTESIAN_POINT('Ctrl Pts',(-0.213971615170531,0.00927146059037024,
0.0102690053158571));
#39825=CARTESIAN_POINT('Ctrl Pts',(-0.213975121956478,0.00916633323749196,
0.0102893703986903));
#39826=CARTESIAN_POINT('Ctrl Pts',(-0.213979431254745,0.0090628082995213,
0.010307568910536));
#39827=CARTESIAN_POINT('Ctrl Pts',(-0.213981585903878,0.00901104583053597,
0.0103166681664589));
#39828=CARTESIAN_POINT('Ctrl Pts',(-0.213983940282687,0.00895969182533451,
0.0103252670482856));
#39829=CARTESIAN_POINT('Ctrl Pts',(-0.213986791258972,0.00890381663198042,
0.0103340808021143));
#39830=CARTESIAN_POINT('Ctrl Pts',(-0.213989642235257,0.00884794143862632,
0.010342894555943));
#39831=CARTESIAN_POINT('Ctrl Pts',(-0.213992993054109,0.00878752094369971,
0.0103517741168447));
#39832=CARTESIAN_POINT('Ctrl Pts',(-0.213995611973794,0.00874260648517612,
0.0103580417152856));
#39833=CARTESIAN_POINT('Ctrl Pts',(-0.213998230893478,0.00869769202665253,
0.0103643093137265));
#39834=CARTESIAN_POINT('Ctrl Pts',(-0.214000113365021,0.00866831195366434,
0.0103681739093432));
#39835=CARTESIAN_POINT('Ctrl Pts',(-0.214002517474644,0.00863218386042468,
0.0103727705888645));
#39836=CARTESIAN_POINT('Ctrl Pts',(-0.214004921584266,0.00859605576718503,
0.0103773672683857));
#39837=CARTESIAN_POINT('Ctrl Pts',(-0.214007849777381,0.00855316610357289,
0.0103825837003049));
#39838=CARTESIAN_POINT('Ctrl Pts',(-0.214010995703821,0.00850896144170923,
0.0103875992331155));
#39839=CARTESIAN_POINT('Ctrl Pts',(-0.214017287556701,0.00842055211798191,
0.0103976302987366));
#39840=CARTESIAN_POINT('Ctrl Pts',(-0.214024447245813,0.00832689656229679,
0.010407000033626));
#39841=CARTESIAN_POINT('Ctrl Pts',(-0.214032716845087,0.00822397462738881,
0.0104154199196861));
#39842=CARTESIAN_POINT('Ctrl Pts',(-0.214049256043635,0.00801813075757284,
0.0104322596918063));
#39843=CARTESIAN_POINT('Ctrl Pts',(-0.214070237444844,0.00777522053581388,
0.0104451823806317));
#39844=CARTESIAN_POINT('Ctrl Pts',(-0.214095609529044,0.00749962227620365,
0.0104457232276612));
#39845=CARTESIAN_POINT('',(-0.214184674208418,0.00275297203288764,0.00910660423566295));
#39846=CARTESIAN_POINT('Ctrl Pts',(-0.214095609529152,0.00749962227619371,
0.0104457232276635));
#39847=CARTESIAN_POINT('Ctrl Pts',(-0.214070225361772,0.00722287809655221,
0.0104451590880677));
#39848=CARTESIAN_POINT('Ctrl Pts',(-0.214049220380385,0.00697896534568404,
0.0104321129966427));
#39849=CARTESIAN_POINT('Ctrl Pts',(-0.21403264326934,0.00677222587095417,
0.0104151132536551));
#39850=CARTESIAN_POINT('Ctrl Pts',(-0.214024354713817,0.00666885613358923,
0.0104066133821613));
#39851=CARTESIAN_POINT('Ctrl Pts',(-0.214017172498679,0.00657477953844181,
0.0103971539088115));
#39852=CARTESIAN_POINT('Ctrl Pts',(-0.214010855799684,0.0064860163185143,
0.0103870326191949));
#39853=CARTESIAN_POINT('Ctrl Pts',(-0.214007697450186,0.00644163470855054,
0.0103819719743867));
#39854=CARTESIAN_POINT('Ctrl Pts',(-0.214004756250064,0.00639858488273828,
0.0103767104892244));
#39855=CARTESIAN_POINT('Ctrl Pts',(-0.214002336625303,0.00636225692718804,
0.0103720655349163));
#39856=CARTESIAN_POINT('Ctrl Pts',(-0.213999917000542,0.0063259289716378,
0.0103674205806083));
#39857=CARTESIAN_POINT('Ctrl Pts',(-0.213998016520098,0.00629630934580017,
0.0103635038297016));
#39858=CARTESIAN_POINT('Ctrl Pts',(-0.213995384865398,0.00625134630123713,
0.010357198392522));
#39859=CARTESIAN_POINT('Ctrl Pts',(-0.213992753210698,0.00620638325667409,
0.0103508929553423));
#39860=CARTESIAN_POINT('Ctrl Pts',(-0.213989394888805,0.00614610502882649,
0.0103419917952826));
#39861=CARTESIAN_POINT('Ctrl Pts',(-0.21398653156378,0.00609034800684164,
0.0103331590792549));
#39862=CARTESIAN_POINT('Ctrl Pts',(-0.213983668238756,0.00603459098485678,
0.0103243263632272));
#39863=CARTESIAN_POINT('Ctrl Pts',(-0.213981296702793,0.00598333124078719,
0.0103157094453065));
#39864=CARTESIAN_POINT('Ctrl Pts',(-0.213979122749828,0.00593168239145384,
0.0103065968143388));
#39865=CARTESIAN_POINT('Ctrl Pts',(-0.213974774843896,0.00582838469278714,
0.0102883715524033));
#39866=CARTESIAN_POINT('Ctrl Pts',(-0.213971220854217,0.00572356184595577,
0.0102679987910534));
#39867=CARTESIAN_POINT('Ctrl Pts',(-0.213968629170881,0.0056214786218438,
0.0102463358658497));
#39868=CARTESIAN_POINT('Ctrl Pts',(-0.213963445804209,0.00541731217361988,
0.0102030100154425));
#39869=CARTESIAN_POINT('Ctrl Pts',(-0.213962101745618,0.00522400033366578,
0.0101549790725054));
#39870=CARTESIAN_POINT('Ctrl Pts',(-0.213964873552575,0.00503030005499574,
0.01010023830303));
#39871=CARTESIAN_POINT('Ctrl Pts',(-0.213967645359531,0.0048365997763257,
0.0100454975335545));
#39872=CARTESIAN_POINT('Ctrl Pts',(-0.213974537218841,0.00464258063418668,
0.00998385461054552));
#39873=CARTESIAN_POINT('Ctrl Pts',(-0.213986279184264,0.00444636027725606,
0.00991397063797153));
#39874=CARTESIAN_POINT('Ctrl Pts',(-0.213992150166976,0.00434825009879075,
0.00987902865168454));
#39875=CARTESIAN_POINT('Ctrl Pts',(-0.2139992347739,0.0042496038046692,
0.00984197597949799));
#39876=CARTESIAN_POINT('Ctrl Pts',(-0.214007169132657,0.00415347647942909,
0.00980399912099018));
#39877=CARTESIAN_POINT('Ctrl Pts',(-0.214011136312036,0.00410541281680903,
0.00978501069173628));
#39878=CARTESIAN_POINT('Ctrl Pts',(-0.214015315205515,0.00405796652499624,
0.00976582446738269));
#39879=CARTESIAN_POINT('Ctrl Pts',(-0.214020163647885,0.00400702271758286,
0.00974467724691843));
#39880=CARTESIAN_POINT('Ctrl Pts',(-0.214025012090255,0.00395607891016948,
0.00972353002645416));
#39881=CARTESIAN_POINT('Ctrl Pts',(-0.214030532775055,0.00390168841775467,
0.00970029807802345));
#39882=CARTESIAN_POINT('Ctrl Pts',(-0.214034858845576,0.00386064793818244,
0.00968241922088636));
#39883=CARTESIAN_POINT('Ctrl Pts',(-0.214039184916098,0.00381960745861021,
0.00966454036374926));
#39884=CARTESIAN_POINT('Ctrl Pts',(-0.214042312567376,0.00379183998995763,
0.0096521893849458));
#39885=CARTESIAN_POINT('Ctrl Pts',(-0.214046191819162,0.00375827537784855,
0.00963707794241496));
#39886=CARTESIAN_POINT('Ctrl Pts',(-0.214050071070949,0.00372471076573947,
0.00962196649988412));
#39887=CARTESIAN_POINT('Ctrl Pts',(-0.214054704007104,0.00368539291187765,
0.00960399886809182));
#39888=CARTESIAN_POINT('Ctrl Pts',(-0.214059615038916,0.00364501315118274,
0.00958515134653227));
#39889=CARTESIAN_POINT('Ctrl Pts',(-0.214069437102542,0.00356425362979292,
0.00954745630341316));
#39890=CARTESIAN_POINT('Ctrl Pts',(-0.21408036893767,0.00347918796641314,
0.00950636164773408));
#39891=CARTESIAN_POINT('Ctrl Pts',(-0.214092773485727,0.00338681699209809,
0.0094596464485715));
#39892=CARTESIAN_POINT('Ctrl Pts',(-0.214117582581841,0.00320207504346799,
0.00936621605024635));
#39893=CARTESIAN_POINT('Ctrl Pts',(-0.214148284403255,0.00298816452839985,
0.00925021741124221));
#39894=CARTESIAN_POINT('Ctrl Pts',(-0.214184674208418,0.00275297203288764,
0.00910660423566295));
#39895=CARTESIAN_POINT('Ctrl Pts',(-0.214184706718132,0.00275296401068821,
0.0091066000178277));
#39896=CARTESIAN_POINT('Ctrl Pts',(-0.213850325206826,0.00275300942663134,
0.00909934875292539));
#39897=CARTESIAN_POINT('Ctrl Pts',(-0.213516724599567,0.00275305138100511,
0.00909211236159907));
#39898=CARTESIAN_POINT('Ctrl Pts',(-0.213184266201433,0.00275308988725477,
0.0090848987175866));
#39899=CARTESIAN_POINT('Origin',(-0.223676757797681,0.00749999628416647,
0.00172570651533405));
#39900=CARTESIAN_POINT('',(-0.22309284651216,0.00749584998232693,0.0106501221268793));
#39901=CARTESIAN_POINT('',(-0.223392296011988,0.00186204391920834,0.00865271087646174));
#39902=CARTESIAN_POINT('Ctrl Pts',(-0.223392296011988,0.00186204391920834,
0.00865271087646174));
#39903=CARTESIAN_POINT('Ctrl Pts',(-0.223319871060027,0.00211980418497422,
0.00886086131836836));
#39904=CARTESIAN_POINT('Ctrl Pts',(-0.223230417685778,0.00247217783692335,
0.00911151291301624));
#39905=CARTESIAN_POINT('Ctrl Pts',(-0.223144978048942,0.00287497601905299,
0.00936251343998583));
#39906=CARTESIAN_POINT('Ctrl Pts',(-0.22310564727859,0.00308846183391502,
0.00948703711985114));
#39907=CARTESIAN_POINT('Ctrl Pts',(-0.22305914643883,0.00341474467215678,
0.00966364610365276));
#39908=CARTESIAN_POINT('Ctrl Pts',(-0.223024306677471,0.00374403882274536,
0.00982342475701909));
#39909=CARTESIAN_POINT('Ctrl Pts',(-0.222996283861068,0.0041018555788969,
0.00998004297101686));
#39910=CARTESIAN_POINT('Ctrl Pts',(-0.222969194008887,0.00463196501065476,
0.0101823328381467));
#39911=CARTESIAN_POINT('Ctrl Pts',(-0.22296083527953,0.00510571723112372,
0.0103269540955497));
#39912=CARTESIAN_POINT('Ctrl Pts',(-0.222966830172775,0.00554467492095415,
0.010432283226809));
#39913=CARTESIAN_POINT('Ctrl Pts',(-0.222973890152792,0.00578493801794152,
0.0104821858289615));
#39914=CARTESIAN_POINT('Ctrl Pts',(-0.222982369849644,0.00598932331249166,
0.0105195922928726));
#39915=CARTESIAN_POINT('Ctrl Pts',(-0.222988213034318,0.00610111321959354,
0.0105379385005546));
#39916=CARTESIAN_POINT('Ctrl Pts',(-0.223000242325119,0.00630906110798175,
0.0105696138144231));
#39917=CARTESIAN_POINT('Ctrl Pts',(-0.223027517337247,0.00671085691261999,
0.0106196318321823));
#39918=CARTESIAN_POINT('Ctrl Pts',(-0.223063339697324,0.00715748003617067,
0.0106493315311508));
#39919=CARTESIAN_POINT('Ctrl Pts',(-0.22309284651216,0.00749584998232693,
0.0106501221268793));
#39920=CARTESIAN_POINT('',(-0.2233982585897,0.013123285512218,0.00866473942159963));
#39921=CARTESIAN_POINT('Ctrl Pts',(-0.223092846396494,0.00749585131677931,
0.0106501221250134));
#39922=CARTESIAN_POINT('Ctrl Pts',(-0.223063630887188,0.00783291331843735,
0.0106496508010981));
#39923=CARTESIAN_POINT('Ctrl Pts',(-0.223028200638697,0.00827785100296254,
0.0106205981598599));
#39924=CARTESIAN_POINT('Ctrl Pts',(-0.223001293631607,0.00867832292771731,
0.0105713108445289));
#39925=CARTESIAN_POINT('Ctrl Pts',(-0.222989468933273,0.00888549981070341,
0.0105400738724192));
#39926=CARTESIAN_POINT('Ctrl Pts',(-0.222983723480319,0.00899722891238163,
0.0105219073079855));
#39927=CARTESIAN_POINT('Ctrl Pts',(-0.222975502745266,0.00919991606191928,
0.0104851529915839));
#39928=CARTESIAN_POINT('Ctrl Pts',(-0.222968716597595,0.00943907010756142,
0.0104359371442604));
#39929=CARTESIAN_POINT('Ctrl Pts',(-0.22296319930633,0.00987692923929947,
0.0103317776510189));
#39930=CARTESIAN_POINT('Ctrl Pts',(-0.222972029344618,0.0103524546158386,
0.0101877530993365));
#39931=CARTESIAN_POINT('Ctrl Pts',(-0.222999554069768,0.0108861515781492,
0.0099850487725875));
#39932=CARTESIAN_POINT('Ctrl Pts',(-0.223027657018532,0.0112442757284449,
0.00982888868406289));
#39933=CARTESIAN_POINT('Ctrl Pts',(-0.223062483445131,0.0115730293585616,
0.00966992388725343));
#39934=CARTESIAN_POINT('Ctrl Pts',(-0.223108468347194,0.0118955673702011,
0.00949610299343309));
#39935=CARTESIAN_POINT('Ctrl Pts',(-0.223148241664016,0.0121105250457455,
0.00937134181568169));
#39936=CARTESIAN_POINT('Ctrl Pts',(-0.223234432572955,0.012513148459596,
0.00912151309303764));
#39937=CARTESIAN_POINT('Ctrl Pts',(-0.223324944071789,0.0128655990519436,
0.0088719056596678));
#39938=CARTESIAN_POINT('Ctrl Pts',(-0.2233982585897,0.013123285512218,0.00866473942159963));
#39939=CARTESIAN_POINT('',(-0.224398127361235,0.0131227913316661,0.0086866275128953));
#39940=CARTESIAN_POINT('Ctrl Pts',(-0.223398249886961,0.0131232867503721,
0.00866473823159148));
#39941=CARTESIAN_POINT('Ctrl Pts',(-0.223731523675107,0.0131231213967512,
0.00867203444050197));
#39942=CARTESIAN_POINT('Ctrl Pts',(-0.22406487360808,0.0131229619290297,
0.00867932750749511));
#39943=CARTESIAN_POINT('Ctrl Pts',(-0.224398096141527,0.013122808446012,
0.00868661298034067));
#39944=CARTESIAN_POINT('',(-0.224092572998184,0.00749536846703943,0.0106715944441166));
#39945=CARTESIAN_POINT('Ctrl Pts',(-0.224398127361235,0.0131227913316661,
0.0086866275128953));
#39946=CARTESIAN_POINT('Ctrl Pts',(-0.224325062414434,0.012865842986752,
0.00889316997404273));
#39947=CARTESIAN_POINT('Ctrl Pts',(-0.224234820704135,0.0125144219497046,
0.00914211665554571));
#39948=CARTESIAN_POINT('Ctrl Pts',(-0.224148755853197,0.0121126796310063,
0.00939153056882088));
#39949=CARTESIAN_POINT('Ctrl Pts',(-0.224109017097858,0.0118984407581323,
0.00951597785856116));
#39950=CARTESIAN_POINT('Ctrl Pts',(-0.224062783214931,0.0115753502059685,
0.0096902410433109));
#39951=CARTESIAN_POINT('Ctrl Pts',(-0.224027819291741,0.0112462212233988,
0.00984947839760243));
#39952=CARTESIAN_POINT('Ctrl Pts',(-0.22399959162762,0.0108878152232127,
0.010005881088725));
#39953=CARTESIAN_POINT('Ctrl Pts',(-0.223971919420138,0.0103523511641684,
0.0102092626278178));
#39954=CARTESIAN_POINT('Ctrl Pts',(-0.223963160381509,0.00988219899480068,
0.0103516928623865));
#39955=CARTESIAN_POINT('Ctrl Pts',(-0.223968441757534,0.0094464451478849,
0.0104557627503415));
#39956=CARTESIAN_POINT('Ctrl Pts',(-0.223975077093011,0.00920839189318166,
0.010504967431807));
#39957=CARTESIAN_POINT('Ctrl Pts',(-0.223983110990325,0.00900703426964022,
0.0105417005683667));
#39958=CARTESIAN_POINT('Ctrl Pts',(-0.223988835346065,0.0088942902955332,
0.0105601622854623));
#39959=CARTESIAN_POINT('Ctrl Pts',(-0.224000615907753,0.00868625901717492,
0.0105917267871887));
#39960=CARTESIAN_POINT('Ctrl Pts',(-0.22402755697167,0.0082832671038718,
0.010641668948832));
#39961=CARTESIAN_POINT('Ctrl Pts',(-0.224063163807534,0.00783511181037311,
0.0106711391391908));
#39962=CARTESIAN_POINT('Ctrl Pts',(-0.224092572998184,0.00749536846703943,
0.0106715944441166));
#39963=CARTESIAN_POINT('',(-0.224391698001265,0.00186171520950775,0.0086738967910923));
#39964=CARTESIAN_POINT('Ctrl Pts',(-0.224092573136878,0.00749536686481965,
0.0106715944462637));
#39965=CARTESIAN_POINT('Ctrl Pts',(-0.224063181659026,0.00715789448494786,
0.0106707879238547));
#39966=CARTESIAN_POINT('Ctrl Pts',(-0.224027485085123,0.00671245635685632,
0.0106412153002841));
#39967=CARTESIAN_POINT('Ctrl Pts',(-0.224000282681402,0.00631182732071981,
0.0105914571765522));
#39968=CARTESIAN_POINT('Ctrl Pts',(-0.223988268398574,0.00610438871051628,
0.0105599315069899));
#39969=CARTESIAN_POINT('Ctrl Pts',(-0.223982438964663,0.00599317088837536,
0.0105417285207031));
#39970=CARTESIAN_POINT('Ctrl Pts',(-0.223973911582342,0.0057884503761421,
0.0105043511524616));
#39971=CARTESIAN_POINT('Ctrl Pts',(-0.223966812223066,0.00554799671714812,
0.0104545007048094));
#39972=CARTESIAN_POINT('Ctrl Pts',(-0.223960725771381,0.00510876621667219,
0.0103493125263479));
#39973=CARTESIAN_POINT('Ctrl Pts',(-0.223969092055907,0.00463281516023792,
0.0102040504815577));
#39974=CARTESIAN_POINT('Ctrl Pts',(-0.223995910584984,0.00410544707731089,
0.0100029403064932));
#39975=CARTESIAN_POINT('Ctrl Pts',(-0.224023629066248,0.00374891304215397,
0.00984712705576497));
#39976=CARTESIAN_POINT('Ctrl Pts',(-0.224058140037829,0.00342059928890112,
0.00968806171234968));
#39977=CARTESIAN_POINT('Ctrl Pts',(-0.224103946844588,0.00309637190744777,
0.00951295535214167));
#39978=CARTESIAN_POINT('Ctrl Pts',(-0.224143508176959,0.00288006695304061,
0.00938706853711633));
#39979=CARTESIAN_POINT('Ctrl Pts',(-0.224229127635015,0.00247511074954968,
0.00913501513009971));
#39980=CARTESIAN_POINT('Ctrl Pts',(-0.224318956776766,0.00212070098651109,
0.00888305882592809));
#39981=CARTESIAN_POINT('Ctrl Pts',(-0.224391698001265,0.00186171520950775,
0.0086738967910923));
#39982=CARTESIAN_POINT('Ctrl Pts',(-0.224391663297086,0.00186170374604395,
0.0086738867188744));
#39983=CARTESIAN_POINT('Ctrl Pts',(-0.224058368109329,0.00186182240933105,
0.00866682869105414));
#39984=CARTESIAN_POINT('Ctrl Pts',(-0.223725161158108,0.00186193524227883,
0.0086597678079791));
#39985=CARTESIAN_POINT('Ctrl Pts',(-0.223392285411273,0.00186204218687632,
0.00865270923953699));
#39986=CARTESIAN_POINT('Origin',(-0.211568383091034,0.00749999976424864,
0.00128327533895461));
#39987=CARTESIAN_POINT('',(-0.2110965359026,0.00749997454127243,0.0103787827909976));
#39988=CARTESIAN_POINT('',(-0.211183402636931,0.00275068069530849,0.00904332274846592));
#39989=CARTESIAN_POINT('Ctrl Pts',(-0.211183402636931,0.00275068069530849,
0.00904332274846592));
#39990=CARTESIAN_POINT('Ctrl Pts',(-0.211147095219407,0.00298515572002027,
0.00918594988314655));
#39991=CARTESIAN_POINT('Ctrl Pts',(-0.211101192602613,0.00330488634667183,
0.00935868020099563));
#39992=CARTESIAN_POINT('Ctrl Pts',(-0.211063143045044,0.00360117936401887,
0.00950160180870966));
#39993=CARTESIAN_POINT('Ctrl Pts',(-0.21104475417619,0.0037577018790529,
0.00957289220178136));
#39994=CARTESIAN_POINT('Ctrl Pts',(-0.211035467150038,0.00384039342259991,
0.00960968445757509));
#39995=CARTESIAN_POINT('Ctrl Pts',(-0.211019066687301,0.0040029883061291,
0.00967908598737613));
#39996=CARTESIAN_POINT('Ctrl Pts',(-0.211002549970838,0.00419272029530249,
0.00975560521859346));
#39997=CARTESIAN_POINT('Ctrl Pts',(-0.210978116351287,0.00453848546937588,
0.00988555577385184));
#39998=CARTESIAN_POINT('Ctrl Pts',(-0.210961424663072,0.00503260509810232,
0.0100417888938481));
#39999=CARTESIAN_POINT('Ctrl Pts',(-0.210965443153373,0.00551404341866351,
0.0101610108572086));
#40000=CARTESIAN_POINT('Ctrl Pts',(-0.210978272865404,0.00588224623587764,
0.0102322905439714));
#40001=CARTESIAN_POINT('Ctrl Pts',(-0.210987956400489,0.00608781575055283,
0.0102667980265165));
#40002=CARTESIAN_POINT('Ctrl Pts',(-0.210998218524945,0.00626946825961742,
0.0102934418192037));
#40003=CARTESIAN_POINT('Ctrl Pts',(-0.211003938107319,0.00635797387487456,
0.0103049979326545));
#40004=CARTESIAN_POINT('Ctrl Pts',(-0.211015693571684,0.00653001085820023,
0.010326006931539));
#40005=CARTESIAN_POINT('Ctrl Pts',(-0.211040617677658,0.0068586970342682,
0.0103587408428194));
#40006=CARTESIAN_POINT('Ctrl Pts',(-0.211071626779655,0.00722383932448257,
0.0103782401381245));
#40007=CARTESIAN_POINT('Ctrl Pts',(-0.2110965359026,0.00749997454127243,
0.0103787827909976));
#40008=CARTESIAN_POINT('',(-0.21118417804845,0.0122471792256319,0.009044647334993));
#40009=CARTESIAN_POINT('Ctrl Pts',(-0.211096535799883,0.00749997567494527,
0.010378782788766));
#40010=CARTESIAN_POINT('Ctrl Pts',(-0.211071573366554,0.00777549325047854,
0.0103782404346483));
#40011=CARTESIAN_POINT('Ctrl Pts',(-0.211040513267916,0.00813985761538285,
0.0103588270763272));
#40012=CARTESIAN_POINT('Ctrl Pts',(-0.211015576714647,0.00846798462518059,
0.0103262153638346));
#40013=CARTESIAN_POINT('Ctrl Pts',(-0.211003834816079,0.00863970531938501,
0.0103052888750913));
#40014=CARTESIAN_POINT('Ctrl Pts',(-0.210998116574614,0.00872823661427716,
0.0102937495397744));
#40015=CARTESIAN_POINT('Ctrl Pts',(-0.210987925682693,0.00890910709332001,
0.0102672755357513));
#40016=CARTESIAN_POINT('Ctrl Pts',(-0.210978321795415,0.00911419488984098,
0.010232927644559));
#40017=CARTESIAN_POINT('Ctrl Pts',(-0.21096565564001,0.00948174160645032,
0.0101619632965175));
#40018=CARTESIAN_POINT('Ctrl Pts',(-0.210961963015379,0.00996543783438438,
0.0100423573285345));
#40019=CARTESIAN_POINT('Ctrl Pts',(-0.210978912084468,0.0104576617459814,
0.0098868796580418));
#40020=CARTESIAN_POINT('Ctrl Pts',(-0.211003457455194,0.0108036566335765,
0.00975703895053704));
#40021=CARTESIAN_POINT('Ctrl Pts',(-0.211020020345204,0.0109935540978411,
0.00968054497958633));
#40022=CARTESIAN_POINT('Ctrl Pts',(-0.211036452134397,0.0111564247405211,
0.00961110274277066));
#40023=CARTESIAN_POINT('Ctrl Pts',(-0.211045742641945,0.0112392207523565,
0.00957430044553631));
#40024=CARTESIAN_POINT('Ctrl Pts',(-0.211064129984168,0.0113959395659256,
0.00950298930486255));
#40025=CARTESIAN_POINT('Ctrl Pts',(-0.211102140859678,0.0116925422723936,
0.00936004108598765));
#40026=CARTESIAN_POINT('Ctrl Pts',(-0.211147954901023,0.0120125365367652,
0.00918728999384757));
#40027=CARTESIAN_POINT('Ctrl Pts',(-0.21118417804845,0.0122471792256319,
0.009044647334993));
#40028=CARTESIAN_POINT('',(-0.212184953537621,0.0122473744306414,0.00906630151341282));
#40029=CARTESIAN_POINT('Ctrl Pts',(-0.21118422788918,0.0122471764791729,
0.00904465009819522));
#40030=CARTESIAN_POINT('Ctrl Pts',(-0.211517519859832,0.0122472431453679,
0.00905186065814718));
#40031=CARTESIAN_POINT('Ctrl Pts',(-0.211851190949066,0.0122473134521283,
0.00905907723991485));
#40032=CARTESIAN_POINT('Ctrl Pts',(-0.212184989270622,0.0122473873638838,
0.00906629438464372));
#40033=CARTESIAN_POINT('',(-0.212096216935387,0.00749993309271591,0.010400531159228));
#40034=CARTESIAN_POINT('Ctrl Pts',(-0.212184953537621,0.0122473744306414,
0.00906630151341282));
#40035=CARTESIAN_POINT('Ctrl Pts',(-0.212148608862081,0.0120119705243528,
0.00920941487666883));
#40036=CARTESIAN_POINT('Ctrl Pts',(-0.212117954036947,0.0117979090212747,
0.00932500833085451));
#40037=CARTESIAN_POINT('Ctrl Pts',(-0.212093189286655,0.0116130124708475,
0.00941812959134124));
#40038=CARTESIAN_POINT('Ctrl Pts',(-0.212080806911509,0.0115205641956338,
0.0094646902215846));
#40039=CARTESIAN_POINT('Ctrl Pts',(-0.212069896597886,0.0114354199872055,
0.00950565381710398));
#40040=CARTESIAN_POINT('Ctrl Pts',(-0.212060100467986,0.0113546092190502,
0.00954321884104617));
#40041=CARTESIAN_POINT('Ctrl Pts',(-0.212055202403036,0.0113142038349725,
0.00956200135301727));
#40042=CARTESIAN_POINT('Ctrl Pts',(-0.212050583528796,0.0112748674132463,
0.00957990458571435));
#40043=CARTESIAN_POINT('Ctrl Pts',(-0.212046712568544,0.0112412478030318,
0.00959497929731873));
#40044=CARTESIAN_POINT('Ctrl Pts',(-0.212042841608291,0.0112076281928174,
0.00961005400892311));
#40045=CARTESIAN_POINT('Ctrl Pts',(-0.212039716504683,0.0111797685814931,
0.0096223947625136));
#40046=CARTESIAN_POINT('Ctrl Pts',(-0.212035415305258,0.0111387765475974,
0.00964018017975509));
#40047=CARTESIAN_POINT('Ctrl Pts',(-0.212031114105832,0.0110977845137017,
0.00965796559699658));
#40048=CARTESIAN_POINT('Ctrl Pts',(-0.212025640550936,0.0110435846392935,
0.00968102375737418));
#40049=CARTESIAN_POINT('Ctrl Pts',(-0.212020830685943,0.0109927516904921,
0.0097020431984729));
#40050=CARTESIAN_POINT('Ctrl Pts',(-0.212016020820949,0.0109419187416906,
0.00972306263957162));
#40051=CARTESIAN_POINT('Ctrl Pts',(-0.212011872008556,0.010894502303713,
0.00974216458214745));
#40052=CARTESIAN_POINT('Ctrl Pts',(-0.212007934174403,0.0108464578821206,
0.00976107397304423));
#40053=CARTESIAN_POINT('Ctrl Pts',(-0.212000058506097,0.0107503690389357,
0.00979889275483778));
#40054=CARTESIAN_POINT('Ctrl Pts',(-0.211993029531615,0.010651721257402,
0.00983581351009456));
#40055=CARTESIAN_POINT('Ctrl Pts',(-0.211987203427364,0.0105533047573211,
0.00987073287076495));
#40056=CARTESIAN_POINT('Ctrl Pts',(-0.211975551218862,0.0103564717571592,
0.00994057159210573));
#40057=CARTESIAN_POINT('Ctrl Pts',(-0.211968707612936,0.0101605940883872,
0.0100025370378822));
#40058=CARTESIAN_POINT('Ctrl Pts',(-0.211965975423112,0.0099663576093433,
0.0100571576241214));
#40059=CARTESIAN_POINT('Ctrl Pts',(-0.211963243233289,0.00977212113029945,
0.0101117782103606));
#40060=CARTESIAN_POINT('Ctrl Pts',(-0.211964616403369,0.0095796185691958,
0.0101593323058388));
#40061=CARTESIAN_POINT('Ctrl Pts',(-0.211969788366012,0.00937629259852591,
0.01020228070507));
#40062=CARTESIAN_POINT('Ctrl Pts',(-0.211972374347333,0.00927462961319097,
0.0102237549046856));
#40063=CARTESIAN_POINT('Ctrl Pts',(-0.211975912663703,0.0091702339273998,
0.0102439564753252));
#40064=CARTESIAN_POINT('Ctrl Pts',(-0.21198024063847,0.00906742206628467,
0.0102620249393407));
#40065=CARTESIAN_POINT('Ctrl Pts',(-0.211982404625853,0.00901601613572711,
0.0102710591713484));
#40066=CARTESIAN_POINT('Ctrl Pts',(-0.211984765148223,0.00896501374588465,
0.0102796005580246));
#40067=CARTESIAN_POINT('Ctrl Pts',(-0.211987610756156,0.00890961963149956,
0.0102883465429082));
#40068=CARTESIAN_POINT('Ctrl Pts',(-0.211990456364088,0.00885422551711447,
0.0102970925277919));
#40069=CARTESIAN_POINT('Ctrl Pts',(-0.21199379016818,0.00879441655146242,
0.0103059001321234));
#40070=CARTESIAN_POINT('Ctrl Pts',(-0.211996413112179,0.00874961583566324,
0.0103121670340523));
#40071=CARTESIAN_POINT('Ctrl Pts',(-0.211999036056178,0.00870481511986407,
0.0103184339359812));
#40072=CARTESIAN_POINT('Ctrl Pts',(-0.212000943752514,0.00867505009895193,
0.0103223618108506));
#40073=CARTESIAN_POINT('Ctrl Pts',(-0.212003363382826,0.0086386498772624,
0.0103270043852339));
#40074=CARTESIAN_POINT('Ctrl Pts',(-0.212005783013139,0.00860224965557287,
0.0103316469596172));
#40075=CARTESIAN_POINT('Ctrl Pts',(-0.21200871695817,0.00855920099241481,
0.0103368948021386));
#40076=CARTESIAN_POINT('Ctrl Pts',(-0.212011866469682,0.00851480072693946,
0.0103419449315219));
#40077=CARTESIAN_POINT('Ctrl Pts',(-0.212018165492707,0.00842600019598875,
0.0103520451902885));
#40078=CARTESIAN_POINT('Ctrl Pts',(-0.212025323759104,0.00833180673148592,
0.0103614935292938));
#40079=CARTESIAN_POINT('Ctrl Pts',(-0.212033577950091,0.00822830849881047,
0.0103699817552531));
#40080=CARTESIAN_POINT('Ctrl Pts',(-0.212050086332064,0.00802131203345956,
0.0103869582071715));
#40081=CARTESIAN_POINT('Ctrl Pts',(-0.212070980805244,0.00777709603119313,
0.0103999842177033));
#40082=CARTESIAN_POINT('Ctrl Pts',(-0.212096216935389,0.00749993309273471,
0.0104005311592281));
#40083=CARTESIAN_POINT('',(-0.212183765169463,0.00275128401172433,0.00906545360362375));
#40084=CARTESIAN_POINT('Ctrl Pts',(-0.212096216935387,0.00749993309271591,
0.010400531159228));
#40085=CARTESIAN_POINT('Ctrl Pts',(-0.212071126307345,0.00722322961499376,
0.0103999832300892));
#40086=CARTESIAN_POINT('Ctrl Pts',(-0.212050323820085,0.00697932624712693,
0.0103869945506515));
#40087=CARTESIAN_POINT('Ctrl Pts',(-0.212033859878558,0.00677255811334454,
0.0103700572244492));
#40088=CARTESIAN_POINT('Ctrl Pts',(-0.212025627907794,0.00666917404645334,
0.0103615885613481));
#40089=CARTESIAN_POINT('Ctrl Pts',(-0.212018479948959,0.00657507361336468,
0.010352161442409));
#40090=CARTESIAN_POINT('Ctrl Pts',(-0.212012174388185,0.00648628210784819,
0.0103420727979329));
#40091=CARTESIAN_POINT('Ctrl Pts',(-0.212009021607799,0.00644188635508995,
0.0103370284756949));
#40092=CARTESIAN_POINT('Ctrl Pts',(-0.212006080193597,0.00639882124771468,
0.0103317835311436));
#40093=CARTESIAN_POINT('Ctrl Pts',(-0.212003655779862,0.00636247064645391,
0.010327151684048));
#40094=CARTESIAN_POINT('Ctrl Pts',(-0.212001231366128,0.00632612004519314,
0.0103225198369524));
#40095=CARTESIAN_POINT('Ctrl Pts',(-0.211999321532852,0.0062964705099328,
0.0103186123262797));
#40096=CARTESIAN_POINT('Ctrl Pts',(-0.211996671040146,0.00625149580262887,
0.010312326350296));
#40097=CARTESIAN_POINT('Ctrl Pts',(-0.211994020547439,0.00620652109532495,
0.0103060403743122));
#40098=CARTESIAN_POINT('Ctrl Pts',(-0.211990633880624,0.00614624923462854,
0.0102971697588912));
#40099=CARTESIAN_POINT('Ctrl Pts',(-0.21198774295475,0.00609049435275109,
0.0102883669432379));
#40100=CARTESIAN_POINT('Ctrl Pts',(-0.211984852028876,0.00603473947087364,
0.0102795641275845));
#40101=CARTESIAN_POINT('Ctrl Pts',(-0.211982453651153,0.00598347782917449,
0.0102709758732188));
#40102=CARTESIAN_POINT('Ctrl Pts',(-0.211980251215045,0.00593181943961855,
0.0102618921530657));
#40103=CARTESIAN_POINT('Ctrl Pts',(-0.211975846342829,0.00582850266050667,
0.0102437247127595));
#40104=CARTESIAN_POINT('Ctrl Pts',(-0.21197222883814,0.00572363000883807,
0.0102234098804427));
#40105=CARTESIAN_POINT('Ctrl Pts',(-0.21196956741466,0.00562157793695026,
0.010201826560603));
#40106=CARTESIAN_POINT('Ctrl Pts',(-0.2119642445677,0.00541747379317463,
0.0101586599209237));
#40107=CARTESIAN_POINT('Ctrl Pts',(-0.211962735409498,0.00522454320374596,
0.010110908237939));
#40108=CARTESIAN_POINT('Ctrl Pts',(-0.211965334255942,0.00503024391291162,
0.0100561856635299));
#40109=CARTESIAN_POINT('Ctrl Pts',(-0.211967933102386,0.00483594462207727,
0.0100014630891208));
#40110=CARTESIAN_POINT('Ctrl Pts',(-0.211974645886691,0.00464036808754224,
0.00993949688927384));
#40111=CARTESIAN_POINT('Ctrl Pts',(-0.211986174288779,0.0044439250258746,
0.00986972273612033));
#40112=CARTESIAN_POINT('Ctrl Pts',(-0.211991938489823,0.00434570349504078,
0.00983483565954358));
#40113=CARTESIAN_POINT('Ctrl Pts',(-0.211998907343389,0.00424727340981272,
0.00979796220794339));
#40114=CARTESIAN_POINT('Ctrl Pts',(-0.212006726980613,0.00415142401522088,
0.00976020909830612));
#40115=CARTESIAN_POINT('Ctrl Pts',(-0.212010636799224,0.00410349931792496,
0.00974133254348749));
#40116=CARTESIAN_POINT('Ctrl Pts',(-0.212014758624468,0.00405620812295089,
0.00972226775875776));
#40117=CARTESIAN_POINT('Ctrl Pts',(-0.212019538220643,0.00400553612295486,
0.00970130241315875));
#40118=CARTESIAN_POINT('Ctrl Pts',(-0.212024317816818,0.00395486412295883,
0.00968033706755973));
#40119=CARTESIAN_POINT('Ctrl Pts',(-0.212029757792179,0.00390086039173556,
0.00965735126569874));
#40120=CARTESIAN_POINT('Ctrl Pts',(-0.212034039987089,0.00385996834286666,
0.00963960170087009));
#40121=CARTESIAN_POINT('Ctrl Pts',(-0.212038322181999,0.00381907629399776,
0.00962185213604143));
#40122=CARTESIAN_POINT('Ctrl Pts',(-0.212041442891325,0.00379122118675441,
0.00960950912507693));
#40123=CARTESIAN_POINT('Ctrl Pts',(-0.212045308742462,0.00375762262362403,
0.00959443826985068));
#40124=CARTESIAN_POINT('Ctrl Pts',(-0.2120491745936,0.00372402406049364,
0.00957936741462442));
#40125=CARTESIAN_POINT('Ctrl Pts',(-0.21205378762908,0.0036847249345285,
0.00956147482426794));
#40126=CARTESIAN_POINT('Ctrl Pts',(-0.212058682884334,0.00364434597571046,
0.00954269834621542));
#40127=CARTESIAN_POINT('Ctrl Pts',(-0.212068473394842,0.00356358805807439,
0.00950514539011038));
#40128=CARTESIAN_POINT('Ctrl Pts',(-0.212079390220398,0.00347845353315219,
0.00946417474742));
#40129=CARTESIAN_POINT('Ctrl Pts',(-0.212091788556574,0.00338599268517819,
0.00941759379839564));
#40130=CARTESIAN_POINT('Ctrl Pts',(-0.212116585228927,0.00320107098923018,
0.00932443190034691));
#40131=CARTESIAN_POINT('Ctrl Pts',(-0.212147309727277,0.00298689421470239,
0.00920874679129024));
#40132=CARTESIAN_POINT('Ctrl Pts',(-0.212183765169463,0.00275128401172433,
0.00906545360362375));
#40133=CARTESIAN_POINT('Ctrl Pts',(-0.212183802162308,0.00275127625620254,
0.00906544966550962));
#40134=CARTESIAN_POINT('Ctrl Pts',(-0.211850395705467,0.00275108062549403,
0.00905807711035799));
#40135=CARTESIAN_POINT('Ctrl Pts',(-0.211516878203266,0.00275088152870816,
0.00905070000977781));
#40136=CARTESIAN_POINT('Ctrl Pts',(-0.211183457783125,0.0027506790911641,
0.00904332296693787));
#40137=CARTESIAN_POINT('Origin',(-0.201568052764461,0.00749999926826592,
0.000898602350899668));
#40138=CARTESIAN_POINT('',(-0.201099819882141,0.00749914619770346,0.0101529062582246));
#40139=CARTESIAN_POINT('',(-0.201180426584977,0.0027404758504493,0.00883792993396412));
#40140=CARTESIAN_POINT('Ctrl Pts',(-0.201180426584977,0.0027404758504493,
0.00883792993396412));
#40141=CARTESIAN_POINT('Ctrl Pts',(-0.201143782776895,0.00297687352666821,
0.00897876952690809));
#40142=CARTESIAN_POINT('Ctrl Pts',(-0.201098326821028,0.00329208064462831,
0.00914639237872595));
#40143=CARTESIAN_POINT('Ctrl Pts',(-0.201053656234426,0.00364905443742606,
0.00931418085756173));
#40144=CARTESIAN_POINT('Ctrl Pts',(-0.2010333398498,0.00382564426305905,
0.00939269762319622));
#40145=CARTESIAN_POINT('Ctrl Pts',(-0.201004911345248,0.0041388485598608,
0.00952147497706033));
#40146=CARTESIAN_POINT('Ctrl Pts',(-0.200980856006014,0.00451692057273125,
0.00966086163852431));
#40147=CARTESIAN_POINT('Ctrl Pts',(-0.200965882884491,0.00504039570807835,
0.00982439009474785));
#40148=CARTESIAN_POINT('Ctrl Pts',(-0.200972067968975,0.00550094059850311,
0.0099359440718681));
#40149=CARTESIAN_POINT('Ctrl Pts',(-0.200985770459153,0.00587373777427713,
0.010007547779862));
#40150=CARTESIAN_POINT('Ctrl Pts',(-0.200995828352292,0.00608227698546498,
0.0100420971753329));
#40151=CARTESIAN_POINT('Ctrl Pts',(-0.201006404478933,0.0062689806201438,
0.0100690695042997));
#40152=CARTESIAN_POINT('Ctrl Pts',(-0.201012027549101,0.00635736976848426,
0.0100803938087593));
#40153=CARTESIAN_POINT('Ctrl Pts',(-0.201023530642222,0.0065306602030437,
0.0101011948342447));
#40154=CARTESIAN_POINT('Ctrl Pts',(-0.2010474121427,0.0068598642396664,
0.0101333483495882));
#40155=CARTESIAN_POINT('Ctrl Pts',(-0.201076578870104,0.0072242446465652,
0.0101523770736324));
#40156=CARTESIAN_POINT('Ctrl Pts',(-0.201099819882141,0.00749914619770346,
0.0101529062582246));
#40157=CARTESIAN_POINT('',(-0.201177053601335,0.0122550060276839,0.00884070721774072));
#40158=CARTESIAN_POINT('Ctrl Pts',(-0.201099415026176,0.00749913299764412,
0.0101528974791025));
#40159=CARTESIAN_POINT('Ctrl Pts',(-0.201096555619577,0.00753150741933934,
0.0101528385065419));
#40160=CARTESIAN_POINT('Ctrl Pts',(-0.201093736994948,0.00756388495100858,
0.0101526106398872));
#40161=CARTESIAN_POINT('Ctrl Pts',(-0.201087666450416,0.00763453987982649,
0.0101517444674804));
#40162=CARTESIAN_POINT('Ctrl Pts',(-0.201084429222973,0.00767281663265906,
0.010151038985735));
#40163=CARTESIAN_POINT('Ctrl Pts',(-0.201080801334986,0.0077163098527908,
0.0101499685939465));
#40164=CARTESIAN_POINT('Ctrl Pts',(-0.201080366927711,0.00772152768394031,
0.0101498357845174));
#40165=CARTESIAN_POINT('Ctrl Pts',(-0.201079462914577,0.00773240637854102,
0.0101495497227957));
#40166=CARTESIAN_POINT('Ctrl Pts',(-0.201078993452857,0.0077380672302977,
0.0101493956923408));
#40167=CARTESIAN_POINT('Ctrl Pts',(-0.201077400593704,0.00775731229740116,
0.0101488544418675));
#40168=CARTESIAN_POINT('Ctrl Pts',(-0.201076281646611,0.00777089616598205,
0.0101484426009006));
#40169=CARTESIAN_POINT('Ctrl Pts',(-0.201071551307129,0.00782858173595134,
0.0101465670310501));
#40170=CARTESIAN_POINT('Ctrl Pts',(-0.201067988458377,0.007872677626471,
0.0101448189497164));
#40171=CARTESIAN_POINT('Ctrl Pts',(-0.201053871077008,0.00804952410981167,
0.010136545542321));
#40172=CARTESIAN_POINT('Ctrl Pts',(-0.201043541456728,0.0081825036848605,
0.0101274548226958));
#40173=CARTESIAN_POINT('Ctrl Pts',(-0.201032352560321,0.00833284176583748,
0.0101139327363592));
#40174=CARTESIAN_POINT('Ctrl Pts',(-0.201031018431873,0.00835090027672925,
0.0101122552185723));
#40175=CARTESIAN_POINT('Ctrl Pts',(-0.201022652850357,0.00846509755040904,
0.0101013102262794));
#40176=CARTESIAN_POINT('Ctrl Pts',(-0.201015937700995,0.00856111993260325,
0.0100905968298343));
#40177=CARTESIAN_POINT('Ctrl Pts',(-0.201001522417578,0.00878472981437558,
0.0100621250456051));
#40178=CARTESIAN_POINT('Ctrl Pts',(-0.200994315161741,0.00891158178381539,
0.0100433010725122));
#40179=CARTESIAN_POINT('Ctrl Pts',(-0.200984966053877,0.00910857513732452,
0.0100099106717903));
#40180=CARTESIAN_POINT('Ctrl Pts',(-0.200982001710847,0.00917864056758256,
0.00999721021346039));
#40181=CARTESIAN_POINT('Ctrl Pts',(-0.200976604379606,0.00932560861946987,
0.00996883327826301));
#40182=CARTESIAN_POINT('Ctrl Pts',(-0.200974256328178,0.00940247516841393,
0.00995298677241071));
#40183=CARTESIAN_POINT('Ctrl Pts',(-0.200968526789994,0.00964294760988883,
0.0099002516080076));
#40184=CARTESIAN_POINT('Ctrl Pts',(-0.200967003526247,0.00980579664254104,
0.00985992759696585));
#40185=CARTESIAN_POINT('Ctrl Pts',(-0.20096903863634,0.0100680083654313,
0.00978748245514171));
#40186=CARTESIAN_POINT('Ctrl Pts',(-0.200970898955289,0.0101677912935188,
0.00975811362521028));
#40187=CARTESIAN_POINT('Ctrl Pts',(-0.200979011841939,0.0104409498990722,
0.00967275625057537));
#40188=CARTESIAN_POINT('Ctrl Pts',(-0.200987498960234,0.0106129719117605,
0.00961344672677827));
#40189=CARTESIAN_POINT('Ctrl Pts',(-0.201017172577816,0.0110403688905056,
0.00945204240146106));
#40190=CARTESIAN_POINT('Ctrl Pts',(-0.201042813248034,0.0112880111477272,
0.00934589777805525));
#40191=CARTESIAN_POINT('Ctrl Pts',(-0.201075293812801,0.0115421151804829,
0.00922361425713881));
#40192=CARTESIAN_POINT('Ctrl Pts',(-0.201076280881285,0.011549797704654,
0.00921990414749716));
#40193=CARTESIAN_POINT('Ctrl Pts',(-0.201079194491396,0.011572363930971,
0.00920896798108764));
#40194=CARTESIAN_POINT('Ctrl Pts',(-0.201081132455913,0.0115872323483612,
0.00920171333031922));
#40195=CARTESIAN_POINT('Ctrl Pts',(-0.201097568219318,0.0117122511540107,
0.00914030016243677));
#40196=CARTESIAN_POINT('Ctrl Pts',(-0.201112835939432,0.0118218912000811,
0.00908371368776426));
#40197=CARTESIAN_POINT('Ctrl Pts',(-0.201133528613954,0.011965820847289,
0.00900576141837299));
#40198=CARTESIAN_POINT('Ctrl Pts',(-0.201138749565774,0.0120016723198076,
0.00898603600794796));
#40199=CARTESIAN_POINT('Ctrl Pts',(-0.201147172122991,0.0120587248794593,
0.00895415204620798));
#40200=CARTESIAN_POINT('Ctrl Pts',(-0.201150340696306,0.0120800145739369,
0.0089421434805461));
#40201=CARTESIAN_POINT('Ctrl Pts',(-0.201155474346223,0.0121142184060044,
0.00892267196211884));
#40202=CARTESIAN_POINT('Ctrl Pts',(-0.201157427314594,0.0121271638790092,
0.00891526094768469));
#40203=CARTESIAN_POINT('Ctrl Pts',(-0.201159756324221,0.0121425212968394,
0.0089064198753503));
#40204=CARTESIAN_POINT('Ctrl Pts',(-0.20116012521612,0.0121449513662034,
0.00890501944645919));
#40205=CARTESIAN_POINT('Ctrl Pts',(-0.201165961618878,0.0121833606018225,
0.00888286129962451));
#40206=CARTESIAN_POINT('Ctrl Pts',(-0.201171486576948,0.0122191939011565,
0.00886186694378061));
#40207=CARTESIAN_POINT('Ctrl Pts',(-0.201177074329032,0.0122548777933217,
0.00884063698486466));
#40208=CARTESIAN_POINT('',(-0.202178357934375,0.0122547990652915,0.00886239654148025));
#40209=CARTESIAN_POINT('Ctrl Pts',(-0.201177075042786,0.0122548774470157,
0.00884063720755112));
#40210=CARTESIAN_POINT('Ctrl Pts',(-0.201513398686541,0.0122548513903108,
0.00884794584758545));
#40211=CARTESIAN_POINT('Ctrl Pts',(-0.201847382617857,0.0122548298057659,
0.00885520107578513));
#40212=CARTESIAN_POINT('Ctrl Pts',(-0.202178423329881,0.0122548125338768,
0.00886238990093067));
#40213=CARTESIAN_POINT('',(-0.20209947962974,0.0074995037887144,0.0101745804416663));
#40214=CARTESIAN_POINT('Ctrl Pts',(-0.202178357934375,0.0122547990652915,
0.00886239654148025));
#40215=CARTESIAN_POINT('Ctrl Pts',(-0.202141594099432,0.0120170628854501,
0.0090038431709906));
#40216=CARTESIAN_POINT('Ctrl Pts',(-0.202096005540814,0.0116999888925394,
0.0091720983007729));
#40217=CARTESIAN_POINT('Ctrl Pts',(-0.202051299589304,0.0113413832046676,
0.00934019418830925));
#40218=CARTESIAN_POINT('Ctrl Pts',(-0.202030922651275,0.0111631559854859,
0.00941915423537262));
#40219=CARTESIAN_POINT('Ctrl Pts',(-0.202002813441514,0.0108513628693672,
0.00954689664555636));
#40220=CARTESIAN_POINT('Ctrl Pts',(-0.201978982212522,0.0104745530127929,
0.00968535788947888));
#40221=CARTESIAN_POINT('Ctrl Pts',(-0.201964231695163,0.00995451013132065,
0.00984735855643358));
#40222=CARTESIAN_POINT('Ctrl Pts',(-0.201970487645389,0.00949571672073084,
0.00995827983118732));
#40223=CARTESIAN_POINT('Ctrl Pts',(-0.20198422225347,0.00912548553395714,
0.0100293214390935));
#40224=CARTESIAN_POINT('Ctrl Pts',(-0.201994298073442,0.0089183090129626,
0.01006364374664));
#40225=CARTESIAN_POINT('Ctrl Pts',(-0.202004853442309,0.00873340615709544,
0.0100903924612634));
#40226=CARTESIAN_POINT('Ctrl Pts',(-0.202010564769062,0.00864432102944395,
0.0101018364537206));
#40227=CARTESIAN_POINT('Ctrl Pts',(-0.202022184353771,0.0084708735187532,
0.0101226862224682));
#40228=CARTESIAN_POINT('Ctrl Pts',(-0.202046363769246,0.00814074718404573,
0.0101549882276266));
#40229=CARTESIAN_POINT('Ctrl Pts',(-0.202075916750842,0.00777532058791057,
0.0101740844248864));
#40230=CARTESIAN_POINT('Ctrl Pts',(-0.202099479627945,0.00749950405175959,
0.0101745804416416));
#40231=CARTESIAN_POINT('',(-0.202180663785047,0.00274072929799762,0.0088597653691895));
#40232=CARTESIAN_POINT('Ctrl Pts',(-0.20209947962974,0.0074995037887144,
0.0101745804416663));
#40233=CARTESIAN_POINT('Ctrl Pts',(-0.202076131298968,0.00722392201477745,
0.0101740593562675));
#40234=CARTESIAN_POINT('Ctrl Pts',(-0.20204684427521,0.00685873434784241,
0.0101549564340284));
#40235=CARTESIAN_POINT('Ctrl Pts',(-0.202022880675394,0.00652881578934848,
0.0101226689516121));
#40236=CARTESIAN_POINT('Ctrl Pts',(-0.202011355028604,0.00635531779374554,
0.010101806581237));
#40237=CARTESIAN_POINT('Ctrl Pts',(-0.202005706364736,0.00626652087781374,
0.0100904032799156));
#40238=CARTESIAN_POINT('Ctrl Pts',(-0.201995177744416,0.00608055260618936,
0.0100634924125636));
#40239=CARTESIAN_POINT('Ctrl Pts',(-0.201985156071195,0.00587249572156429,
0.0100289878141918));
#40240=CARTESIAN_POINT('Ctrl Pts',(-0.201971520984681,0.00550072819479208,
0.00995755927342406));
#40241=CARTESIAN_POINT('Ctrl Pts',(-0.20196544994584,0.00503969878565304,
0.00984581157874883));
#40242=CARTESIAN_POINT('Ctrl Pts',(-0.201980400836738,0.00452026663623846,
0.00968362153215009));
#40243=CARTESIAN_POINT('Ctrl Pts',(-0.202004357630176,0.00414366225519954,
0.00954499266392052));
#40244=CARTESIAN_POINT('Ctrl Pts',(-0.202032546032405,0.00383236089516692,
0.00941725161945248));
#40245=CARTESIAN_POINT('Ctrl Pts',(-0.202053003952958,0.00365417172245642,
0.00933820187402095));
#40246=CARTESIAN_POINT('Ctrl Pts',(-0.202097905643997,0.00329565767648496,
0.00916992114684366));
#40247=CARTESIAN_POINT('Ctrl Pts',(-0.202143715934825,0.00297852659698653,
0.0090014268340662));
#40248=CARTESIAN_POINT('Ctrl Pts',(-0.202180663785047,0.00274072929799762,
0.0088597653691895));
#40249=CARTESIAN_POINT('Ctrl Pts',(-0.202180730245087,0.00274072081434495,
0.00885976172744631));
#40250=CARTESIAN_POINT('Ctrl Pts',(-0.201847614367768,0.002740642783753,
0.00885249354413258));
#40251=CARTESIAN_POINT('Ctrl Pts',(-0.201514127092812,0.00274056060342704,
0.00884521482192548));
#40252=CARTESIAN_POINT('Ctrl Pts',(-0.201180516431429,0.00274047431825838,
0.00883793096370741));
#40253=CARTESIAN_POINT('Origin',(-0.199568033794847,0.00749999923595005,
0.000819344953990154));
#40254=CARTESIAN_POINT('',(-0.1991008326205,0.00749816128270665,0.0101077386020297));
#40255=CARTESIAN_POINT('',(-0.199179696503545,0.00273822610415434,0.00879699955640872));
#40256=CARTESIAN_POINT('Ctrl Pts',(-0.199179696503545,0.00273822610415434,
0.00879699955640872));
#40257=CARTESIAN_POINT('Ctrl Pts',(-0.199143244354989,0.00297491563473041,
0.00893740460207546));
#40258=CARTESIAN_POINT('Ctrl Pts',(-0.199098034288274,0.00329043121711526,
0.00910449277330028));
#40259=CARTESIAN_POINT('Ctrl Pts',(-0.199053629766553,0.00364764361753438,
0.00927172156032095));
#40260=CARTESIAN_POINT('Ctrl Pts',(-0.199033441682036,0.00382433767861057,
0.00934997449065479));
#40261=CARTESIAN_POINT('Ctrl Pts',(-0.199005233009131,0.0041375930335457,
0.00947827794999704));
#40262=CARTESIAN_POINT('Ctrl Pts',(-0.198981402060209,0.00451576736201145,
0.00961718934348785));
#40263=CARTESIAN_POINT('Ctrl Pts',(-0.198966678315752,0.0050396146973732,
0.00978024084154024));
#40264=CARTESIAN_POINT('Ctrl Pts',(-0.198973006624955,0.00549995157901586,
0.00989136011088092));
#40265=CARTESIAN_POINT('Ctrl Pts',(-0.198986778545821,0.00587279695417407,
0.00996274653281332));
#40266=CARTESIAN_POINT('Ctrl Pts',(-0.198996863774921,0.00608136231939041,
0.00999719312649999));
#40267=CARTESIAN_POINT('Ctrl Pts',(-0.199007457649552,0.00626811792143402,
0.0100240914954152));
#40268=CARTESIAN_POINT('Ctrl Pts',(-0.199013083248747,0.00635648831399133,
0.0100353799134243));
#40269=CARTESIAN_POINT('Ctrl Pts',(-0.199024590483033,0.00652977437477116,
0.0100561209067557));
#40270=CARTESIAN_POINT('Ctrl Pts',(-0.199048467492299,0.00685894990481282,
0.0100881861616881));
#40271=CARTESIAN_POINT('Ctrl Pts',(-0.199077613823705,0.00722329121805871,
0.0101071812274239));
#40272=CARTESIAN_POINT('Ctrl Pts',(-0.1991008326205,0.00749816128270665,
0.0101077386020297));
#40273=CARTESIAN_POINT('',(-0.199174846040548,0.0122573379664025,0.00879984889793131));
#40274=CARTESIAN_POINT('Ctrl Pts',(-0.199100423117724,0.00749814796091967,
0.0101077297270977));
#40275=CARTESIAN_POINT('Ctrl Pts',(-0.19909756555931,0.0075305462084152,
0.0101076742637468));
#40276=CARTESIAN_POINT('Ctrl Pts',(-0.199094748669567,0.00756294756525031,
0.0101074502765084));
#40277=CARTESIAN_POINT('Ctrl Pts',(-0.199088680122758,0.00763367215169112,
0.0101065931641555));
#40278=CARTESIAN_POINT('Ctrl Pts',(-0.199085443155413,0.00767199473866375,
0.0101058927930515));
#40279=CARTESIAN_POINT('Ctrl Pts',(-0.199081815402933,0.0077155398050165,
0.0101048285564554));
#40280=CARTESIAN_POINT('Ctrl Pts',(-0.199081381028702,0.00772076361829315,
0.0101046964973235));
#40281=CARTESIAN_POINT('Ctrl Pts',(-0.199080477068572,0.00773165489864521,
0.0101044120095616));
#40282=CARTESIAN_POINT('Ctrl Pts',(-0.199080007626291,0.0077373223541118,
0.0101042588036328));
#40283=CARTESIAN_POINT('Ctrl Pts',(-0.199078414782293,0.00775659033516524,
0.0101037203668784));
#40284=CARTESIAN_POINT('Ctrl Pts',(-0.199077295813301,0.00777019051735651,
0.0101033105458919));
#40285=CARTESIAN_POINT('Ctrl Pts',(-0.199072564471858,0.00782795529984388,
0.010101443394002));
#40286=CARTESIAN_POINT('Ctrl Pts',(-0.199069000449091,0.00787211412832768,
0.0100997019290571));
#40287=CARTESIAN_POINT('Ctrl Pts',(-0.199054876294354,0.00804922540293602,
0.0100914555228068));
#40288=CARTESIAN_POINT('Ctrl Pts',(-0.19904453897387,0.00818240784315175,
0.0100823868562197));
#40289=CARTESIAN_POINT('Ctrl Pts',(-0.199033337016503,0.00833297925678125,
0.0100688913142093));
#40290=CARTESIAN_POINT('Ctrl Pts',(-0.199032001445838,0.00835106298428525,
0.0100672172864517));
#40291=CARTESIAN_POINT('Ctrl Pts',(-0.199023626091707,0.00846542043988094,
0.0100562946091264));
#40292=CARTESIAN_POINT('Ctrl Pts',(-0.199016899990595,0.00856157817146482,
0.0100456013004476));
#40293=CARTESIAN_POINT('Ctrl Pts',(-0.199002448107951,0.00878551065801579,
0.0100171786105707));
#40294=CARTESIAN_POINT('Ctrl Pts',(-0.198995210202229,0.00891256346882149,
0.00999838210039725));
#40295=CARTESIAN_POINT('Ctrl Pts',(-0.19898579937427,0.00910984027578994,
0.00996504196596855));
#40296=CARTESIAN_POINT('Ctrl Pts',(-0.198982810425363,0.00917999713999155,
0.00995236200383042));
#40297=CARTESIAN_POINT('Ctrl Pts',(-0.198977354128857,0.00932718349070731,
0.00992402518089048));
#40298=CARTESIAN_POINT('Ctrl Pts',(-0.198974971381639,0.00940417699397456,
0.00990819783379226));
#40299=CARTESIAN_POINT('Ctrl Pts',(-0.198969144880626,0.00964414837341371,
0.00985572112873346));
#40300=CARTESIAN_POINT('Ctrl Pts',(-0.198967522050789,0.00980638347769885,
0.00981568579315269));
#40301=CARTESIAN_POINT('Ctrl Pts',(-0.198969324601282,0.0100680598402537,
0.00974366898222702));
#40302=CARTESIAN_POINT('Ctrl Pts',(-0.198971089194015,0.0101679091427984,
0.0097143946132173));
#40303=CARTESIAN_POINT('Ctrl Pts',(-0.198978917886141,0.010441256588431,
0.00962930961412696));
#40304=CARTESIAN_POINT('Ctrl Pts',(-0.198987201313106,0.0106134127355314,
0.0095701851250402));
#40305=CARTESIAN_POINT('Ctrl Pts',(-0.199016321440205,0.0110411790868304,
0.00940927412525473));
#40306=CARTESIAN_POINT('Ctrl Pts',(-0.199041597438575,0.0112890619670433,
0.00930344946960165));
#40307=CARTESIAN_POINT('Ctrl Pts',(-0.19907660436805,0.0115666451139836,
0.00917040760605046));
#40308=CARTESIAN_POINT('Ctrl Pts',(-0.199080566717778,0.0115974228045342,
0.00915544770808169));
#40309=CARTESIAN_POINT('Ctrl Pts',(-0.199098466915732,0.0117341340684825,
0.00908806532924535));
#40310=CARTESIAN_POINT('Ctrl Pts',(-0.199113021702264,0.0118396876158331,
0.00903351829961953));
#40311=CARTESIAN_POINT('Ctrl Pts',(-0.199132696289241,0.0119779176994999,
0.0089587005678997));
#40312=CARTESIAN_POINT('Ctrl Pts',(-0.199137603313996,0.0120119720702286,
0.00893999160482358));
#40313=CARTESIAN_POINT('Ctrl Pts',(-0.199145564734414,0.0120665080077619,
0.00890958426378745));
#40314=CARTESIAN_POINT('Ctrl Pts',(-0.19914858987286,0.01208706755771,0.00889801824544057));
#40315=CARTESIAN_POINT('Ctrl Pts',(-0.199155380000627,0.0121328394308257,
0.00887203916099361));
#40316=CARTESIAN_POINT('Ctrl Pts',(-0.199159154233648,0.0121580277333056,
0.00885758650169327));
#40317=CARTESIAN_POINT('Ctrl Pts',(-0.199166705696621,0.0122079000416094,
0.00882865950851265));
#40318=CARTESIAN_POINT('Ctrl Pts',(-0.19917048206159,0.0122325858177661,
0.00881418863909818));
#40319=CARTESIAN_POINT('Ctrl Pts',(-0.199174288103971,0.0122572011081367,
0.00879960620353417));
#40320=CARTESIAN_POINT('',(-0.200176262520899,0.012256855145248,0.0088215241666907));
#40321=CARTESIAN_POINT('Ctrl Pts',(-0.199174569563385,0.0122572006783931,
0.00879961255852584));
#40322=CARTESIAN_POINT('Ctrl Pts',(-0.199508459486052,0.0122570856871889,
0.00880691615277684));
#40323=CARTESIAN_POINT('Ctrl Pts',(-0.199842448484061,0.0122569750175065,
0.0088142193158282));
#40324=CARTESIAN_POINT('Ctrl Pts',(-0.200176327292855,0.012256868740326,
0.00882151747157252));
#40325=CARTESIAN_POINT('',(-0.200100338986871,0.00749890820710971,0.0101293940320589));
#40326=CARTESIAN_POINT('Ctrl Pts',(-0.200176262520899,0.012256855145248,
0.0088215241666907));
#40327=CARTESIAN_POINT('Ctrl Pts',(-0.200139848831246,0.0120187427182138,
0.00896257979280764));
#40328=CARTESIAN_POINT('Ctrl Pts',(-0.200094704254856,0.0117012524516469,
0.0091303434798315));
#40329=CARTESIAN_POINT('Ctrl Pts',(-0.20005045695783,0.0113422735683314,
0.00929792076866446));
#40330=CARTESIAN_POINT('Ctrl Pts',(-0.200030300865821,0.0111639202596685,
0.00937661504422539));
#40331=CARTESIAN_POINT('Ctrl Pts',(-0.200002516361759,0.0108518407830771,
0.00950396043743957));
#40332=CARTESIAN_POINT('Ctrl Pts',(-0.199979012211579,0.0104747794652236,
0.00964195956351153));
#40333=CARTESIAN_POINT('Ctrl Pts',(-0.199964586451688,0.00995464152162186,
0.00980336058488574));
#40334=CARTESIAN_POINT('Ctrl Pts',(-0.199971015201619,0.00949550037894515,
0.00991393870179615));
#40335=CARTESIAN_POINT('Ctrl Pts',(-0.199984854194566,0.0091251855923606,
0.00998471643871501));
#40336=CARTESIAN_POINT('Ctrl Pts',(-0.199994977020821,0.00891797369328077,
0.0100189096450406));
#40337=CARTESIAN_POINT('Ctrl Pts',(-0.20000556647705,0.00873306695781704,
0.0100455533980267));
#40338=CARTESIAN_POINT('Ctrl Pts',(-0.200011293457012,0.00864395082942657,
0.0100569561025451));
#40339=CARTESIAN_POINT('Ctrl Pts',(-0.200022940128602,0.00847046801670082,
0.0100777265959388));
#40340=CARTESIAN_POINT('Ctrl Pts',(-0.200047163314547,0.00814026979588536,
0.0101099034239855));
#40341=CARTESIAN_POINT('Ctrl Pts',(-0.200076753172813,0.00777477572470487,
0.0101289155097155));
#40342=CARTESIAN_POINT('Ctrl Pts',(-0.200100338983303,0.0074989084716685,
0.0101293940320128));
#40343=CARTESIAN_POINT('',(-0.200180004805387,0.00273845846940322,0.00881880778057919));
#40344=CARTESIAN_POINT('Ctrl Pts',(-0.200100338986871,0.00749890820710971,
0.0101293940320589));
#40345=CARTESIAN_POINT('Ctrl Pts',(-0.200077055880268,0.007223317195962,
0.0101288571167368));
#40346=CARTESIAN_POINT('Ctrl Pts',(-0.200047843901506,0.00685811476510037,
0.0101097990374615));
#40347=CARTESIAN_POINT('Ctrl Pts',(-0.200023930105906,0.00652817936751469,
0.0100776062887231));
#40348=CARTESIAN_POINT('Ctrl Pts',(-0.200012422102254,0.006354660368642,
0.0100568059955802));
#40349=CARTESIAN_POINT('Ctrl Pts',(-0.200006781974207,0.0062658760601037,
0.0100454406027125));
#40350=CARTESIAN_POINT('Ctrl Pts',(-0.199996254518662,0.00607981053317545,
0.010018601506999));
#40351=CARTESIAN_POINT('Ctrl Pts',(-0.199986224309984,0.00587169694792907,
0.00998419872280633));
#40352=CARTESIAN_POINT('Ctrl Pts',(-0.199972547223942,0.00549983639015558,
0.009912982695534));
#40353=CARTESIAN_POINT('Ctrl Pts',(-0.199966345220014,0.00503915807743746,
0.00980171648677967));
#40354=CARTESIAN_POINT('Ctrl Pts',(-0.199981045250382,0.00451916422140907,
0.0096399511092111));
#40355=CARTESIAN_POINT('Ctrl Pts',(-0.200004772849193,0.00414244958212928,
0.0095017911578116));
#40356=CARTESIAN_POINT('Ctrl Pts',(-0.200032732117133,0.00383113331162465,
0.00937453733845435));
#40357=CARTESIAN_POINT('Ctrl Pts',(-0.200053059983703,0.00365281023225859,
0.00929574219517862));
#40358=CARTESIAN_POINT('Ctrl Pts',(-0.200097690354166,0.00329403452386807,
0.00912801389820296));
#40359=CARTESIAN_POINT('Ctrl Pts',(-0.200143251201405,0.00297656720641742,
0.00896004372071677));
#40360=CARTESIAN_POINT('Ctrl Pts',(-0.200180004805387,0.00273845846940322,
0.00881880778057919));
#40361=CARTESIAN_POINT('Ctrl Pts',(-0.200180071690563,0.00273844985852019,
0.00881880409310063));
#40362=CARTESIAN_POINT('Ctrl Pts',(-0.199847123138668,0.00273837907375333,
0.00881154922699135));
#40363=CARTESIAN_POINT('Ctrl Pts',(-0.199513602268475,0.00273830396530483,
0.00880427938248978));
#40364=CARTESIAN_POINT('Ctrl Pts',(-0.199179786681636,0.00273822456479632,
0.00879700059164244));
#40365=CARTESIAN_POINT('Origin',(-0.19756813490279,0.0074999991336252,0.000739267166499619));
#40366=CARTESIAN_POINT('',(-0.197101856029946,0.00749734564313153,0.0100625711830282));
#40367=CARTESIAN_POINT('',(-0.197178881546705,0.00273601310122549,0.00875618433461763));
#40368=CARTESIAN_POINT('Ctrl Pts',(-0.197178881546705,0.00273601310122549,
0.00875618433461763));
#40369=CARTESIAN_POINT('Ctrl Pts',(-0.197142626964537,0.00297299673492067,
0.00889614308672296));
#40370=CARTESIAN_POINT('Ctrl Pts',(-0.197097670535042,0.00328882261774284,
0.00906268248965719));
#40371=CARTESIAN_POINT('Ctrl Pts',(-0.197053541172525,0.00364627238000341,
0.00922933666434974));
#40372=CARTESIAN_POINT('Ctrl Pts',(-0.197033485692237,0.00382307290229682,
0.00930731998477126));
#40373=CARTESIAN_POINT('Ctrl Pts',(-0.197005506268391,0.00413636603733711,
0.00943513380611822));
#40374=CARTESIAN_POINT('Ctrl Pts',(-0.196981909916078,0.00451463585616606,
0.00957355710978556));
#40375=CARTESIAN_POINT('Ctrl Pts',(-0.196967449184374,0.00503887642033483,
0.00973612429519158));
#40376=CARTESIAN_POINT('Ctrl Pts',(-0.196973930017077,0.00549897094200798,
0.00984679224998308));
#40377=CARTESIAN_POINT('Ctrl Pts',(-0.196987776644517,0.00587186549873816,
0.00991795678216301));
#40378=CARTESIAN_POINT('Ctrl Pts',(-0.19699789164315,0.00608045844290354,
0.0099522983150153));
#40379=CARTESIAN_POINT('Ctrl Pts',(-0.197008505217262,0.00626727125993394,
0.00997912139989793));
#40380=CARTESIAN_POINT('Ctrl Pts',(-0.197014133781209,0.00635562038557536,
0.00999037271097673));
#40381=CARTESIAN_POINT('Ctrl Pts',(-0.197025646063537,0.00652890076404714,
0.0100110519118934));
#40382=CARTESIAN_POINT('Ctrl Pts',(-0.197049522384861,0.00685808246893175,
0.0100430297163264));
#40383=CARTESIAN_POINT('Ctrl Pts',(-0.197078653753898,0.00722244105207463,
0.0100619906974236));
#40384=CARTESIAN_POINT('Ctrl Pts',(-0.197101856530647,0.00749734560084308,
0.0100625711961792));
#40385=CARTESIAN_POINT('',(-0.197176217067543,0.0122591131058223,0.00875901669782422));
#40386=CARTESIAN_POINT('Ctrl Pts',(-0.19710185655348,0.00749734587138656,
0.0100625711967505));
#40387=CARTESIAN_POINT('Ctrl Pts',(-0.197078523516818,0.00777162104014169,
0.0100621439902365));
#40388=CARTESIAN_POINT('Ctrl Pts',(-0.197049199366131,0.00813529702223795,
0.0100434664523806));
#40389=CARTESIAN_POINT('Ctrl Pts',(-0.197025114401905,0.00846412790914781,
0.0100117657915565));
#40390=CARTESIAN_POINT('Ctrl Pts',(-0.197013477905477,0.00863733646442351,
0.00999122542111019));
#40391=CARTESIAN_POINT('Ctrl Pts',(-0.197007781021792,0.00872568364978063,
0.00998004160952768));
#40392=CARTESIAN_POINT('Ctrl Pts',(-0.196997012427155,0.00891259409020632,
0.00995334571824261));
#40393=CARTESIAN_POINT('Ctrl Pts',(-0.19698672575335,0.00912127329859086,
0.00991914668186268));
#40394=CARTESIAN_POINT('Ctrl Pts',(-0.1969725724387,0.00949430522202776,
0.00984823772706428));
#40395=CARTESIAN_POINT('Ctrl Pts',(-0.196965699496595,0.00995460126870586,
0.0097378606524851));
#40396=CARTESIAN_POINT('Ctrl Pts',(-0.196979759716268,0.010478671284573,
0.00957576289904584));
#40397=CARTESIAN_POINT('Ctrl Pts',(-0.197003135124178,0.0108570185538505,
0.00943763320894697));
#40398=CARTESIAN_POINT('Ctrl Pts',(-0.197030958275967,0.0111703409896189,
0.00931008407709414));
#40399=CARTESIAN_POINT('Ctrl Pts',(-0.197050972536751,0.011347427828458,
0.00923213571472623));
#40400=CARTESIAN_POINT('Ctrl Pts',(-0.197095032095316,0.0117053572034986,
0.00906557221068337));
#40401=CARTESIAN_POINT('Ctrl Pts',(-0.197139967387252,0.0120217156630974,
0.00889902627611354));
#40402=CARTESIAN_POINT('Ctrl Pts',(-0.197176217067543,0.0122591131058223,
0.00875901669782422));
#40403=CARTESIAN_POINT('',(-0.198173992730521,0.0122590030744015,0.00878068750897002));
#40404=CARTESIAN_POINT('Ctrl Pts',(-0.197176307469774,0.012259110245449,
0.00875902035178441));
#40405=CARTESIAN_POINT('Ctrl Pts',(-0.197510848228027,0.0122590743715548,
0.00876628567977086));
#40406=CARTESIAN_POINT('Ctrl Pts',(-0.19784360274998,0.0122590432302266,
0.0087735095219768));
#40407=CARTESIAN_POINT('Ctrl Pts',(-0.198174057214716,0.012259016706353,
0.00878068082077123));
#40408=CARTESIAN_POINT('',(-0.198101353816547,0.00749782534027133,0.0100842108241173));
#40409=CARTESIAN_POINT('Ctrl Pts',(-0.198173992730521,0.0122590030744015,
0.00878068750897002));
#40410=CARTESIAN_POINT('Ctrl Pts',(-0.198138004888705,0.0120204746132674,
0.00892136889022891));
#40411=CARTESIAN_POINT('Ctrl Pts',(-0.198093401335538,0.0117025124533415,
0.00908865958938337));
#40412=CARTESIAN_POINT('Ctrl Pts',(-0.198049719256268,0.0113431216479256,
0.00925572482570341));
#40413=CARTESIAN_POINT('Ctrl Pts',(-0.198029831826993,0.0111645836672768,
0.00933417156341316));
#40414=CARTESIAN_POINT('Ctrl Pts',(-0.198002470389522,0.0108523209073434,
0.00946106760549989));
#40415=CARTESIAN_POINT('Ctrl Pts',(-0.197979387062072,0.0104750174531497,
0.00959859870239481));
#40416=CARTESIAN_POINT('Ctrl Pts',(-0.197965389781622,0.00995446908941076,
0.00975947656779084));
#40417=CARTESIAN_POINT('Ctrl Pts',(-0.197972030645853,0.00949520601411241,
0.00986963753715952));
#40418=CARTESIAN_POINT('Ctrl Pts',(-0.19798596221564,0.00912470398287173,
0.00994016293552026));
#40419=CARTESIAN_POINT('Ctrl Pts',(-0.197996115677719,0.00891738945160544,
0.00997423054978755));
#40420=CARTESIAN_POINT('Ctrl Pts',(-0.198006719249522,0.00873237689330112,
0.0100007756142138));
#40421=CARTESIAN_POINT('Ctrl Pts',(-0.198012445790112,0.00864323678034072,
0.0100121312968828));
#40422=CARTESIAN_POINT('Ctrl Pts',(-0.1980240882512,0.00846968835882415,
0.0100328176107757));
#40423=CARTESIAN_POINT('Ctrl Pts',(-0.198048284245988,0.00813937985693941,
0.0100648555245894));
#40424=CARTESIAN_POINT('Ctrl Pts',(-0.198077819417979,0.00777377379615927,
0.0100837657093142));
#40425=CARTESIAN_POINT('Ctrl Pts',(-0.198101353812703,0.00749782560887336,
0.0100842108240968));
#40426=CARTESIAN_POINT('',(-0.198179277467544,0.00273626767412241,0.00877799114281851));
#40427=CARTESIAN_POINT('Ctrl Pts',(-0.198101353816547,0.00749782534027133,
0.0100842108241173));
#40428=CARTESIAN_POINT('Ctrl Pts',(-0.198078088183822,0.00722225737258161,
0.0100836427809772));
#40429=CARTESIAN_POINT('Ctrl Pts',(-0.198048890875069,0.00685708620871131,
0.0100646149235419));
#40430=CARTESIAN_POINT('Ctrl Pts',(-0.19802497722664,0.00652717554366646,
0.0100325082639782));
#40431=CARTESIAN_POINT('Ctrl Pts',(-0.19801346332886,0.00635366308942737,
0.0100117676259961));
#40432=CARTESIAN_POINT('Ctrl Pts',(-0.198007819566227,0.00626489379443579,
0.0100004373772158));
#40433=CARTESIAN_POINT('Ctrl Pts',(-0.197997274071363,0.00607879754285442,
0.00997367463662727));
#40434=CARTESIAN_POINT('Ctrl Pts',(-0.197987215946941,0.00587067685471771,
0.00993937790394548));
#40435=CARTESIAN_POINT('Ctrl Pts',(-0.197973468852053,0.00549880245195572,
0.00986838680752163));
#40436=CARTESIAN_POINT('Ctrl Pts',(-0.197967122562937,0.00503838759263585,
0.00975757572268468));
#40437=CARTESIAN_POINT('Ctrl Pts',(-0.197981576098232,0.0045180222909139,
0.00959629573797476));
#40438=CARTESIAN_POINT('Ctrl Pts',(-0.198005082771862,0.00414121672263879,
0.00945862266623302));
#40439=CARTESIAN_POINT('Ctrl Pts',(-0.198032826989652,0.00382985614807151,
0.00933185115640346));
#40440=CARTESIAN_POINT('Ctrl Pts',(-0.198053027382874,0.0036514357600232,
0.00925333145484234));
#40441=CARTESIAN_POINT('Ctrl Pts',(-0.198097395119529,0.00329243200436169,
0.00908618421763473));
#40442=CARTESIAN_POINT('Ctrl Pts',(-0.198142713099356,0.00297466421302015,
0.00891877230038998));
#40443=CARTESIAN_POINT('Ctrl Pts',(-0.198179277467544,0.00273626767412241,
0.00877799114281851));
#40444=CARTESIAN_POINT('Ctrl Pts',(-0.19817934460266,0.00273625896376666,
0.0087779874234125));
#40445=CARTESIAN_POINT('Ctrl Pts',(-0.197846274705172,0.00273618093672907,
0.00877073110479899));
#40446=CARTESIAN_POINT('Ctrl Pts',(-0.197512729366218,0.00273609845023171,
0.0087634618445431));
#40447=CARTESIAN_POINT('Ctrl Pts',(-0.197178972113877,0.00273601154455744,
0.00875618537063138));
#40448=CARTESIAN_POINT('Origin',(-0.195568703024637,0.00749999923833712,
0.000658360812067055));
#40449=CARTESIAN_POINT('',(-0.195102854699168,0.00749647351839117,0.0100174036757887));
#40450=CARTESIAN_POINT('',(-0.195178081382383,0.00273409965744036,0.00871564145407736));
#40451=CARTESIAN_POINT('Ctrl Pts',(-0.195178081382383,0.00273409965744036,
0.00871564145407736));
#40452=CARTESIAN_POINT('Ctrl Pts',(-0.195142003031606,0.00297137204920274,
0.00885512670497663));
#40453=CARTESIAN_POINT('Ctrl Pts',(-0.195097271567982,0.00328749493151492,
0.00902108304563917));
#40454=CARTESIAN_POINT('Ctrl Pts',(-0.195053379669963,0.00364518457110896,
0.00918713546639911));
#40455=CARTESIAN_POINT('Ctrl Pts',(-0.195033441180626,0.00382205047526963,
0.00926481961242654));
#40456=CARTESIAN_POINT('Ctrl Pts',(-0.195005638551936,0.00413551272222303,
0.009392175608848));
#40457=CARTESIAN_POINT('Ctrl Pts',(-0.194982225913951,0.00451392049931529,
0.00953009104539298));
#40458=CARTESIAN_POINT('Ctrl Pts',(-0.194967960467318,0.00503823275189329,
0.00969205034835313));
#40459=CARTESIAN_POINT('Ctrl Pts',(-0.194974562672158,0.00549844324011582,
0.00980233354848123));
#40460=CARTESIAN_POINT('Ctrl Pts',(-0.194988493479225,0.00587128826194149,
0.00987323309250545));
#40461=CARTESIAN_POINT('Ctrl Pts',(-0.194998650748219,0.00607983838954741,
0.0099074486869859));
#40462=CARTESIAN_POINT('Ctrl Pts',(-0.195009298503175,0.00626658803704918,
0.0099341733993258));
#40463=CARTESIAN_POINT('Ctrl Pts',(-0.195014943861307,0.00635493196350272,
0.00994538806277399));
#40464=CARTESIAN_POINT('Ctrl Pts',(-0.195026487338825,0.00652818220539433,
0.00996599834821625));
#40465=CARTESIAN_POINT('Ctrl Pts',(-0.195050420612355,0.00685731380746718,
0.0099978773710621));
#40466=CARTESIAN_POINT('Ctrl Pts',(-0.195079610558799,0.00722161145123598,
0.0100167973575665));
#40467=CARTESIAN_POINT('Ctrl Pts',(-0.195102855210816,0.00749647347509058,
0.0100174036899749));
#40468=CARTESIAN_POINT('',(-0.19517793622571,0.0122618594502722,0.00871802364175171));
#40469=CARTESIAN_POINT('Ctrl Pts',(-0.195102855229775,0.00749647369925886,
0.0100174036904694));
#40470=CARTESIAN_POINT('Ctrl Pts',(-0.195079650033701,0.0077708960107351,
0.0100170049335787));
#40471=CARTESIAN_POINT('Ctrl Pts',(-0.195050492730399,0.00813475203583469,
0.00999841538572308));
#40472=CARTESIAN_POINT('Ctrl Pts',(-0.195026555120156,0.00846373126034199,
0.0099668392959626));
#40473=CARTESIAN_POINT('Ctrl Pts',(-0.195014995306788,0.00863700065608847,
0.00994637890650517));
#40474=CARTESIAN_POINT('Ctrl Pts',(-0.195009336160461,0.00872539617663902,
0.00993523552157287));
#40475=CARTESIAN_POINT('Ctrl Pts',(-0.194998651227084,0.00891229649891521,
0.00990865196002218));
#40476=CARTESIAN_POINT('Ctrl Pts',(-0.194988450243687,0.0091210211909995,
0.00987458746983198));
#40477=CARTESIAN_POINT('Ctrl Pts',(-0.194974434565974,0.00949420365260338,
0.00980394105343129));
#40478=CARTESIAN_POINT('Ctrl Pts',(-0.194967699416777,0.00995492489130331,
0.0096939165698559));
#40479=CARTESIAN_POINT('Ctrl Pts',(-0.19498181283275,0.0104798102273614,
0.0095321912702417));
#40480=CARTESIAN_POINT('Ctrl Pts',(-0.195005149570046,0.0108583756108732,
0.00939450978445774));
#40481=CARTESIAN_POINT('Ctrl Pts',(-0.195032878840536,0.0111716458058373,
0.00926749369434052));
#40482=CARTESIAN_POINT('Ctrl Pts',(-0.195052857418986,0.0113489620203353,
0.00918976770636426));
#40483=CARTESIAN_POINT('Ctrl Pts',(-0.195096844479162,0.01170725645881,
0.00902372410857468));
#40484=CARTESIAN_POINT('Ctrl Pts',(-0.195141725801382,0.0120240670219162,
0.00885765266532079));
#40485=CARTESIAN_POINT('Ctrl Pts',(-0.19517793622571,0.0122618594502722,
0.00871802364175171));
#40486=CARTESIAN_POINT('',(-0.19617749360186,0.0122611495956684,0.00874007044956493));
#40487=CARTESIAN_POINT('Ctrl Pts',(-0.195178027888241,0.0122618562493937,
0.00871802751514387));
#40488=CARTESIAN_POINT('Ctrl Pts',(-0.195511176940293,0.0122616207531416,
0.0087253750077405));
#40489=CARTESIAN_POINT('Ctrl Pts',(-0.195844424120966,0.01226138980123,
0.00873272192611785));
#40490=CARTESIAN_POINT('Ctrl Pts',(-0.196177561574348,0.0122611635394136,
0.00874006368840159));
#40491=CARTESIAN_POINT('',(-0.19610247501614,0.00749683809102515,0.0100390300519628));
#40492=CARTESIAN_POINT('Ctrl Pts',(-0.19617749360186,0.0122611495956684,
0.00874007044956493));
#40493=CARTESIAN_POINT('Ctrl Pts',(-0.196141014853573,0.0120222633487051,
0.00888031100537719));
#40494=CARTESIAN_POINT('Ctrl Pts',(-0.19609580872818,0.0117038769497799,
0.00904706732867685));
#40495=CARTESIAN_POINT('Ctrl Pts',(-0.196051579746205,0.011344201623836,
0.00921353755448672));
#40496=CARTESIAN_POINT('Ctrl Pts',(-0.196031434794024,0.0111652973544448,
0.00929179681903197));
#40497=CARTESIAN_POINT('Ctrl Pts',(-0.196003872188682,0.0108536221626497,
0.00941792065964247));
#40498=CARTESIAN_POINT('Ctrl Pts',(-0.195980602663577,0.0104763472727013,
0.00955493379103075));
#40499=CARTESIAN_POINT('Ctrl Pts',(-0.195966554994754,0.00995393571634196,
0.00971572130618377));
#40500=CARTESIAN_POINT('Ctrl Pts',(-0.195973267353857,0.00949586692018786,
0.00982513937332992));
#40501=CARTESIAN_POINT('Ctrl Pts',(-0.195987224807208,0.00912487364769354,
0.00989550872314588));
#40502=CARTESIAN_POINT('Ctrl Pts',(-0.195997392390853,0.00891725362595259,
0.00992949377263191));
#40503=CARTESIAN_POINT('Ctrl Pts',(-0.196008014235276,0.00873175598500685,
0.00995599726309419));
#40504=CARTESIAN_POINT('Ctrl Pts',(-0.196013728479012,0.00864268846028022,
0.00996729220581992));
#40505=CARTESIAN_POINT('Ctrl Pts',(-0.196025358475374,0.00846903577183134,
0.009987901148687));
#40506=CARTESIAN_POINT('Ctrl Pts',(-0.196049514119745,0.00813862434607263,
0.0100198011636422));
#40507=CARTESIAN_POINT('Ctrl Pts',(-0.196078991315259,0.00777288071169348,
0.0100386152787338));
#40508=CARTESIAN_POINT('Ctrl Pts',(-0.19610247501614,0.00749683809102515,
0.0100390300519628));
#40509=CARTESIAN_POINT('',(-0.196178471694746,0.00273416910722515,0.00873732259680264));
#40510=CARTESIAN_POINT('Ctrl Pts',(-0.196102475015075,0.00749683779606065,
0.01003903005184));
#40511=CARTESIAN_POINT('Ctrl Pts',(-0.196079179883013,0.00722129154127866,
0.0100384329494739));
#40512=CARTESIAN_POINT('Ctrl Pts',(-0.196049938683409,0.00685615343993873,
0.010019439305117));
#40513=CARTESIAN_POINT('Ctrl Pts',(-0.196025978348201,0.00652626866424729,
0.00998742334664808));
#40514=CARTESIAN_POINT('Ctrl Pts',(-0.19601443718888,0.00635277195028409,
0.00996674647638142));
#40515=CARTESIAN_POINT('Ctrl Pts',(-0.196008778514743,0.00626400469010116,
0.00995545091588954));
#40516=CARTESIAN_POINT('Ctrl Pts',(-0.195998200063883,0.0060779436700094,
0.00992877795260165));
#40517=CARTESIAN_POINT('Ctrl Pts',(-0.195988099405926,0.00586985213365078,
0.00989459928016789));
#40518=CARTESIAN_POINT('Ctrl Pts',(-0.195974263559204,0.00549801481097926,
0.0098238581958861));
#40519=CARTESIAN_POINT('Ctrl Pts',(-0.195967774730541,0.00503764505177799,
0.00971346212967491));
#40520=CARTESIAN_POINT('Ctrl Pts',(-0.195982000966316,0.00451710683680645,
0.0095527459791788));
#40521=CARTESIAN_POINT('Ctrl Pts',(-0.19600530088904,0.00414017154598768,
0.00941556906216487));
#40522=CARTESIAN_POINT('Ctrl Pts',(-0.196032847971522,0.00382866522289246,
0.00928925272084666));
#40523=CARTESIAN_POINT('Ctrl Pts',(-0.19605292051857,0.00365017065488466,
0.0092110260323459));
#40524=CARTESIAN_POINT('Ctrl Pts',(-0.196097027755299,0.00329092584867731,
0.00904447216382486));
#40525=CARTESIAN_POINT('Ctrl Pts',(-0.196142099821149,0.00297285698814056,
0.00887763569320788));
#40526=CARTESIAN_POINT('Ctrl Pts',(-0.196178471694746,0.00273416910722515,
0.00873732259680264));
#40527=CARTESIAN_POINT('Ctrl Pts',(-0.196178538776777,0.00273416018332472,
0.0087373187725441));
#40528=CARTESIAN_POINT('Ctrl Pts',(-0.195848366636187,0.00273414417116084,
0.00873016714070241));
#40529=CARTESIAN_POINT('Ctrl Pts',(-0.195514684660614,0.00273412355097259,
0.00872293686128152));
#40530=CARTESIAN_POINT('Ctrl Pts',(-0.195178171724056,0.00273409810905456,
0.00871564249297404));
#40531=CARTESIAN_POINT('Origin',(-0.221676747656307,0.00749999656668326,
0.0016542281911168));
#40532=CARTESIAN_POINT('',(-0.221093368579246,0.00749707905428301,0.0106049493394889));
#40533=CARTESIAN_POINT('',(-0.221393324273061,0.00186012453844665,0.0086135531677188));
#40534=CARTESIAN_POINT('Ctrl Pts',(-0.221393324273061,0.00186012453844665,
0.0086135531677188));
#40535=CARTESIAN_POINT('Ctrl Pts',(-0.221320882289907,0.00211836443593635,
0.00882119182016569));
#40536=CARTESIAN_POINT('Ctrl Pts',(-0.221231403465256,0.00247125386688205,
0.00907118054582986));
#40537=CARTESIAN_POINT('Ctrl Pts',(-0.221145920712544,0.00287451696712188,
0.0093214834214468));
#40538=CARTESIAN_POINT('Ctrl Pts',(-0.221106573265363,0.00308812820272732,
0.00944560427206486));
#40539=CARTESIAN_POINT('Ctrl Pts',(-0.221059991603806,0.00341486099713401,
0.0096217897422861));
#40540=CARTESIAN_POINT('Ctrl Pts',(-0.221025097040765,0.00374441410818285,
0.00978109693071447));
#40541=CARTESIAN_POINT('Ctrl Pts',(-0.220997020866922,0.00410243999479013,
0.00993723070964949));
#40542=CARTESIAN_POINT('Ctrl Pts',(-0.220969869674211,0.00463263526782197,
0.0101388265080547));
#40543=CARTESIAN_POINT('Ctrl Pts',(-0.220961461135514,0.0051065827707716,
0.0102830013236984));
#40544=CARTESIAN_POINT('Ctrl Pts',(-0.22096742412538,0.00554565041247079,
0.0103879784709596));
#40545=CARTESIAN_POINT('Ctrl Pts',(-0.22097446939084,0.00578597401251634,
0.0104377123773018));
#40546=CARTESIAN_POINT('Ctrl Pts',(-0.22098293893607,0.00599041622708282,
0.0104749903919));
#40547=CARTESIAN_POINT('Ctrl Pts',(-0.220988776572196,0.00610221416093042,
0.0104932684418798));
#40548=CARTESIAN_POINT('Ctrl Pts',(-0.221000797352358,0.00631019098849533,
0.0105248268975094));
#40549=CARTESIAN_POINT('Ctrl Pts',(-0.221028058933879,0.00671202962450896,
0.0105746498724072));
#40550=CARTESIAN_POINT('Ctrl Pts',(-0.221063870013657,0.00715868680504821,
0.0106042063475681));
#40551=CARTESIAN_POINT('Ctrl Pts',(-0.221093368579246,0.00749707905428301,
0.0106049493394889));
#40552=CARTESIAN_POINT('',(-0.22139901452729,0.0131263848813722,0.0086245734578183));
#40553=CARTESIAN_POINT('Ctrl Pts',(-0.221093368511532,0.00749707983574417,
0.0106049493382898));
#40554=CARTESIAN_POINT('Ctrl Pts',(-0.221064138632359,0.00783440526382265,
0.0106044317127623));
#40555=CARTESIAN_POINT('Ctrl Pts',(-0.221028690283817,0.00827968401694266,
0.0105753564148156));
#40556=CARTESIAN_POINT('Ctrl Pts',(-0.221001771034026,0.00868043883058296,
0.0105260869185151));
#40557=CARTESIAN_POINT('Ctrl Pts',(-0.220989940522154,0.00888778115969991,
0.0104948644318784));
#40558=CARTESIAN_POINT('Ctrl Pts',(-0.220984195526036,0.00899953416961957,
0.0104767199871332));
#40559=CARTESIAN_POINT('Ctrl Pts',(-0.220975962958393,0.00920256216542126,
0.0104399565249176));
#40560=CARTESIAN_POINT('Ctrl Pts',(-0.220969173569176,0.00944187368631053,
0.010390779029624));
#40561=CARTESIAN_POINT('Ctrl Pts',(-0.220963664948118,0.00987968825111028,
0.0102868015301267));
#40562=CARTESIAN_POINT('Ctrl Pts',(-0.220972537969122,0.0103543468070456,
0.0101433091098129));
#40563=CARTESIAN_POINT('Ctrl Pts',(-0.22100014605577,0.0108863043563923,
0.00994189923874667));
#40564=CARTESIAN_POINT('Ctrl Pts',(-0.221028400357267,0.0112443083842731,
0.0097863495839049));
#40565=CARTESIAN_POINT('Ctrl Pts',(-0.221063406650245,0.011573393629629,
0.00962781935203964));
#40566=CARTESIAN_POINT('Ctrl Pts',(-0.221109786986603,0.0118977656332968,
0.00945360557205793));
#40567=CARTESIAN_POINT('Ctrl Pts',(-0.221149495808629,0.0121123070321511,
0.00932948385688051));
#40568=CARTESIAN_POINT('Ctrl Pts',(-0.221235610859116,0.012515396777809,
0.00908025727666793));
#40569=CARTESIAN_POINT('Ctrl Pts',(-0.221325901145816,0.0128682488917034,
0.00883128630788534));
#40570=CARTESIAN_POINT('Ctrl Pts',(-0.22139901452729,0.0131263848813722,
0.0086245734578183));
#40571=CARTESIAN_POINT('',(-0.222398584008074,0.0131269370004452,0.00864558885643978));
#40572=CARTESIAN_POINT('Ctrl Pts',(-0.221399005354199,0.0131263862088147,
0.00862457218979462));
#40573=CARTESIAN_POINT('Ctrl Pts',(-0.22173218058233,0.0131265693374647,
0.00863157775568907));
#40574=CARTESIAN_POINT('Ctrl Pts',(-0.222065430958852,0.0131267587198589,
0.00863857987776453));
#40575=CARTESIAN_POINT('Ctrl Pts',(-0.222398552886268,0.0131269542394213,
0.00864557427637836));
#40576=CARTESIAN_POINT('',(-0.222093143437656,0.00749648534996505,0.0106264030851718));
#40577=CARTESIAN_POINT('Ctrl Pts',(-0.222398584008074,0.0131269370004452,
0.00864558885643978));
#40578=CARTESIAN_POINT('Ctrl Pts',(-0.222325641082348,0.0128695208609679,
0.00885175731756058));
#40579=CARTESIAN_POINT('Ctrl Pts',(-0.222235540235227,0.0125176000581379,
0.00910020560792411));
#40580=CARTESIAN_POINT('Ctrl Pts',(-0.222149564294992,0.0121153707119367,
0.00934910793309511));
#40581=CARTESIAN_POINT('Ctrl Pts',(-0.222109873160673,0.0119010991654769,
0.00947318891730329));
#40582=CARTESIAN_POINT('Ctrl Pts',(-0.222063547308976,0.0115772555261176,
0.00964731674420564));
#40583=CARTESIAN_POINT('Ctrl Pts',(-0.222028542068434,0.0112478469047188,
0.00980619275617348));
#40584=CARTESIAN_POINT('Ctrl Pts',(-0.222000270545164,0.0108892810765668,
0.0099621912896326));
#40585=CARTESIAN_POINT('Ctrl Pts',(-0.221972560495376,0.01035418756447,
0.0101648683784779));
#40586=CARTESIAN_POINT('Ctrl Pts',(-0.22196374637383,0.00988361918379579,
0.0103070820085407));
#40587=CARTESIAN_POINT('Ctrl Pts',(-0.22196900595078,0.00944781271840059,
0.0104109088339609));
#40588=CARTESIAN_POINT('Ctrl Pts',(-0.221975632337354,0.00920971477057703,
0.0104600109800392));
#40589=CARTESIAN_POINT('Ctrl Pts',(-0.221983661532872,0.00900833042423417,
0.0104966686439572));
#40590=CARTESIAN_POINT('Ctrl Pts',(-0.221989384785992,0.00889557040884757,
0.0105150945176128));
#40591=CARTESIAN_POINT('Ctrl Pts',(-0.222001164804074,0.00868751157232488,
0.0105465995258684));
#40592=CARTESIAN_POINT('Ctrl Pts',(-0.222028109563492,0.00828446961210274,
0.0105964575047171));
#40593=CARTESIAN_POINT('Ctrl Pts',(-0.22206372594124,0.00783626729013152,
0.0106259053127712));
#40594=CARTESIAN_POINT('Ctrl Pts',(-0.222093143437656,0.00749648534996505,
0.0106264030851718));
#40595=CARTESIAN_POINT('',(-0.222392855892362,0.00185977364761083,0.00863470624003947));
#40596=CARTESIAN_POINT('Ctrl Pts',(-0.222093143598432,0.0074964834929572,
0.0106264030878921));
#40597=CARTESIAN_POINT('Ctrl Pts',(-0.22206375015713,0.00715897485979281,
0.0106256396722468));
#40598=CARTESIAN_POINT('Ctrl Pts',(-0.222028050253872,0.00671348063535476,
0.010596200751429));
#40599=CARTESIAN_POINT('Ctrl Pts',(-0.222000846841533,0.00631280356028926,
0.0105466293505842));
#40600=CARTESIAN_POINT('Ctrl Pts',(-0.221988831912577,0.00610531304827131,
0.0105152119148758));
#40601=CARTESIAN_POINT('Ctrl Pts',(-0.22198300522171,0.00599413078537288,
0.0104970825394779));
#40602=CARTESIAN_POINT('Ctrl Pts',(-0.221974470768666,0.00578916799523837,
0.0104597946922141));
#40603=CARTESIAN_POINT('Ctrl Pts',(-0.221967372630738,0.00554854776043954,
0.0104100791661046));
#40604=CARTESIAN_POINT('Ctrl Pts',(-0.221961300260906,0.00510911991771959,
0.0103051978930735));
#40605=CARTESIAN_POINT('Ctrl Pts',(-0.221969719400783,0.00463309356998036,
0.0101603737211353));
#40606=CARTESIAN_POINT('Ctrl Pts',(-0.221996612877404,0.00410625701407935,
0.0099601894605402));
#40607=CARTESIAN_POINT('Ctrl Pts',(-0.222024427583076,0.00374960296769934,
0.00980491605246754));
#40608=CARTESIAN_POINT('Ctrl Pts',(-0.222059048888332,0.00342099857771816,
0.00964632710519627));
#40609=CARTESIAN_POINT('Ctrl Pts',(-0.22210506112296,0.00309585054480878,
0.00947138795878032));
#40610=CARTESIAN_POINT('Ctrl Pts',(-0.222144630451831,0.0028796076224462,
0.00934600847256188));
#40611=CARTESIAN_POINT('Ctrl Pts',(-0.222230300116289,0.00247416995600222,
0.00909464993907419));
#40612=CARTESIAN_POINT('Ctrl Pts',(-0.222320125851231,0.00211925508531268,
0.00884336697495338));
#40613=CARTESIAN_POINT('Ctrl Pts',(-0.222392855892362,0.00185977364761083,
0.00863470624003947));
#40614=CARTESIAN_POINT('Ctrl Pts',(-0.22239282131095,0.00185976173076948,
0.00863469584383406));
#40615=CARTESIAN_POINT('Ctrl Pts',(-0.222059512049327,0.00185988814640051,
0.00862764965075787));
#40616=CARTESIAN_POINT('Ctrl Pts',(-0.221726263388519,0.00186000852650555,
0.0086205998615492));
#40617=CARTESIAN_POINT('Ctrl Pts',(-0.221393313500158,0.00186012280700108,
0.00861355153407611));
#40618=CARTESIAN_POINT('Origin',(-0.21967833919211,0.00750000224638511,
0.0015821781795227));
#40619=CARTESIAN_POINT('',(-0.219093931424061,0.00749805713493659,0.0105597809184262));
#40620=CARTESIAN_POINT('',(-0.219329675491582,0.00207001641050771,0.00873878981654981));
#40621=CARTESIAN_POINT('Ctrl Pts',(-0.219329675491582,0.00207001641050771,
0.0087387898165498));
#40622=CARTESIAN_POINT('Ctrl Pts',(-0.21926673218781,0.00232397546437185,
0.00893001603366529));
#40623=CARTESIAN_POINT('Ctrl Pts',(-0.21918910173417,0.00266911277428291,
0.0091597253869842));
#40624=CARTESIAN_POINT('Ctrl Pts',(-0.219115197421065,0.00306172087601469,
0.00938926825850818));
#40625=CARTESIAN_POINT('Ctrl Pts',(-0.219081341420747,0.00326851581087775,
0.00950267558687953));
#40626=CARTESIAN_POINT('Ctrl Pts',(-0.219041428682301,0.00358655944730087,
0.00966440155326771));
#40627=CARTESIAN_POINT('Ctrl Pts',(-0.219002234332528,0.00400670339074093,
0.00985725686767314));
#40628=CARTESIAN_POINT('Ctrl Pts',(-0.218968686763695,0.0046367188189223,
0.0101006623712429));
#40629=CARTESIAN_POINT('Ctrl Pts',(-0.218962333710723,0.00521465726012983,
0.0102673885531289));
#40630=CARTESIAN_POINT('Ctrl Pts',(-0.218970025383219,0.00563368217517905,
0.0103625206402003));
#40631=CARTESIAN_POINT('Ctrl Pts',(-0.21897762636222,0.00586348838946524,
0.0104077368567593));
#40632=CARTESIAN_POINT('Ctrl Pts',(-0.218986309443235,0.00605854847551105,
0.0104415635341072));
#40633=CARTESIAN_POINT('Ctrl Pts',(-0.218992164333208,0.00616555763761863,
0.0104582113469295));
#40634=CARTESIAN_POINT('Ctrl Pts',(-0.219004098923365,0.00636432765538068,
0.010486908383612));
#40635=CARTESIAN_POINT('Ctrl Pts',(-0.219030818498434,0.00674834748173606,
0.0105322256424722));
#40636=CARTESIAN_POINT('Ctrl Pts',(-0.219065504441556,0.00717490747545383,
0.010559101519801));
#40637=CARTESIAN_POINT('Ctrl Pts',(-0.219093931424061,0.00749805713493659,
0.0105597809184262));
#40638=CARTESIAN_POINT('',(-0.219334449421015,0.0129184051342887,0.00874766341044521));
#40639=CARTESIAN_POINT('Ctrl Pts',(-0.219093931309954,0.00749805843864198,
0.0105597809162631));
#40640=CARTESIAN_POINT('Ctrl Pts',(-0.219065711408738,0.00782047596527625,
0.010559245912387));
#40641=CARTESIAN_POINT('Ctrl Pts',(-0.219031316520399,0.00824607622127998,
0.0105326831954569));
#40642=CARTESIAN_POINT('Ctrl Pts',(-0.219004889515743,0.00862937329987748,
0.010487720905152));
#40643=CARTESIAN_POINT('Ctrl Pts',(-0.218993127081861,0.00882766146147039,
0.0104592502874459));
#40644=CARTESIAN_POINT('Ctrl Pts',(-0.218987354155981,0.00893476683096917,
0.0104426666457267));
#40645=CARTESIAN_POINT('Ctrl Pts',(-0.218978909341311,0.00912836382219906,
0.0104092624073532));
#40646=CARTESIAN_POINT('Ctrl Pts',(-0.218971559602137,0.00935720765481112,
0.0103644753266291));
#40647=CARTESIAN_POINT('Ctrl Pts',(-0.218964305057173,0.00977503223623715,
0.0102701201291484));
#40648=CARTESIAN_POINT('Ctrl Pts',(-0.218971244168002,0.0103548699408352,
0.0101036237942178));
#40649=CARTESIAN_POINT('Ctrl Pts',(-0.219005168265794,0.0109862554488166,
0.0098602839683849));
#40650=CARTESIAN_POINT('Ctrl Pts',(-0.219044409430049,0.0114052096208588,
0.00966840150914399));
#40651=CARTESIAN_POINT('Ctrl Pts',(-0.219084036732671,0.0117202529412656,
0.00950870094055952));
#40652=CARTESIAN_POINT('Ctrl Pts',(-0.219118190408138,0.0119278693536131,
0.00939524877450844));
#40653=CARTESIAN_POINT('Ctrl Pts',(-0.21919260264818,0.0123199329036179,
0.00916673739389008));
#40654=CARTESIAN_POINT('Ctrl Pts',(-0.219270925812016,0.0126647568293119,
0.0089379970943531));
#40655=CARTESIAN_POINT('Ctrl Pts',(-0.219334449421015,0.0129184051342887,
0.00874766341044521));
#40656=CARTESIAN_POINT('',(-0.220398875414435,0.013127345180933,0.00860767229782415));
#40657=CARTESIAN_POINT('Ctrl Pts',(-0.2193344482324,0.0129185235189919,
0.00874777258268191));
#40658=CARTESIAN_POINT('Ctrl Pts',(-0.219446892856324,0.0129669566534953,
0.00871338003143611));
#40659=CARTESIAN_POINT('Ctrl Pts',(-0.219543061237216,0.0130071173503667,
0.00868434426531221));
#40660=CARTESIAN_POINT('Ctrl Pts',(-0.21962977665937,0.0130390459589621,
0.00866119629744851));
#40661=CARTESIAN_POINT('Ctrl Pts',(-0.219673135892507,0.0130550108236821,
0.00864962190721527));
#40662=CARTESIAN_POINT('Ctrl Pts',(-0.219714134616583,0.0130688951516554,
0.00863954132345271));
#40663=CARTESIAN_POINT('Ctrl Pts',(-0.219746959307074,0.0130792506280983,
0.00863205556330531));
#40664=CARTESIAN_POINT('Ctrl Pts',(-0.219779783997565,0.0130896061045412,
0.00862456980315791));
#40665=CARTESIAN_POINT('Ctrl Pts',(-0.219804185483759,0.0130968868605942,
0.00861931110782013));
#40666=CARTESIAN_POINT('Ctrl Pts',(-0.219843260685388,0.0131070498458526,
0.00861201982549279));
#40667=CARTESIAN_POINT('Ctrl Pts',(-0.219855710948212,0.0131102880079675,
0.00860969665433781));
#40668=CARTESIAN_POINT('Ctrl Pts',(-0.219869697085274,0.0131137784499516,
0.00860720288149674));
#40669=CARTESIAN_POINT('Ctrl Pts',(-0.219884547633558,0.0131172460352354,
0.00860474250115293));
#40670=CARTESIAN_POINT('Ctrl Pts',(-0.219916305592798,0.0131246614807796,
0.00859948096755987));
#40671=CARTESIAN_POINT('Ctrl Pts',(-0.219952020187925,0.013131841676374,
0.00859447424251011));
#40672=CARTESIAN_POINT('Ctrl Pts',(-0.219985174108256,0.0131371095774531,
0.00859094902561431));
#40673=CARTESIAN_POINT('Ctrl Pts',(-0.220033831351422,0.0131448408364181,
0.00858577535885028));
#40674=CARTESIAN_POINT('Ctrl Pts',(-0.220076741916514,0.0131489240309038,
0.00858338293662867));
#40675=CARTESIAN_POINT('Ctrl Pts',(-0.220118876196711,0.0131505486997066,
0.00858296642564705));
#40676=CARTESIAN_POINT('Ctrl Pts',(-0.220141481026886,0.0131514203263775,
0.00858274296959271));
#40677=CARTESIAN_POINT('Ctrl Pts',(-0.220163923963669,0.0131515501294491,
0.00858311495808394));
#40678=CARTESIAN_POINT('Ctrl Pts',(-0.220186832211857,0.013150858495987,
0.00858416347060276));
#40679=CARTESIAN_POINT('Ctrl Pts',(-0.220249322385183,0.0131489718264098,
0.00858702365128946));
#40680=CARTESIAN_POINT('Ctrl Pts',(-0.22031494630866,0.0131409425340114,
0.00859494515751143));
#40681=CARTESIAN_POINT('Ctrl Pts',(-0.220398951901741,0.0131276350205432,
0.00860743104837679));
#40682=CARTESIAN_POINT('',(-0.220093673496084,0.00749758231473663,0.0105812097663496));
#40683=CARTESIAN_POINT('Ctrl Pts',(-0.220398875414435,0.013127345180933,
0.00860767229782415));
#40684=CARTESIAN_POINT('Ctrl Pts',(-0.220325934104189,0.0128696007310759,
0.00881311000494965));
#40685=CARTESIAN_POINT('Ctrl Pts',(-0.220235832151988,0.012517380154814,
0.00906064802695024));
#40686=CARTESIAN_POINT('Ctrl Pts',(-0.22014983518567,0.0121148742622212,
0.00930865312239604));
#40687=CARTESIAN_POINT('Ctrl Pts',(-0.220110148563968,0.0119006189294791,
0.00943221399864835));
#40688=CARTESIAN_POINT('Ctrl Pts',(-0.220063730000698,0.0115762317761984,
0.00960591985594359));
#40689=CARTESIAN_POINT('Ctrl Pts',(-0.220028700288234,0.011246729617028,
0.0097641926164711));
#40690=CARTESIAN_POINT('Ctrl Pts',(-0.220000425693391,0.0108882511595183,
0.00991953869054433));
#40691=CARTESIAN_POINT('Ctrl Pts',(-0.21997276242715,0.0103537426143642,
0.0101212364943754));
#40692=CARTESIAN_POINT('Ctrl Pts',(-0.219964019306003,0.00988381931694247,
0.0102628033818167));
#40693=CARTESIAN_POINT('Ctrl Pts',(-0.219969349684687,0.00944806796185167,
0.010366308027579));
#40694=CARTESIAN_POINT('Ctrl Pts',(-0.219976017534628,0.00920993945947005,
0.0104152726707589));
#40695=CARTESIAN_POINT('Ctrl Pts',(-0.219984088108219,0.00900837540122992,
0.0104518536356056));
#40696=CARTESIAN_POINT('Ctrl Pts',(-0.219989822314319,0.00889575753165797,
0.0104702005507611));
#40697=CARTESIAN_POINT('Ctrl Pts',(-0.220001626212636,0.00868779787530209,
0.0105016013492101));
#40698=CARTESIAN_POINT('Ctrl Pts',(-0.220028604724524,0.00828502755883445,
0.0105512922085914));
#40699=CARTESIAN_POINT('Ctrl Pts',(-0.220064244947719,0.00783712777332673,
0.0105806702055769));
#40700=CARTESIAN_POINT('Ctrl Pts',(-0.220093673496084,0.00749758231473663,
0.0105812097663496));
#40701=CARTESIAN_POINT('',(-0.220393469212935,0.00185932807944966,0.00859684197992795));
#40702=CARTESIAN_POINT('Ctrl Pts',(-0.220093673613352,0.00749758096170686,
0.0105812097684996));
#40703=CARTESIAN_POINT('Ctrl Pts',(-0.220064263129577,0.00716015337126071,
0.0105804886629416));
#40704=CARTESIAN_POINT('Ctrl Pts',(-0.220028538804154,0.00671475847876594,
0.010551204008513));
#40705=CARTESIAN_POINT('Ctrl Pts',(-0.220001313267265,0.00631415782065367,
0.0105018520462385));
#40706=CARTESIAN_POINT('Ctrl Pts',(-0.219989286579143,0.00610669204075673,
0.0104705664657165));
#40707=CARTESIAN_POINT('Ctrl Pts',(-0.219983455094469,0.00599554664686926,
0.0104525162872843));
#40708=CARTESIAN_POINT('Ctrl Pts',(-0.219974905590976,0.00579052816249508,
0.0104153681588899));
#40709=CARTESIAN_POINT('Ctrl Pts',(-0.219967795508928,0.00554977942667081,
0.0103658112243735));
#40710=CARTESIAN_POINT('Ctrl Pts',(-0.219961695456283,0.00511134405379829,
0.0102616067514142));
#40711=CARTESIAN_POINT('Ctrl Pts',(-0.219972297213109,0.00450814141055009,
0.0100789890536557));
#40712=CARTESIAN_POINT('Ctrl Pts',(-0.22001334899915,0.00385700754459336,
0.0098147555328663));
#40713=CARTESIAN_POINT('Ctrl Pts',(-0.220059518713161,0.00342300351096295,
0.00960528627718777));
#40714=CARTESIAN_POINT('Ctrl Pts',(-0.220105621826452,0.00309650561112459,
0.00943058591199622));
#40715=CARTESIAN_POINT('Ctrl Pts',(-0.220145194571405,0.00288044200687532,
0.0093057716638572));
#40716=CARTESIAN_POINT('Ctrl Pts',(-0.220230894847921,0.00247454997032606,
0.00905526038955808));
#40717=CARTESIAN_POINT('Ctrl Pts',(-0.220320732206519,0.00211923598389529,
0.00880483474782587));
#40718=CARTESIAN_POINT('Ctrl Pts',(-0.220393469212935,0.00185932807944966,
0.00859684197992795));
#40719=CARTESIAN_POINT('Ctrl Pts',(-0.220393469326552,0.00185932703395312,
0.00859684113942577));
#40720=CARTESIAN_POINT('Ctrl Pts',(-0.220266240041375,0.00185875869807335,
0.00859365486146192));
#40721=CARTESIAN_POINT('Ctrl Pts',(-0.220103936772937,0.0018605882269132,
0.00859165532427359));
#40722=CARTESIAN_POINT('Ctrl Pts',(-0.219926730734395,0.00187135174347915,
0.00859651152760235));
#40723=CARTESIAN_POINT('Ctrl Pts',(-0.219849192249158,0.00187769702112859,
0.00859995165438822));
#40724=CARTESIAN_POINT('Ctrl Pts',(-0.219683953461115,0.00190591750515629,
0.00861898651311973));
#40725=CARTESIAN_POINT('Ctrl Pts',(-0.219522447796733,0.00195479415049073,
0.0086541771714266));
#40726=CARTESIAN_POINT('Ctrl Pts',(-0.219420848743358,0.00201019267767576,
0.00869537988459834));
#40727=CARTESIAN_POINT('Ctrl Pts',(-0.219329691282643,0.00206995189687594,
0.00873874123435077));
#40728=CARTESIAN_POINT('Origin',(-0.21760795179008,0.00750000191208944,
0.00150723219269739));
#40729=CARTESIAN_POINT('',(-0.217094603861694,0.00749884707608177,0.0105144330567323));
#40730=CARTESIAN_POINT('',(-0.217213232792442,0.00253460675136436,0.0090261857131641));
#40731=CARTESIAN_POINT('Ctrl Pts',(-0.217213232792442,0.00253460675136436,
0.00902618571316409));
#40732=CARTESIAN_POINT('Ctrl Pts',(-0.217170309351211,0.00277579295122344,
0.00918442809411469));
#40733=CARTESIAN_POINT('Ctrl Pts',(-0.217117004028407,0.00309947496425187,
0.00937334421669727));
#40734=CARTESIAN_POINT('Ctrl Pts',(-0.21706463523819,0.00346758551596026,
0.0095627049050888));
#40735=CARTESIAN_POINT('Ctrl Pts',(-0.217040687245035,0.00365149899647496,
0.00965203925472441));
#40736=CARTESIAN_POINT('Ctrl Pts',(-0.217007699799833,0.00397270993102743,
0.00979619091369355));
#40737=CARTESIAN_POINT('Ctrl Pts',(-0.216979123906403,0.00436472477058794,
0.00995398513378322));
#40738=CARTESIAN_POINT('Ctrl Pts',(-0.216960097915139,0.00491864701878528,
0.0101420370266245));
#40739=CARTESIAN_POINT('Ctrl Pts',(-0.21696496840512,0.00539322729827493,
0.010266679263318));
#40740=CARTESIAN_POINT('Ctrl Pts',(-0.216978301352722,0.00578584987535544,
0.0103486271386283));
#40741=CARTESIAN_POINT('Ctrl Pts',(-0.216988380938197,0.0060059828310731,
0.0103881729924593));
#40742=CARTESIAN_POINT('Ctrl Pts',(-0.216999137729455,0.00620401844451835,
0.010419155240653));
#40743=CARTESIAN_POINT('Ctrl Pts',(-0.21700485626558,0.00629724070264874,
0.0104320669469113));
#40744=CARTESIAN_POINT('Ctrl Pts',(-0.217016575872302,0.00648013407847732,
0.0104558017273798));
#40745=CARTESIAN_POINT('Ctrl Pts',(-0.217040949115086,0.00682691734809784,
0.0104923617788424));
#40746=CARTESIAN_POINT('Ctrl Pts',(-0.217070787207733,0.00721009507694088,
0.0105138806616736));
#40747=CARTESIAN_POINT('Ctrl Pts',(-0.217094604615836,0.00749884651657513,
0.0105144330760153));
#40748=CARTESIAN_POINT('',(-0.217217320966152,0.0124615983754921,0.00902878263841572));
#40749=CARTESIAN_POINT('Ctrl Pts',(-0.217094604580183,0.00749884713502375,
0.0105144330753234));
#40750=CARTESIAN_POINT('Ctrl Pts',(-0.217070937522513,0.00778749281737824,
0.01051395809991));
#40751=CARTESIAN_POINT('Ctrl Pts',(-0.217041312684742,0.00817050093947764,
0.0104925590483005));
#40752=CARTESIAN_POINT('Ctrl Pts',(-0.217017156529758,0.00851709921734971,
0.0104561284919407));
#40753=CARTESIAN_POINT('Ctrl Pts',(-0.217005563781867,0.00869984918082267,
0.0104324752847162));
#40754=CARTESIAN_POINT('Ctrl Pts',(-0.216999909235435,0.00879305702910093,
0.0104195962148299));
#40755=CARTESIAN_POINT('Ctrl Pts',(-0.216989318519438,0.00899071226752479,
0.0103887488120621));
#40756=CARTESIAN_POINT('Ctrl Pts',(-0.216979434680228,0.00921060200406897,
0.0103493316559271));
#40757=CARTESIAN_POINT('Ctrl Pts',(-0.216966443804416,0.00960257895555559,
0.0102677731436431));
#40758=CARTESIAN_POINT('Ctrl Pts',(-0.216962353786427,0.0100798262263821,
0.0101422226623979));
#40759=CARTESIAN_POINT('Ctrl Pts',(-0.216981259047774,0.0106259713240169,
0.00995801306633485));
#40760=CARTESIAN_POINT('Ctrl Pts',(-0.217008015270036,0.0109796849032678,
0.00981495279359965));
#40761=CARTESIAN_POINT('Ctrl Pts',(-0.217026124783938,0.0111726831205931,
0.00973148164241474));
#40762=CARTESIAN_POINT('Ctrl Pts',(-0.217043798305059,0.0113336323415438,
0.00965791312087231));
#40763=CARTESIAN_POINT('Ctrl Pts',(-0.217054626933635,0.011421252747556,
0.00961622526465953));
#40764=CARTESIAN_POINT('Ctrl Pts',(-0.217075748242504,0.0115827300577152,
0.00953743738321973));
#40765=CARTESIAN_POINT('Ctrl Pts',(-0.217120156049393,0.0118899261409953,
0.00937864862166455));
#40766=CARTESIAN_POINT('Ctrl Pts',(-0.217174287324889,0.0122201761123988,
0.0091870018582681));
#40767=CARTESIAN_POINT('Ctrl Pts',(-0.217217320966152,0.0124615983754921,
0.00902878263841572));
#40768=CARTESIAN_POINT('',(-0.218253210572638,0.0126493218644601,0.00892398112026186));
#40769=CARTESIAN_POINT('Ctrl Pts',(-0.217217407969934,0.012461760044758,
0.00902867794239265));
#40770=CARTESIAN_POINT('Ctrl Pts',(-0.217390176156768,0.0125240868152205,
0.00899132591420084));
#40771=CARTESIAN_POINT('Ctrl Pts',(-0.217559211504655,0.0125854878241809,
0.00895315310690254));
#40772=CARTESIAN_POINT('Ctrl Pts',(-0.217872840726586,0.0126523647125971,
0.00891377523936488));
#40773=CARTESIAN_POINT('Ctrl Pts',(-0.218037719196302,0.0126678617041626,
0.00890646877918805));
#40774=CARTESIAN_POINT('Ctrl Pts',(-0.218252689489813,0.0126468959037447,
0.00892569856217048));
#40775=CARTESIAN_POINT('',(-0.218094234747031,0.00749853993277985,0.0105360606597374));
#40776=CARTESIAN_POINT('Ctrl Pts',(-0.21825294850133,0.0126481187356084,
0.00892485362262281));
#40777=CARTESIAN_POINT('Ctrl Pts',(-0.218213614101177,0.0124649627842807,
0.00905141958171181));
#40778=CARTESIAN_POINT('Ctrl Pts',(-0.218178110563308,0.0122764066318995,
0.00917173521317051));
#40779=CARTESIAN_POINT('Ctrl Pts',(-0.218033008484456,0.0113863756832155,
0.00969402331777485));
#40780=CARTESIAN_POINT('Ctrl Pts',(-0.217971681763306,0.010633235009572,
0.0100108663882326));
#40781=CARTESIAN_POINT('Ctrl Pts',(-0.217958148745726,0.00907579362155081,
0.0104298068455017));
#40782=CARTESIAN_POINT('Ctrl Pts',(-0.218002961139097,0.00828768224388102,
0.0105340872225598));
#40783=CARTESIAN_POINT('Ctrl Pts',(-0.218097863485635,0.00749998147943064,
0.0105361392872622));
#40784=CARTESIAN_POINT('',(-0.218256592144584,0.00234509828687441,0.00892021730379066));
#40785=CARTESIAN_POINT('Ctrl Pts',(-0.218094234747031,0.00749853993277985,
0.0105360606597374));
#40786=CARTESIAN_POINT('Ctrl Pts',(-0.218067229862006,0.00719461363377097,
0.0105354273206674));
#40787=CARTESIAN_POINT('Ctrl Pts',(-0.218034080490654,0.00679346748207321,
0.0105116869301656));
#40788=CARTESIAN_POINT('Ctrl Pts',(-0.21800818493669,0.00643215822152021,
0.0104716988671063));
#40789=CARTESIAN_POINT('Ctrl Pts',(-0.21799644503754,0.00624516791030783,
0.0104463965071334));
#40790=CARTESIAN_POINT('Ctrl Pts',(-0.217990618901119,0.00614435829544673,
0.0104316969225262));
#40791=CARTESIAN_POINT('Ctrl Pts',(-0.217981770592061,0.00596124495709672,
0.0104019555911123));
#40792=CARTESIAN_POINT('Ctrl Pts',(-0.217973610494308,0.00574494251941056,
0.0103621182566814));
#40793=CARTESIAN_POINT('Ctrl Pts',(-0.217964050770803,0.00535017373709659,
0.010278344750214));
#40794=CARTESIAN_POINT('Ctrl Pts',(-0.217965654179541,0.0047997316957265,
0.0101297502965913));
#40795=CARTESIAN_POINT('Ctrl Pts',(-0.217989855945059,0.0042083269497704,
0.0099166719695582));
#40796=CARTESIAN_POINT('Ctrl Pts',(-0.218020294338235,0.00380946035749678,
0.00974665422212974));
#40797=CARTESIAN_POINT('Ctrl Pts',(-0.218051893437689,0.00350742154534804,
0.00960429012063944));
#40798=CARTESIAN_POINT('Ctrl Pts',(-0.218079557608433,0.00330729544536573,
0.00950272759445357));
#40799=CARTESIAN_POINT('Ctrl Pts',(-0.218140179572864,0.00292838976944255,
0.00929780698585744));
#40800=CARTESIAN_POINT('Ctrl Pts',(-0.218204388361096,0.00259313741219679,
0.00909197882225042));
#40801=CARTESIAN_POINT('Ctrl Pts',(-0.218256592144584,0.00234509828687441,
0.00892021730379066));
#40802=CARTESIAN_POINT('Ctrl Pts',(-0.218256590177538,0.00234471180662227,
0.00891993757141349));
#40803=CARTESIAN_POINT('Ctrl Pts',(-0.218134550040916,0.00234639978140227,
0.00891846142581766));
#40804=CARTESIAN_POINT('Ctrl Pts',(-0.218030331307428,0.00234857254097845,
0.00891770527303425));
#40805=CARTESIAN_POINT('Ctrl Pts',(-0.217938284843155,0.00235370353966548,
0.00891928351630347));
#40806=CARTESIAN_POINT('Ctrl Pts',(-0.21789226158873,0.00235626904025144,
0.00892007263832024));
#40807=CARTESIAN_POINT('Ctrl Pts',(-0.217849294553891,0.00235959837297097,
0.00892146168011855));
#40808=CARTESIAN_POINT('Ctrl Pts',(-0.217815141143007,0.00236287402990444,
0.00892300578397156));
#40809=CARTESIAN_POINT('Ctrl Pts',(-0.217787234278518,0.00236555057997048,
0.00892426747631409));
#40810=CARTESIAN_POINT('Ctrl Pts',(-0.21776523359559,0.00236797977945377,
0.00892548211417782));
#40811=CARTESIAN_POINT('Ctrl Pts',(-0.217736542858525,0.00237174995177,
0.00892747026727036));
#40812=CARTESIAN_POINT('Ctrl Pts',(-0.217730120853637,0.00237259385009819,
0.00892791528647114));
#40813=CARTESIAN_POINT('Ctrl Pts',(-0.217723369119116,0.00237351184464279,
0.00892840402086493));
#40814=CARTESIAN_POINT('Ctrl Pts',(-0.217716155559666,0.00237453595774939,
0.00892895558766939));
#40815=CARTESIAN_POINT('Ctrl Pts',(-0.217676714940117,0.00238013536476782,
0.00893197131612372));
#40816=CARTESIAN_POINT('Ctrl Pts',(-0.217623386945995,0.00238937088151384,
0.00893719459845315));
#40817=CARTESIAN_POINT('Ctrl Pts',(-0.217575997502252,0.0024000928055468,
0.00894352742526225));
#40818=CARTESIAN_POINT('Ctrl Pts',(-0.217528608058509,0.00241081472957976,
0.00894986025207134));
#40819=CARTESIAN_POINT('Ctrl Pts',(-0.21748692365309,0.00242239208269951,
0.00895686377608915));
#40820=CARTESIAN_POINT('Ctrl Pts',(-0.217445993783405,0.00243562190843874,
0.00896496838443612));
#40821=CARTESIAN_POINT('Ctrl Pts',(-0.217364134044035,0.00246208155991719,
0.00898117760113005));
#40822=CARTESIAN_POINT('Ctrl Pts',(-0.217285909895761,0.00249586793471726,
0.009002268401476));
#40823=CARTESIAN_POINT('Ctrl Pts',(-0.217213846553127,0.00253441541015326,
0.00902621814787699));
#40824=CARTESIAN_POINT('Origin',(-0.215573530857847,0.00749999953571053,
0.00143242725109262));
#40825=CARTESIAN_POINT('',(-0.215095212480479,0.0074994624607262,0.0104691619874357));
#40826=CARTESIAN_POINT('',(-0.215184718243368,0.00267629428099901,0.00907717660912712));
#40827=CARTESIAN_POINT('Ctrl Pts',(-0.215184718243368,0.00267629428099901,
0.00907717660912712));
#40828=CARTESIAN_POINT('Ctrl Pts',(-0.215146525718128,0.00291333324471743,
0.00922581923697571));
#40829=CARTESIAN_POINT('Ctrl Pts',(-0.215099132128048,0.00323035142786572,
0.00940295055899245));
#40830=CARTESIAN_POINT('Ctrl Pts',(-0.215052529840506,0.00359027095313646,
0.0095804179996351));
#40831=CARTESIAN_POINT('Ctrl Pts',(-0.215031287815733,0.00376889701897786,
0.00966366879374054));
#40832=CARTESIAN_POINT('Ctrl Pts',(-0.215001646638346,0.00408470068498395,
0.00979968054158577));
#40833=CARTESIAN_POINT('Ctrl Pts',(-0.214976411300077,0.00446709191320605,
0.00994727203699884));
#40834=CARTESIAN_POINT('Ctrl Pts',(-0.214960404393782,0.00499883510574172,
0.0101209196609526));
#40835=CARTESIAN_POINT('Ctrl Pts',(-0.21496627361394,0.00546556789926266,
0.0102389566418329));
#40836=CARTESIAN_POINT('Ctrl Pts',(-0.214979945130265,0.00584476958512956,
0.0103149788292726));
#40837=CARTESIAN_POINT('Ctrl Pts',(-0.214990053470249,0.00605703382503594,
0.0103516623791654));
#40838=CARTESIAN_POINT('Ctrl Pts',(-0.215000719830354,0.00624722516962262,
0.0103803117380582));
#40839=CARTESIAN_POINT('Ctrl Pts',(-0.21500639948341,0.00633726586564142,
0.0103923346962857));
#40840=CARTESIAN_POINT('Ctrl Pts',(-0.2150180188578,0.00651372661228292,
0.0104144070541134));
#40841=CARTESIAN_POINT('Ctrl Pts',(-0.21504216176965,0.00684888162182612,
0.0104484989408323));
#40842=CARTESIAN_POINT('Ctrl Pts',(-0.215071675719688,0.00721973594776213,
0.0104686336712516));
#40843=CARTESIAN_POINT('Ctrl Pts',(-0.215095212937786,0.00749946183679744,
0.010469161998726));
#40844=CARTESIAN_POINT('',(-0.215187306909941,0.0123212872974831,0.00907875575671606));
#40845=CARTESIAN_POINT('Ctrl Pts',(-0.21509521288266,0.00749946249445561,
0.0104691619975665));
#40846=CARTESIAN_POINT('Ctrl Pts',(-0.215071829072947,0.00777843220526683,
0.0104686701414006));
#40847=CARTESIAN_POINT('Ctrl Pts',(-0.215042508186161,0.00814840410898096,
0.0104486874756129));
#40848=CARTESIAN_POINT('Ctrl Pts',(-0.215018521912491,0.00848302265137899,
0.010414771019284));
#40849=CARTESIAN_POINT('Ctrl Pts',(-0.215006981087804,0.00865925893055341,
0.0103927968298261));
#40850=CARTESIAN_POINT('Ctrl Pts',(-0.215001332092595,0.00874932749581215,
0.0103808046216084));
#40851=CARTESIAN_POINT('Ctrl Pts',(-0.214990761677216,0.00893910554359824,
0.0103522978628875));
#40852=CARTESIAN_POINT('Ctrl Pts',(-0.214980760303275,0.00915110651643444,
0.0103157592549189));
#40853=CARTESIAN_POINT('Ctrl Pts',(-0.214967291189273,0.00952991578169268,
0.0102400211047526));
#40854=CARTESIAN_POINT('Ctrl Pts',(-0.214961715433187,0.00999770202566206,
0.0101219354144702));
#40855=CARTESIAN_POINT('Ctrl Pts',(-0.21497805603957,0.0105281712554395,
0.00994897805687468));
#40856=CARTESIAN_POINT('Ctrl Pts',(-0.215003530828357,0.0109108254011088,
0.00980155134947677));
#40857=CARTESIAN_POINT('Ctrl Pts',(-0.215033385682381,0.0112272328548644,
0.00966546816384362));
#40858=CARTESIAN_POINT('Ctrl Pts',(-0.215054708220528,0.0114059998732139,
0.00958225194620914));
#40859=CARTESIAN_POINT('Ctrl Pts',(-0.215101483573991,0.0117664187103973,
0.00940474035128169));
#40860=CARTESIAN_POINT('Ctrl Pts',(-0.215149013018853,0.0120838921330146,
0.00922751589232591));
#40861=CARTESIAN_POINT('Ctrl Pts',(-0.215187306909941,0.0123212872974831,
0.00907875575671606));
#40862=CARTESIAN_POINT('',(-0.21619498111519,0.0123592223745629,0.00907662987181358));
#40863=CARTESIAN_POINT('Ctrl Pts',(-0.215187395634347,0.0123213065775708,
0.00907874549728632));
#40864=CARTESIAN_POINT('Ctrl Pts',(-0.215523256950413,0.0123339606047753,
0.00907807433826628));
#40865=CARTESIAN_POINT('Ctrl Pts',(-0.215859118725865,0.0123466006041971,
0.00907736836098088));
#40866=CARTESIAN_POINT('Ctrl Pts',(-0.216194981027653,0.0123592246090725,
0.00907662842429546));
#40867=CARTESIAN_POINT('',(-0.216094921541195,0.00749916570422793,0.0104908968200396));
#40868=CARTESIAN_POINT('Ctrl Pts',(-0.21619498111519,0.0123592223745629,
0.00907662987181358));
#40869=CARTESIAN_POINT('Ctrl Pts',(-0.216155362015906,0.0121196513974751,
0.00922839918985609));
#40870=CARTESIAN_POINT('Ctrl Pts',(-0.216106178511469,0.0117989338970978,
0.00940923223843171));
#40871=CARTESIAN_POINT('Ctrl Pts',(-0.216057811341763,0.0114349409820479,
0.00959017566794329));
#40872=CARTESIAN_POINT('Ctrl Pts',(-0.216035688926043,0.0112534767903711,
0.00967536323588877));
#40873=CARTESIAN_POINT('Ctrl Pts',(-0.216005069337273,0.010936292214568,
0.00981293044007726));
#40874=CARTESIAN_POINT('Ctrl Pts',(-0.215978741304516,0.0105517099265693,
0.00996241119423929));
#40875=CARTESIAN_POINT('Ctrl Pts',(-0.215961582825803,0.0100173646530297,
0.0101380807976369));
#40876=CARTESIAN_POINT('Ctrl Pts',(-0.21596673159867,0.0095493024043187,
0.0102572803569698));
#40877=CARTESIAN_POINT('Ctrl Pts',(-0.215979905520899,0.00916939986895247,
0.0103340767317814));
#40878=CARTESIAN_POINT('Ctrl Pts',(-0.215989775607879,0.00895666797254574,
0.0103711720214632));
#40879=CARTESIAN_POINT('Ctrl Pts',(-0.216000215681289,0.0087666271555183,
0.0104000960510575));
#40880=CARTESIAN_POINT('Ctrl Pts',(-0.216005897736623,0.00867501258808179,
0.0104124712062286));
#40881=CARTESIAN_POINT('Ctrl Pts',(-0.216017469984678,0.00849676060675789,
0.0104349965087626));
#40882=CARTESIAN_POINT('Ctrl Pts',(-0.216041627508878,0.00815759916772721,
0.0104698569176309));
#40883=CARTESIAN_POINT('Ctrl Pts',(-0.216071253207282,0.00778232161320312,
0.0104904084248528));
#40884=CARTESIAN_POINT('Ctrl Pts',(-0.216094921542323,0.00749916603381114,
0.0104908968200947));
#40885=CARTESIAN_POINT('',(-0.216191654426503,0.00263704645852275,0.00907417602083059));
#40886=CARTESIAN_POINT('Ctrl Pts',(-0.216094921541195,0.00749916570422794,
0.0104908968200396));
#40887=CARTESIAN_POINT('Ctrl Pts',(-0.216071192372307,0.00721653565110898,
0.0104903547759566));
#40888=CARTESIAN_POINT('Ctrl Pts',(-0.216041458964601,0.00684184722529076,
0.0104697980736088));
#40889=CARTESIAN_POINT('Ctrl Pts',(-0.216017167701719,0.00650321518860178,
0.0104349873050386));
#40890=CARTESIAN_POINT('Ctrl Pts',(-0.216005495918259,0.00632499391538343,
0.0104124603199507));
#40891=CARTESIAN_POINT('Ctrl Pts',(-0.215999785556795,0.00623389233782072,
0.0104001638087242));
#40892=CARTESIAN_POINT('Ctrl Pts',(-0.215989126899373,0.00604229502726595,
0.0103709986123811));
#40893=CARTESIAN_POINT('Ctrl Pts',(-0.215979049981255,0.00582832919195152,
0.0103336406317383));
#40894=CARTESIAN_POINT('Ctrl Pts',(-0.215965509745345,0.00544633154702591,
0.0102563020723301));
#40895=CARTESIAN_POINT('Ctrl Pts',(-0.215960018296731,0.00497512481975459,
0.0101358767402293));
#40896=CARTESIAN_POINT('Ctrl Pts',(-0.215976719095431,0.00444282320964421,
0.00996037719921713));
#40897=CARTESIAN_POINT('Ctrl Pts',(-0.2160026550059,0.0040591388957791,
0.00981098396273215));
#40898=CARTESIAN_POINT('Ctrl Pts',(-0.216032864044917,0.00374339550357232,
0.00967386268571153));
#40899=CARTESIAN_POINT('Ctrl Pts',(-0.21605487584295,0.00356169862545164,
0.00958848969233502));
#40900=CARTESIAN_POINT('Ctrl Pts',(-0.216103025180366,0.00319777204921344,
0.00940738142590156));
#40901=CARTESIAN_POINT('Ctrl Pts',(-0.216152098903379,0.00287680952339826,
0.00922623444225587));
#40902=CARTESIAN_POINT('Ctrl Pts',(-0.216191654426503,0.00263704645852275,
0.00907417602083059));
#40903=CARTESIAN_POINT('Ctrl Pts',(-0.216191653441714,0.00263701806743481,
0.0090741571960286));
#40904=CARTESIAN_POINT('Ctrl Pts',(-0.215856037597591,0.0026500960872135,
0.00907520307043243));
#40905=CARTESIAN_POINT('Ctrl Pts',(-0.215520422243746,0.00266318974959057,
0.0090762109895145));
#40906=CARTESIAN_POINT('Ctrl Pts',(-0.215184807285386,0.00267629643176575,
0.00907717990060014));
#40907=CARTESIAN_POINT('Origin',(-0.191547395567967,0.00749999908856939,
0.000492597042041278));
#40908=CARTESIAN_POINT('',(-0.192132144845555,0.0119762408965025,0.00882053073189916));
#40909=CARTESIAN_POINT('',(-0.191055849854836,0.0113889510484509,0.00908769145233091));
#40910=CARTESIAN_POINT('Ctrl Pts',(-0.191056614430799,0.0113898867221809,
0.0090872068420641));
#40911=CARTESIAN_POINT('Ctrl Pts',(-0.191117574310851,0.0114548399350986,
0.00905915673004499));
#40912=CARTESIAN_POINT('Ctrl Pts',(-0.191190506743783,0.0115169438727942,
0.00903175032826067));
#40913=CARTESIAN_POINT('Ctrl Pts',(-0.191270216528898,0.0115738470715757,
0.00900626058658664));
#40914=CARTESIAN_POINT('Ctrl Pts',(-0.191310071421455,0.0116022986709664,
0.00899351571574962));
#40915=CARTESIAN_POINT('Ctrl Pts',(-0.191351620396497,0.0116294555035853,
0.00898126176834248));
#40916=CARTESIAN_POINT('Ctrl Pts',(-0.191400054122322,0.011657748330379,
0.00896843433727955));
#40917=CARTESIAN_POINT('Ctrl Pts',(-0.191448487848146,0.0116860411571727,
0.00895560690621663));
#40918=CARTESIAN_POINT('Ctrl Pts',(-0.191503807137231,0.0117154517655055,
0.00894216860952244));
#40919=CARTESIAN_POINT('Ctrl Pts',(-0.191545244991808,0.0117363473659623,
0.00893257605113595));
#40920=CARTESIAN_POINT('Ctrl Pts',(-0.191586682846384,0.0117572429664192,
0.00892298349274945));
#40921=CARTESIAN_POINT('Ctrl Pts',(-0.191614238129345,0.0117696499199227,
0.00891728899045274));
#40922=CARTESIAN_POINT('Ctrl Pts',(-0.191651171850599,0.0117857911134441,
0.00890986709567738));
#40923=CARTESIAN_POINT('Ctrl Pts',(-0.191688105571854,0.0118019323069654,
0.00890244520090202));
#40924=CARTESIAN_POINT('Ctrl Pts',(-0.191734418368519,0.0118217927219441,
0.00889326660022605));
#40925=CARTESIAN_POINT('Ctrl Pts',(-0.191784295315848,0.0118423082724498,
0.00888372257736298));
#40926=CARTESIAN_POINT('Ctrl Pts',(-0.191884049210506,0.011883339373461,
0.00886463453163682));
#40927=CARTESIAN_POINT('Ctrl Pts',(-0.191998058757268,0.0119270141737984,
0.00884412853116881));
#40928=CARTESIAN_POINT('Ctrl Pts',(-0.192132145017542,0.0119762404947695,
0.00882053095199951));
#40929=CARTESIAN_POINT('',(-0.192104389150085,0.00749606093322131,0.00994933148053198));
#40930=CARTESIAN_POINT('Ctrl Pts',(-0.192132144845555,0.0119762408965025,
0.00882053073189916));
#40931=CARTESIAN_POINT('Ctrl Pts',(-0.192103715169681,0.0117490897743726,
0.00894225010388478));
#40932=CARTESIAN_POINT('Ctrl Pts',(-0.192068573234184,0.0114478633967073,
0.00908676981991131));
#40933=CARTESIAN_POINT('Ctrl Pts',(-0.192034329267438,0.0111082303760389,
0.00923117662410021));
#40934=CARTESIAN_POINT('Ctrl Pts',(-0.19201889600854,0.0109412049797955,
0.00929844365315326));
#40935=CARTESIAN_POINT('Ctrl Pts',(-0.191997561428072,0.0106431647032832,
0.00940955553695104));
#40936=CARTESIAN_POINT('Ctrl Pts',(-0.191980397858888,0.010285777696736,
0.00952909690683793));
#40937=CARTESIAN_POINT('Ctrl Pts',(-0.191971805248502,0.00979625382147503,
0.00966822026083504));
#40938=CARTESIAN_POINT('Ctrl Pts',(-0.191980496803262,0.0093617963463922,
0.00976413432443437));
#40939=CARTESIAN_POINT('Ctrl Pts',(-0.19199493540629,0.00901347121364747,
0.00982508008438882));
#40940=CARTESIAN_POINT('Ctrl Pts',(-0.192005038620267,0.00881887992917666,
0.00985447421971926));
#40941=CARTESIAN_POINT('Ctrl Pts',(-0.192015409865108,0.00864506423045702,
0.00987737947917409));
#40942=CARTESIAN_POINT('Ctrl Pts',(-0.192020861696104,0.00856256927112993,
0.00988702574005904));
#40943=CARTESIAN_POINT('Ctrl Pts',(-0.192031955449212,0.00840095045736884,
0.00990472890594345));
#40944=CARTESIAN_POINT('Ctrl Pts',(-0.192054786510697,0.00809374315339341,
0.00993211432591152));
#40945=CARTESIAN_POINT('Ctrl Pts',(-0.192082412664333,0.00775366058309626,
0.00994830547279376));
#40946=CARTESIAN_POINT('Ctrl Pts',(-0.192104324882764,0.00749698449310426,
0.00994869951306347));
#40947=CARTESIAN_POINT('',(-0.192122489455637,0.00301997722274325,0.00881827773461044));
#40948=CARTESIAN_POINT('Ctrl Pts',(-0.192108700682526,0.00749526582339488,
0.0099487938961807));
#40949=CARTESIAN_POINT('Ctrl Pts',(-0.192103230217472,0.00744949681047625,
0.00994865204056603));
#40950=CARTESIAN_POINT('Ctrl Pts',(-0.192097918522563,0.00740368269194635,
0.00994818073646005));
#40951=CARTESIAN_POINT('Ctrl Pts',(-0.191981016723199,0.00636317794369435,
0.00992996660640991));
#40952=CARTESIAN_POINT('Ctrl Pts',(-0.191946332157474,0.00536896481747056,
0.00975679744953434));
#40953=CARTESIAN_POINT('Ctrl Pts',(-0.192015267591331,0.00393288153336258,
0.00926171219322835));
#40954=CARTESIAN_POINT('Ctrl Pts',(-0.192058801228599,0.00346626441370585,
0.00905753219206862));
#40955=CARTESIAN_POINT('Ctrl Pts',(-0.192122301842675,0.00301972304784883,
0.00881813661224312));
#40956=CARTESIAN_POINT('',(-0.191053639265561,0.00360252014973371,0.0090841498220513));
#40957=CARTESIAN_POINT('Ctrl Pts',(-0.192122489455637,0.00301997722274325,
0.00881827773461044));
#40958=CARTESIAN_POINT('Ctrl Pts',(-0.191991549101578,0.00306796965600734,
0.00884130847560521));
#40959=CARTESIAN_POINT('Ctrl Pts',(-0.191879858919587,0.00311067479627433,
0.00886139413752867));
#40960=CARTESIAN_POINT('Ctrl Pts',(-0.191781902301749,0.00315083974748719,
0.00888011500123793));
#40961=CARTESIAN_POINT('Ctrl Pts',(-0.191732037727987,0.00317128561645069,
0.00888964481055488));
#40962=CARTESIAN_POINT('Ctrl Pts',(-0.191685732156451,0.00319107891156394,
0.00889881027145093));
#40963=CARTESIAN_POINT('Ctrl Pts',(-0.191648801068625,0.00320716638729363,
0.00890622211943673));
#40964=CARTESIAN_POINT('Ctrl Pts',(-0.191611869980799,0.00322325386302332,
0.00891363396742254));
#40965=CARTESIAN_POINT('Ctrl Pts',(-0.191584312743833,0.00323562056547369,
0.00891932133001983));
#40966=CARTESIAN_POINT('Ctrl Pts',(-0.191542866130379,0.00325644619026458,
0.00892890116478443));
#40967=CARTESIAN_POINT('Ctrl Pts',(-0.191501419516925,0.00327727181505547,
0.00893848099954903));
#40968=CARTESIAN_POINT('Ctrl Pts',(-0.191446084656406,0.00330658260963377,
0.00895190132394306));
#40969=CARTESIAN_POINT('Ctrl Pts',(-0.19139762533046,0.0033347802690586,
0.00896471272346431));
#40970=CARTESIAN_POINT('Ctrl Pts',(-0.191349166004514,0.00336297792848342,
0.00897752412298555));
#40971=CARTESIAN_POINT('Ctrl Pts',(-0.191307581406187,0.00339004431685584,
0.00898976373818474));
#40972=CARTESIAN_POINT('Ctrl Pts',(-0.191267681664384,0.00341840149675534,
0.0090024944772828));
#40973=CARTESIAN_POINT('Ctrl Pts',(-0.19118788218078,0.00347511585655432,
0.00902795595547893));
#40974=CARTESIAN_POINT('Ctrl Pts',(-0.191114823138575,0.00353701496799355,
0.00905533519994708));
#40975=CARTESIAN_POINT('Ctrl Pts',(-0.191053698914977,0.00360175590961342,
0.00908336191387111));
#40976=CARTESIAN_POINT('',(-0.191108184220926,0.00749768564093594,0.00992694022012107));
#40977=CARTESIAN_POINT('Ctrl Pts',(-0.191051632810295,0.00360221947727921,
0.0090835271983084));
#40978=CARTESIAN_POINT('Ctrl Pts',(-0.191021186878507,0.00392206635238341,
0.00922786958441169));
#40979=CARTESIAN_POINT('Ctrl Pts',(-0.190999811324095,0.00425072879523787,
0.00935489154048301));
#40980=CARTESIAN_POINT('Ctrl Pts',(-0.19095367527545,0.00553194090199199,
0.00976957032772443));
#40981=CARTESIAN_POINT('Ctrl Pts',(-0.190993468703091,0.0065152661879122,
0.0099245060075464));
#40982=CARTESIAN_POINT('Ctrl Pts',(-0.191104699967524,0.00749947736827617,
0.00992697735777636));
#40983=CARTESIAN_POINT('Ctrl Pts',(-0.191108093501586,0.00749933750016912,
0.00992705109316002));
#40984=CARTESIAN_POINT('Ctrl Pts',(-0.191061680806587,0.00790407504383842,
0.00992607079981439));
#40985=CARTESIAN_POINT('Ctrl Pts',(-0.191027478698722,0.0083095718978316,
0.00989932465622092));
#40986=CARTESIAN_POINT('Ctrl Pts',(-0.190955876152719,0.00964018279270969,
0.00972531409106423));
#40987=CARTESIAN_POINT('Ctrl Pts',(-0.190972448810475,0.0105416572289866,
0.00946878822548761));
#40988=CARTESIAN_POINT('Ctrl Pts',(-0.191053991198766,0.0113881984379763,
0.00908791315351825));
#40989=CARTESIAN_POINT('Origin',(-0.228243019758013,0.0143258968887991,
-0.00627376866199084));
#40990=CARTESIAN_POINT('Origin',(-0.228011089022205,0.0141214482232033,
0.00627054897881623));
#40991=CARTESIAN_POINT('Ctrl Pts',(-0.204265073067,0.0127803686690591,-0.00856007647208766));
#40992=CARTESIAN_POINT('Ctrl Pts',(-0.204262729393093,0.0128387107088317,
-0.00864367908736358));
#40993=CARTESIAN_POINT('Ctrl Pts',(-0.204363894126176,0.0128284728860937,
-0.00865137065812417));
#40994=CARTESIAN_POINT('Ctrl Pts',(-0.204128064700356,0.0119492725903312,
-0.00913958927820265));
#40995=CARTESIAN_POINT('Ctrl Pts',(-0.204125477102728,0.011998566632778,
-0.00922956161310565));
#40996=CARTESIAN_POINT('Ctrl Pts',(-0.204226296468488,0.0119847835364124,
-0.00923756796894809));
#40997=CARTESIAN_POINT('Ctrl Pts',(-0.20384472208749,0.0100688601319156,
-0.0100298347632221));
#40998=CARTESIAN_POINT('Ctrl Pts',(-0.203841777898438,0.0100970878860094,
-0.0101297217092875));
#40999=CARTESIAN_POINT('Ctrl Pts',(-0.203944562018244,0.0100968720882839,
-0.010127895382756));
#41000=CARTESIAN_POINT('Ctrl Pts',(-0.20405840592736,0.00799378812699186,
-0.0102626707868758));
#41001=CARTESIAN_POINT('Ctrl Pts',(-0.204055334959227,0.00799938949731187,
-0.0103650911256359));
#41002=CARTESIAN_POINT('Ctrl Pts',(-0.204156746755187,0.00800979415998372,
-0.0103656374081853));
#41003=CARTESIAN_POINT('Ctrl Pts',(-0.204143725320899,0.00697638819353669,
-0.0102055690374362));
#41004=CARTESIAN_POINT('Ctrl Pts',(-0.204140678288162,0.00697055492621437,
-0.0103073359394314));
#41005=CARTESIAN_POINT('Ctrl Pts',(-0.204242317153123,0.00697890273577786,
-0.0103088949221699));
#41006=CARTESIAN_POINT('Ctrl Pts',(-0.204098738700262,0.00750019395234659,
-0.0102204142510564));
#41007=CARTESIAN_POINT('Ctrl Pts',(-0.204098590806404,0.00750019416653296,
-0.0102269583017623));
#41008=CARTESIAN_POINT('Ctrl Pts',(-0.204099088227802,0.00750019418365599,
-0.0102335006756741));
#41009=CARTESIAN_POINT('Ctrl Pts',(-0.204101430857704,0.00750019381893088,
-0.0102468030395632));
#41010=CARTESIAN_POINT('Ctrl Pts',(-0.204103353066049,0.00750019341260105,
-0.0102535132046417));
#41011=CARTESIAN_POINT('Ctrl Pts',(-0.204110778163236,0.00750019166647608,
-0.0102719147849014));
#41012=CARTESIAN_POINT('Ctrl Pts',(-0.204117865186854,0.00750018983664796,
-0.0102828141944625));
#41013=CARTESIAN_POINT('Ctrl Pts',(-0.204135782840589,0.0075001851440154,
-0.0103013364231896));
#41014=CARTESIAN_POINT('Ctrl Pts',(-0.204146447502616,0.00750018224294542,
-0.0103087848563091));
#41015=CARTESIAN_POINT('Ctrl Pts',(-0.204168356804244,0.00750017719045867,
-0.0103185177811627));
#41016=CARTESIAN_POINT('Ctrl Pts',(-0.204179152845045,0.0075001616685909,
-0.0103213085170776));
#41017=CARTESIAN_POINT('Ctrl Pts',(-0.204192375920369,0.00750018573349939,
-0.010322485851024));
#41018=CARTESIAN_POINT('Ctrl Pts',(-0.204194617299677,0.00750016630405051,
-0.0103226107361709));
#41019=CARTESIAN_POINT('Ctrl Pts',(-0.204196829921526,0.00750016559189676,
-0.0103226607415403));
#41020=CARTESIAN_POINT('Ctrl Pts',(-0.204181325032408,0.012257065641656,
-0.0089007774107484));
#41021=CARTESIAN_POINT('Ctrl Pts',(-0.204181296960589,0.0122609820637786,
-0.00890705005018559));
#41022=CARTESIAN_POINT('Ctrl Pts',(-0.204182202033119,0.0122655230269731,
-0.0089127959082597));
#41023=CARTESIAN_POINT('Ctrl Pts',(-0.204186011734323,0.0122765363438471,
-0.00892409037649733));
#41024=CARTESIAN_POINT('Ctrl Pts',(-0.204189199583018,0.0122830325026838,
-0.00892921331103979));
#41025=CARTESIAN_POINT('Ctrl Pts',(-0.204199541926441,0.0123005310075908,
-0.00894012819848833));
#41026=CARTESIAN_POINT('Ctrl Pts',(-0.204208309649517,0.0123124975679202,
-0.00894480621639041));
#41027=CARTESIAN_POINT('Ctrl Pts',(-0.204229550306519,0.0123373226808868,
-0.00894949032305491));
#41028=CARTESIAN_POINT('Ctrl Pts',(-0.204241261291575,0.0123493418130815,
-0.00894941000383247));
#41029=CARTESIAN_POINT('Ctrl Pts',(-0.204270868303184,0.0123769117862931,
-0.00894476547705386));
#41030=CARTESIAN_POINT('Ctrl Pts',(-0.204285432901854,0.0123881214336822,
-0.00893862798591079));
#41031=CARTESIAN_POINT('Ctrl Pts',(-0.204290480284829,0.0123917113386855,
-0.00893668244562294));
#41032=CARTESIAN_POINT('Ctrl Pts',(-0.204291371857698,0.012392496384385,
-0.0089362358274016));
#41033=CARTESIAN_POINT('Ctrl Pts',(-0.20429256803976,0.0123935448586381,
-0.00893563119921439));
#41034=CARTESIAN_POINT('Ctrl Pts',(-0.20429352351428,0.0123942615368791,
-0.00893520764733819));
#41035=CARTESIAN_POINT('Origin',(-0.204344423434958,0.012341683860884,-0.00885114476085288));
#41036=CARTESIAN_POINT('Ctrl Pts',(-0.203181004915558,0.0122576992722632,
-0.00887926075513702));
#41037=CARTESIAN_POINT('Ctrl Pts',(-0.203180880319866,0.0122616709335099,
-0.00888578894591877));
#41038=CARTESIAN_POINT('Ctrl Pts',(-0.203179990406391,0.0122663403805014,
-0.00889176162511392));
#41039=CARTESIAN_POINT('Ctrl Pts',(-0.203176628181342,0.012277395470525,
-0.00890301597230118));
#41040=CARTESIAN_POINT('Ctrl Pts',(-0.203174034602288,0.0122837777646263,
-0.00890801287099688));
#41041=CARTESIAN_POINT('Ctrl Pts',(-0.203165609250051,0.0123012757963656,
-0.00891867551477168));
#41042=CARTESIAN_POINT('Ctrl Pts',(-0.2031586136738,0.0123132348356185,
-0.00892310403449977));
#41043=CARTESIAN_POINT('Ctrl Pts',(-0.203142310649237,0.0123374075395989,
-0.00892703668417647));
#41044=CARTESIAN_POINT('Ctrl Pts',(-0.20313364719466,0.0123488884750934,
-0.00892677050332955));
#41045=CARTESIAN_POINT('Ctrl Pts',(-0.203113574189725,0.0123732482306594,
-0.00892228087227181));
#41046=CARTESIAN_POINT('Ctrl Pts',(-0.20310390248531,0.0123834505968482,
-0.00891756729833953));
#41047=CARTESIAN_POINT('Ctrl Pts',(-0.203096855974668,0.0123907471432063,
-0.00891357268518451));
#41048=CARTESIAN_POINT('Ctrl Pts',(-0.203094724720638,0.0123928548299233,
-0.00891238941300899));
#41049=CARTESIAN_POINT('Ctrl Pts',(-0.203092585205556,0.012394904002844,
-0.00891112094646253));
#41050=CARTESIAN_POINT('Ctrl Pts',(-0.203091800754282,0.0123956724650861,
-0.00891063229697375));
#41051=CARTESIAN_POINT('Ctrl Pts',(-0.204143997496444,0.00802323628381861,
-0.010205565063399));
#41052=CARTESIAN_POINT('Ctrl Pts',(-0.204140860611556,0.00802908085166497,
-0.0103074831625607));
#41053=CARTESIAN_POINT('Ctrl Pts',(-0.204242648149941,0.00802065830824136,
-0.0103089801716569));
#41054=CARTESIAN_POINT('Ctrl Pts',(-0.204058120672358,0.0070071871206502,
-0.0102622885094666));
#41055=CARTESIAN_POINT('Ctrl Pts',(-0.204054960205719,0.00700159695666881,
-0.0103648577443184));
#41056=CARTESIAN_POINT('Ctrl Pts',(-0.204156519163295,0.00699110367585506,
-0.0103653309638915));
#41057=CARTESIAN_POINT('Ctrl Pts',(-0.203843718954951,0.00493709923159828,
-0.0100315643925817));
#41058=CARTESIAN_POINT('Ctrl Pts',(-0.203840683456935,0.00490889608674471,
-0.0101316222849361));
#41059=CARTESIAN_POINT('Ctrl Pts',(-0.20394362305939,0.00490914794716083,
-0.0101297299846125));
#41060=CARTESIAN_POINT('Ctrl Pts',(-0.204127350940855,0.00305239049180689,
-0.00914022524378526));
#41061=CARTESIAN_POINT('Ctrl Pts',(-0.204124674731928,0.0030030291564167,
-0.00923033259386805));
#41062=CARTESIAN_POINT('Ctrl Pts',(-0.204225653522232,0.00301681463646749,
-0.00923826204389967));
#41063=CARTESIAN_POINT('Ctrl Pts',(-0.204263087479502,0.00222512775952759,
-0.00856364933328716));
#41064=CARTESIAN_POINT('Ctrl Pts',(-0.204260654022477,0.00216675058638386,
-0.00864741054064513));
#41065=CARTESIAN_POINT('Ctrl Pts',(-0.204361977315468,0.00217701080273715,
-0.00865502494961599));
#41066=CARTESIAN_POINT('Ctrl Pts',(-0.204292070928345,0.00260973041950684,
-0.00893764167137754));
#41067=CARTESIAN_POINT('Ctrl Pts',(-0.204291025482645,0.0026105155431871,
-0.00893810511839575));
#41068=CARTESIAN_POINT('Ctrl Pts',(-0.204288291638048,0.00261253468312918,
-0.00893925983789712));
#41069=CARTESIAN_POINT('Ctrl Pts',(-0.204285564855784,0.00261461434218402,
-0.00894033431311169));
#41070=CARTESIAN_POINT('Ctrl Pts',(-0.204276064531964,0.00262215153202754,
-0.00894413460675116));
#41071=CARTESIAN_POINT('Ctrl Pts',(-0.204263487933207,0.00263243098352953,
-0.0089483423375052));
#41072=CARTESIAN_POINT('Ctrl Pts',(-0.204238165020081,0.00265635914450468,
-0.00895184060040076));
#41073=CARTESIAN_POINT('Ctrl Pts',(-0.204227085909756,0.00266784811865962,
-0.00895174571839484));
#41074=CARTESIAN_POINT('Ctrl Pts',(-0.204206485960734,0.00269205167398984,
-0.00894702757360248));
#41075=CARTESIAN_POINT('Ctrl Pts',(-0.204197817017632,0.00270394972816067,
-0.00894230284157555));
#41076=CARTESIAN_POINT('Ctrl Pts',(-0.204187634236843,0.00272129696193903,
-0.00893136919571814));
#41077=CARTESIAN_POINT('Ctrl Pts',(-0.204184510539432,0.00272771010242592,
-0.00892627211040956));
#41078=CARTESIAN_POINT('Ctrl Pts',(-0.204180778308437,0.00273858477453516,
-0.00891506519824069));
#41079=CARTESIAN_POINT('Ctrl Pts',(-0.204179892226625,0.00274307102426783,
-0.00890937100289297));
#41080=CARTESIAN_POINT('Ctrl Pts',(-0.204179919702534,0.0027469445005241,
-0.00890316186212408));
#41081=CARTESIAN_POINT('Ctrl Pts',(-0.203143271812693,0.00698365837066073,
-0.0101836772736148));
#41082=CARTESIAN_POINT('Ctrl Pts',(-0.203141490914464,0.00697759707409294,
-0.0102900221295829));
#41083=CARTESIAN_POINT('Ctrl Pts',(-0.203035646026025,0.00696931019329735,
-0.0102810055802145));
#41084=CARTESIAN_POINT('Ctrl Pts',(-0.203057844304204,0.0080065505568688,
-0.0102395474721513));
#41085=CARTESIAN_POINT('Ctrl Pts',(-0.203056046122935,0.00801244156714122,
-0.0103465781511104));
#41086=CARTESIAN_POINT('Ctrl Pts',(-0.202950428971978,0.0080013749484015,
-0.0103385156607444));
#41087=CARTESIAN_POINT('Ctrl Pts',(-0.202848075368191,0.0100621302750322,
-0.0100051837092143));
#41088=CARTESIAN_POINT('Ctrl Pts',(-0.20284637539565,0.0100914860875319,
-0.0101095507090941));
#41089=CARTESIAN_POINT('Ctrl Pts',(-0.202739297675281,0.0100893700411261,
-0.0101043269775615));
#41090=CARTESIAN_POINT('Ctrl Pts',(-0.20312348077053,0.0119264298985161,
-0.00913154104380249));
#41091=CARTESIAN_POINT('Ctrl Pts',(-0.203122192521676,0.0119776612356224,
-0.00922571207633984));
#41092=CARTESIAN_POINT('Ctrl Pts',(-0.20301715666529,0.0119884333075752,
-0.0092108489932237));
#41093=CARTESIAN_POINT('Ctrl Pts',(-0.203261844553021,0.0127629120170625,
-0.00855350135677558));
#41094=CARTESIAN_POINT('Ctrl Pts',(-0.203260802723471,0.0128236026115707,
-0.00864104139382898));
#41095=CARTESIAN_POINT('Ctrl Pts',(-0.203155408062606,0.0128300897901739,
-0.00862693568704257));
#41096=CARTESIAN_POINT('Ctrl Pts',(-0.203101179356735,0.00746966964796713,
-0.0102067046864171));
#41097=CARTESIAN_POINT('Ctrl Pts',(-0.203099854724934,0.00747070927761228,
-0.0102176727827858));
#41098=CARTESIAN_POINT('Ctrl Pts',(-0.203096735385425,0.00747151343855428,
-0.0102283717733987));
#41099=CARTESIAN_POINT('Ctrl Pts',(-0.203086474952352,0.00747277282275856,
-0.010249734057713));
#41100=CARTESIAN_POINT('Ctrl Pts',(-0.203078924411847,0.00747318532340408,
-0.0102599911857472));
#41101=CARTESIAN_POINT('Ctrl Pts',(-0.203060454056968,0.00747281561145981,
-0.0102772439408748));
#41102=CARTESIAN_POINT('Ctrl Pts',(-0.203050700793186,0.00747201479849369,
-0.010283086345843));
#41103=CARTESIAN_POINT('Ctrl Pts',(-0.203036935787999,0.00746867281090778,
-0.0102893158064833));
#41104=CARTESIAN_POINT('Ctrl Pts',(-0.203031522359902,0.00746676460049837,
-0.0102911830158309));
#41105=CARTESIAN_POINT('Ctrl Pts',(-0.203026437789923,0.00746335128295609,
-0.0102925387461303));
#41106=CARTESIAN_POINT('Ctrl Pts',(-0.203025927392644,0.00746299355861727,
-0.0102926715115178));
#41107=CARTESIAN_POINT('Origin',(-0.203018630792398,0.0026610259015663,
-0.00882665770830219));
#41108=CARTESIAN_POINT('Ctrl Pts',(-0.20317320031072,0.00274689768611898,
-0.00888128997470166));
#41109=CARTESIAN_POINT('Ctrl Pts',(-0.203173025615196,0.00274389089988737,
-0.00888629384615075));
#41110=CARTESIAN_POINT('Ctrl Pts',(-0.203172429950494,0.00274045322122823,
-0.00889101255376211));
#41111=CARTESIAN_POINT('Ctrl Pts',(-0.20316959601839,0.00272971614503562,
-0.0089033005435487));
#41112=CARTESIAN_POINT('Ctrl Pts',(-0.203166494707998,0.00272180664330849,
-0.00890980481065451));
#41113=CARTESIAN_POINT('Ctrl Pts',(-0.203157477023721,0.00270296534417372,
-0.00892114361452894));
#41114=CARTESIAN_POINT('Ctrl Pts',(-0.2031511876556,0.00269197143508385,
-0.00892515254381942));
#41115=CARTESIAN_POINT('Ctrl Pts',(-0.203133615926001,0.00266420206416287,
-0.00893042371830774));
#41116=CARTESIAN_POINT('Ctrl Pts',(-0.203122454277358,0.00264914254816469,
-0.00892877786070083));
#41117=CARTESIAN_POINT('Ctrl Pts',(-0.203109312459774,0.00263034302082137,
-0.00892395358816016));
#41118=CARTESIAN_POINT('Ctrl Pts',(-0.203104868123276,0.00262369280401741,
-0.00892137703935346));
#41119=CARTESIAN_POINT('Ctrl Pts',(-0.203101838781183,0.00261554887056482,
-0.00891742625592927));
#41120=CARTESIAN_POINT('Ctrl Pts',(-0.203101402755506,0.00261337739142643,
-0.0089162616978424));
#41121=CARTESIAN_POINT('Ctrl Pts',(-0.203101377855557,0.00261069939040457,
-0.00891472500874586));
#41122=CARTESIAN_POINT('Ctrl Pts',(-0.203101415214044,0.0026100532038125,
-0.00891434527384206));
#41123=CARTESIAN_POINT('Ctrl Pts',(-0.203101497042113,0.00260941164989306,
-0.00891395940072847));
#41124=CARTESIAN_POINT('Origin',(-0.206699882182129,0.00706535101846166,
-0.00270713639773735));
#41125=CARTESIAN_POINT('Ctrl Pts',(-0.206265373707575,0.0127777966478479,
-0.00859997364655191));
#41126=CARTESIAN_POINT('Ctrl Pts',(-0.20626304639632,0.012836204592148,
-0.00868330038990975));
#41127=CARTESIAN_POINT('Ctrl Pts',(-0.206364024979952,0.0128261001065475,
-0.00869114028853961));
#41128=CARTESIAN_POINT('Ctrl Pts',(-0.206129048262261,0.011947813807502,
-0.00918129811142922));
#41129=CARTESIAN_POINT('Ctrl Pts',(-0.206126478296519,0.0119971744172948,
-0.00927102308516758));
#41130=CARTESIAN_POINT('Ctrl Pts',(-0.206227111583568,0.0119835677514146,
-0.00927917721234948));
#41131=CARTESIAN_POINT('Ctrl Pts',(-0.205843113708995,0.0100692150364398,
-0.0100742796343862));
#41132=CARTESIAN_POINT('Ctrl Pts',(-0.205840189802564,0.0100974870119682,
-0.0101739681899843));
#41133=CARTESIAN_POINT('Ctrl Pts',(-0.205942785236712,0.0100970730771734,
-0.0101723622736461));
#41134=CARTESIAN_POINT('Ctrl Pts',(-0.206056905618493,0.00799330463484866,
-0.010308040249357));
#41135=CARTESIAN_POINT('Ctrl Pts',(-0.206053854566429,0.00799891449469382,
-0.0104102754427349));
#41136=CARTESIAN_POINT('Ctrl Pts',(-0.206155065185868,0.00800948684235285,
-0.0104109713944681));
#41137=CARTESIAN_POINT('Ctrl Pts',(-0.206143839207489,0.00697634899411554,
-0.0102507166129379));
#41138=CARTESIAN_POINT('Ctrl Pts',(-0.206140812015937,0.0069705060182345,
-0.0103522948486019));
#41139=CARTESIAN_POINT('Ctrl Pts',(-0.206242251803155,0.00697892476553575,
-0.0103540372485459));
#41140=CARTESIAN_POINT('Ctrl Pts',(-0.206098147225107,0.00750010495671034,
-0.0102656023871143));
#41141=CARTESIAN_POINT('Ctrl Pts',(-0.20609799932479,0.00750010511644564,
-0.0102721467492724));
#41142=CARTESIAN_POINT('Ctrl Pts',(-0.206098496860782,0.00750010510170206,
-0.0102786894234506));
#41143=CARTESIAN_POINT('Ctrl Pts',(-0.206100839967226,0.00750010471944094,
-0.010291992420886));
#41144=CARTESIAN_POINT('Ctrl Pts',(-0.20610276255874,0.0075001043305413,
-0.0102987028842377));
#41145=CARTESIAN_POINT('Ctrl Pts',(-0.20611018892991,0.00750010270993599,
-0.010317104869771));
#41146=CARTESIAN_POINT('Ctrl Pts',(-0.206117276936597,0.00750010105092799,
-0.0103280041761893));
#41147=CARTESIAN_POINT('Ctrl Pts',(-0.206135196697436,0.00750009687187179,
-0.0103465261516109));
#41148=CARTESIAN_POINT('Ctrl Pts',(-0.206145862546723,0.00750009430132802,
-0.0103539743426226));
#41149=CARTESIAN_POINT('Ctrl Pts',(-0.206167775052211,0.00750009006200001,
-0.0103637073224297));
#41150=CARTESIAN_POINT('Ctrl Pts',(-0.206178571379276,0.00750007378825076,
-0.0103664970753006));
#41151=CARTESIAN_POINT('Ctrl Pts',(-0.206191789970321,0.00750010082790921,
-0.0103676740516232));
#41152=CARTESIAN_POINT('Ctrl Pts',(-0.206194036900753,0.00750007978106561,
-0.0103677992460968));
#41153=CARTESIAN_POINT('Ctrl Pts',(-0.206196247266376,0.00750007914373993,
-0.0103678492117139));
#41154=CARTESIAN_POINT('Ctrl Pts',(-0.206181817694621,0.0122551267607735,
-0.00894171598702609));
#41155=CARTESIAN_POINT('Ctrl Pts',(-0.20618178860154,0.0122590539690899,
-0.00894798079528798));
#41156=CARTESIAN_POINT('Ctrl Pts',(-0.206182692488116,0.0122636047879427,
-0.00895371774478208));
#41157=CARTESIAN_POINT('Ctrl Pts',(-0.206186498221275,0.0122746343758503,
-0.00896498778296844));
#41158=CARTESIAN_POINT('Ctrl Pts',(-0.206189682130124,0.0122811357191452,
-0.00897009628597565));
#41159=CARTESIAN_POINT('Ctrl Pts',(-0.206200014724264,0.0122986475116484,
-0.00898097783826835));
#41160=CARTESIAN_POINT('Ctrl Pts',(-0.206208776639363,0.0123106204169374,
-0.00898563506172976));
#41161=CARTESIAN_POINT('Ctrl Pts',(-0.206229865025598,0.0123352875681986,
-0.00899024734596498));
#41162=CARTESIAN_POINT('Ctrl Pts',(-0.206241398738038,0.0123471495980202,
-0.0089901803069501));
#41163=CARTESIAN_POINT('Ctrl Pts',(-0.206270681041155,0.0123744968585233,
-0.00898565892481136));
#41164=CARTESIAN_POINT('Ctrl Pts',(-0.206285145158284,0.0123856175724812,
-0.00897964283157976));
#41165=CARTESIAN_POINT('Ctrl Pts',(-0.206290134239438,0.012389286123914,
-0.00897768187932079));
#41166=CARTESIAN_POINT('Ctrl Pts',(-0.206291280718472,0.0123902435954362,
-0.00897714552013086));
#41167=CARTESIAN_POINT('Ctrl Pts',(-0.206292817844583,0.0123915197022351,
-0.00897641524707116));
#41168=CARTESIAN_POINT('Ctrl Pts',(-0.206294013519307,0.0123924158224524,
-0.00897588334166704));
#41169=CARTESIAN_POINT('Origin',(-0.206344964115316,0.0123396857707647,
-0.0088919177026923));
#41170=CARTESIAN_POINT('Ctrl Pts',(-0.205181552286433,0.0122555409350824,
-0.00892029894995692));
#41171=CARTESIAN_POINT('Ctrl Pts',(-0.205181427582414,0.0122595243991831,
-0.00892681884907278));
#41172=CARTESIAN_POINT('Ctrl Pts',(-0.205180537761043,0.012264204315227,
-0.00893278217335894));
#41173=CARTESIAN_POINT('Ctrl Pts',(-0.205177176102581,0.01227527836818,
-0.00894401489787914));
#41174=CARTESIAN_POINT('Ctrl Pts',(-0.205174583048941,0.0122816686296184,
-0.0089489997063002));
#41175=CARTESIAN_POINT('Ctrl Pts',(-0.20516615887642,0.0122991836084092,
-0.00895963048145717));
#41176=CARTESIAN_POINT('Ctrl Pts',(-0.205159163971388,0.012311149055828,
-0.008964037697506));
#41177=CARTESIAN_POINT('Ctrl Pts',(-0.205142860944653,0.0123353268288297,
-0.008967928075468));
#41178=CARTESIAN_POINT('Ctrl Pts',(-0.205134196499638,0.0123468070286007,
-0.00896764154323951));
#41179=CARTESIAN_POINT('Ctrl Pts',(-0.205114342718288,0.0123708879580858,
-0.00896315819011513));
#41180=CARTESIAN_POINT('Ctrl Pts',(-0.205104622989719,0.0123811700400964,
-0.00895847447913059));
#41181=CARTESIAN_POINT('Ctrl Pts',(-0.205097384650215,0.0123886506823329,
-0.00895436076088045));
#41182=CARTESIAN_POINT('Ctrl Pts',(-0.205095267860903,0.0123907425138203,
-0.00895318017659277));
#41183=CARTESIAN_POINT('Ctrl Pts',(-0.205093143040606,0.0123927769598421,
-0.00895191630922259));
#41184=CARTESIAN_POINT('Ctrl Pts',(-0.205092344163379,0.0123935584157556,
-0.00895141728292034));
#41185=CARTESIAN_POINT('Ctrl Pts',(-0.206144103513576,0.00802320152732896,
-0.0102507274525613));
#41186=CARTESIAN_POINT('Ctrl Pts',(-0.206140997950459,0.00802904586778321,
-0.010352306059325));
#41187=CARTESIAN_POINT('Ctrl Pts',(-0.206242434213696,0.00802058399184559,
-0.0103541294277887));
#41188=CARTESIAN_POINT('Ctrl Pts',(-0.206056579512448,0.00700735013193967,
-0.0103076580428027));
#41189=CARTESIAN_POINT('Ctrl Pts',(-0.206053450453671,0.00700175551739084,
-0.0104098901160137));
#41190=CARTESIAN_POINT('Ctrl Pts',(-0.206154656804463,0.00699109309901565,
-0.0104106529954126));
#41191=CARTESIAN_POINT('Ctrl Pts',(-0.205842609607531,0.00493647513741988,
-0.0100759677680453));
#41192=CARTESIAN_POINT('Ctrl Pts',(-0.205839605792459,0.00490826674460647,
-0.0101756783187804));
#41193=CARTESIAN_POINT('Ctrl Pts',(-0.205942200979761,0.00490877422186876,
-0.0101741790754591));
#41194=CARTESIAN_POINT('Ctrl Pts',(-0.206129004920361,0.00305341025745715,
-0.00918172589817647));
#41195=CARTESIAN_POINT('Ctrl Pts',(-0.206126357176411,0.00300405160961498,
-0.00927145037743672));
#41196=CARTESIAN_POINT('Ctrl Pts',(-0.206226999266609,0.00301755440218435,
-0.00927963958615716));
#41197=CARTESIAN_POINT('Ctrl Pts',(-0.206264033249047,0.0022273051379683,
-0.00860330356791341));
#41198=CARTESIAN_POINT('Ctrl Pts',(-0.206261626670221,0.00216894495741129,
-0.00868666242678945));
#41199=CARTESIAN_POINT('Ctrl Pts',(-0.206362612710959,0.00217897942055083,
-0.00869453476898776));
#41200=CARTESIAN_POINT('Ctrl Pts',(-0.206293209986791,0.00261116835746199,
-0.0089780881565586));
#41201=CARTESIAN_POINT('Ctrl Pts',(-0.206292152439964,0.00261196180857207,
-0.00897855861405994));
#41202=CARTESIAN_POINT('Ctrl Pts',(-0.206289430497985,0.00261397171563914,
-0.00897971274745204));
#41203=CARTESIAN_POINT('Ctrl Pts',(-0.206286715821411,0.00261604111206668,
-0.00898078772033416));
#41204=CARTESIAN_POINT('Ctrl Pts',(-0.206277145814662,0.00262362445694192,
-0.00898462953548511));
#41205=CARTESIAN_POINT('Ctrl Pts',(-0.206264610353204,0.0026338711059093,
-0.0089888332769248));
#41206=CARTESIAN_POINT('Ctrl Pts',(-0.206239352438,0.00265772908183957,
-0.00899237788634536));
#41207=CARTESIAN_POINT('Ctrl Pts',(-0.206228282712326,0.00266920622605173,
-0.00899231142454711));
#41208=CARTESIAN_POINT('Ctrl Pts',(-0.206207676314294,0.00269341580046527,
-0.0089876600294395));
#41209=CARTESIAN_POINT('Ctrl Pts',(-0.206198995732441,0.0027053325979369,
-0.0089829638682279));
#41210=CARTESIAN_POINT('Ctrl Pts',(-0.206188794293892,0.00272272036421045,
-0.00897206573525393));
#41211=CARTESIAN_POINT('Ctrl Pts',(-0.206185663094497,0.00272915354208732,
-0.00896697788736482));
#41212=CARTESIAN_POINT('Ctrl Pts',(-0.206181921166814,0.00274006870319551,
-0.00895577915139813));
#41213=CARTESIAN_POINT('Ctrl Pts',(-0.206181032892529,0.00274457413552852,
-0.00895008469635413));
#41214=CARTESIAN_POINT('Ctrl Pts',(-0.206181061337296,0.00274846569215316,
-0.00894387223338268));
#41215=CARTESIAN_POINT('Ctrl Pts',(-0.205142482088579,0.00699220996088759,
-0.0102293438807348));
#41216=CARTESIAN_POINT('Ctrl Pts',(-0.205140639337482,0.00698620356045466,
-0.0103359908107351));
#41217=CARTESIAN_POINT('Ctrl Pts',(-0.205034537097864,0.00697779962238244,
-0.0103265903532839));
#41218=CARTESIAN_POINT('Ctrl Pts',(-0.205055686601309,0.00801208405484312,
-0.0102842507443711));
#41219=CARTESIAN_POINT('Ctrl Pts',(-0.205053827163856,0.00801807257933057,
-0.0103915774312491));
#41220=CARTESIAN_POINT('Ctrl Pts',(-0.204947949614617,0.00800680784218544,
-0.0103831666819726));
#41221=CARTESIAN_POINT('Ctrl Pts',(-0.204846824706544,0.01006416746964,
-0.0100486295602955));
#41222=CARTESIAN_POINT('Ctrl Pts',(-0.204845062847581,0.0100937289998733,
-0.0101532635178354));
#41223=CARTESIAN_POINT('Ctrl Pts',(-0.204737712388477,0.0100917772942086,
-0.0101476164771957));
#41224=CARTESIAN_POINT('Ctrl Pts',(-0.205124477129889,0.0119248241379215,
-0.00917343580602142));
#41225=CARTESIAN_POINT('Ctrl Pts',(-0.20512312749823,0.011976373863991,
-0.00926778133092942));
#41226=CARTESIAN_POINT('Ctrl Pts',(-0.205017823077147,0.0119869252156459,
-0.00925255879414128));
#41227=CARTESIAN_POINT('Ctrl Pts',(-0.205262235724447,0.012760158868421,
-0.00859356109315354));
#41228=CARTESIAN_POINT('Ctrl Pts',(-0.205261132004666,0.0128212089278307,
-0.00868121456209581));
#41229=CARTESIAN_POINT('Ctrl Pts',(-0.205155466933443,0.0128274850701372,
-0.00866676438333058));
#41230=CARTESIAN_POINT('Ctrl Pts',(-0.205098440011371,0.00750015035561199,
-0.0102432542980132));
#41231=CARTESIAN_POINT('Ctrl Pts',(-0.205098278016604,0.00750015055076414,
-0.0102497158135366));
#41232=CARTESIAN_POINT('Ctrl Pts',(-0.205097487561935,0.00750015091686855,
-0.0102561461143775));
#41233=CARTESIAN_POINT('Ctrl Pts',(-0.205094563933792,0.00750015203413857,
-0.0102692494005583));
#41234=CARTESIAN_POINT('Ctrl Pts',(-0.205092340334007,0.00750015280942587,
-0.0102758660159279));
#41235=CARTESIAN_POINT('Ctrl Pts',(-0.205084090834935,0.00750015556900989,
-0.0102939134832974));
#41236=CARTESIAN_POINT('Ctrl Pts',(-0.205076518175416,0.0075001579817565,
-0.0103044814708938));
#41237=CARTESIAN_POINT('Ctrl Pts',(-0.205057781000493,0.00750016407237376,
-0.0103221751119802));
#41238=CARTESIAN_POINT('Ctrl Pts',(-0.205046790114734,0.00750016753939868,
-0.0103291339882119));
#41239=CARTESIAN_POINT('Ctrl Pts',(-0.205023489197286,0.00750017683211112,
-0.0103382475058349));
#41240=CARTESIAN_POINT('Ctrl Pts',(-0.205012454789772,0.00750016099293299,
-0.0103402131205683));
#41241=CARTESIAN_POINT('Ctrl Pts',(-0.205000340687757,0.00750021268667578,
-0.0103407434268609));
#41242=CARTESIAN_POINT('Ctrl Pts',(-0.204998015689761,0.00750017802011827,
-0.0103407682740367));
#41243=CARTESIAN_POINT('Ctrl Pts',(-0.204995840626232,0.00750017862353099,
-0.010340719315994));
#41244=CARTESIAN_POINT('Origin',(-0.20501976771991,0.00266278717579714,
-0.00886724406818112));
#41245=CARTESIAN_POINT('Ctrl Pts',(-0.205180471484369,0.00274828496058784,
-0.00892259092201156));
#41246=CARTESIAN_POINT('Ctrl Pts',(-0.205180344443188,0.00274423647563211,
-0.00892922577511845));
#41247=CARTESIAN_POINT('Ctrl Pts',(-0.205179425306355,0.0027394680149155,
-0.00893528377307584));
#41248=CARTESIAN_POINT('Ctrl Pts',(-0.20517595033189,0.00272816290128792,
-0.00894667609632815));
#41249=CARTESIAN_POINT('Ctrl Pts',(-0.205173267608394,0.00272163074259415,
-0.00895171169464386));
#41250=CARTESIAN_POINT('Ctrl Pts',(-0.205164629939474,0.00270387175476733,
-0.00896230741493743));
#41251=CARTESIAN_POINT('Ctrl Pts',(-0.205157518531435,0.00269181197528201,
-0.0089666338369735));
#41252=CARTESIAN_POINT('Ctrl Pts',(-0.205140876756943,0.00266732113900677,
-0.00897034072357252));
#41253=CARTESIAN_POINT('Ctrl Pts',(-0.205131972362909,0.00265562604229162,
-0.00896989952403503));
#41254=CARTESIAN_POINT('Ctrl Pts',(-0.205109001760081,0.00262806363961682,
-0.00896432066061317));
#41255=CARTESIAN_POINT('Ctrl Pts',(-0.205097770882948,0.00261689896753867,
-0.00895770506605427));
#41256=CARTESIAN_POINT('Ctrl Pts',(-0.205093772027569,0.00261306844039898,
-0.00895550370242417));
#41257=CARTESIAN_POINT('Ctrl Pts',(-0.205092571930731,0.00261162363512667,
-0.00895462460683516));
#41258=CARTESIAN_POINT('Ctrl Pts',(-0.205091223366067,0.00261030520999543,
-0.00895378355642604));
#41259=CARTESIAN_POINT('Ctrl Pts',(-0.205260955479136,0.00224264774500391,
-0.0085954366889458));
#41260=CARTESIAN_POINT('Ctrl Pts',(-0.20526001140994,0.00218180944454979,
-0.00868289007491256));
#41261=CARTESIAN_POINT('Ctrl Pts',(-0.205154592360999,0.00217532007259305,
-0.00866886906021484));
#41262=CARTESIAN_POINT('Ctrl Pts',(-0.205123528174581,0.00308109440095735,
-0.00917641256757719));
#41263=CARTESIAN_POINT('Ctrl Pts',(-0.205122337805058,0.00302977228761021,
-0.00927055314944947));
#41264=CARTESIAN_POINT('Ctrl Pts',(-0.205017275753863,0.00301909471955522,
-0.00925579939875452));
#41265=CARTESIAN_POINT('Ctrl Pts',(-0.20484613965658,0.00493748613428339,
-0.0100487096525008));
#41266=CARTESIAN_POINT('Ctrl Pts',(-0.204844542660311,0.0049080243327645,
-0.0101530627638109));
#41267=CARTESIAN_POINT('Ctrl Pts',(-0.204737444299667,0.00490974190000643,
-0.0101478430648011));
#41268=CARTESIAN_POINT('Ctrl Pts',(-0.205055811865902,0.00699451686999224,
-0.0102849389073442));
#41269=CARTESIAN_POINT('Ctrl Pts',(-0.205054115345084,0.00698860532580391,
-0.0103919880796032));
#41270=CARTESIAN_POINT('Ctrl Pts',(-0.204948496773928,0.00699993329614755,
-0.0103840506703114));
#41271=CARTESIAN_POINT('Ctrl Pts',(-0.205143562118305,0.00801654945543371,
-0.0102286679529194));
#41272=CARTESIAN_POINT('Ctrl Pts',(-0.205141882892494,0.00802262912478596,
-0.0103350243606254));
#41273=CARTESIAN_POINT('Ctrl Pts',(-0.20503603371479,0.00803106429285927,
-0.0103260782815921));
#41274=CARTESIAN_POINT('Ctrl Pts',(-0.208254443206528,0.0127067297690959,
-0.00868853043591179));
#41275=CARTESIAN_POINT('Ctrl Pts',(-0.208252817177365,0.0127639831859331,
-0.00877159573976323));
#41276=CARTESIAN_POINT('Ctrl Pts',(-0.208352886496751,0.0127538205857698,
-0.00877954740891872));
#41277=CARTESIAN_POINT('Ctrl Pts',(-0.208122153160708,0.0118948116780756,
-0.00924830039922951));
#41278=CARTESIAN_POINT('Ctrl Pts',(-0.208120294425605,0.0119432213060983,
-0.00933749997466366));
#41279=CARTESIAN_POINT('Ctrl Pts',(-0.208220100686766,0.0119302505900155,
-0.00934548024255124));
#41280=CARTESIAN_POINT('Ctrl Pts',(-0.207848482421744,0.0100670043687399,
-0.010110433671947));
#41281=CARTESIAN_POINT('Ctrl Pts',(-0.207846300193864,0.0100950982407419,
-0.0102091369504758));
#41282=CARTESIAN_POINT('Ctrl Pts',(-0.207947953070991,0.0100944347762669,
-0.0102079379981602));
#41283=CARTESIAN_POINT('Ctrl Pts',(-0.208049545050965,0.00805000192234531,
-0.0103475054232749));
#41284=CARTESIAN_POINT('Ctrl Pts',(-0.208047228055695,0.00805628014436581,
-0.0104487912651243));
#41285=CARTESIAN_POINT('Ctrl Pts',(-0.208147577167768,0.00806662809390711,
-0.0104495775820796));
#41286=CARTESIAN_POINT('Ctrl Pts',(-0.208136501793819,0.00706036444276593,
-0.0103009087163086));
#41287=CARTESIAN_POINT('Ctrl Pts',(-0.208134205125068,0.00705555198922157,
-0.0104016678523864));
#41288=CARTESIAN_POINT('Ctrl Pts',(-0.208234728401044,0.00706414444257922,
-0.0104034975501504));
#41289=CARTESIAN_POINT('Ctrl Pts',(-0.208097499489004,0.00749999845002932,
-0.0103107892565932));
#41290=CARTESIAN_POINT('Ctrl Pts',(-0.208097351583086,0.00749999854583129,
-0.0103173339068719));
#41291=CARTESIAN_POINT('Ctrl Pts',(-0.208097849227417,0.00749999849669942,
-0.0103238768584556));
#41292=CARTESIAN_POINT('Ctrl Pts',(-0.20810019278319,0.00749999810609638,
-0.0103371804420943));
#41293=CARTESIAN_POINT('Ctrl Pts',(-0.208102115735706,0.00749999774723053,
-0.0103438911809762));
#41294=CARTESIAN_POINT('Ctrl Pts',(-0.20810954331178,0.00749999630993762,
-0.0103622935486121));
#41295=CARTESIAN_POINT('Ctrl Pts',(-0.208116632253359,0.00749999488489928,
-0.0103731927605778));
#41296=CARTESIAN_POINT('Ctrl Pts',(-0.20813455402164,0.00749999139152034,
-0.0103917145053224));
#41297=CARTESIAN_POINT('Ctrl Pts',(-0.208145221004457,0.00749998925827104,
-0.0103991624716254));
#41298=CARTESIAN_POINT('Ctrl Pts',(-0.208167136994736,0.00749998606736913,
-0.0104088957045982));
#41299=CARTESIAN_POINT('Ctrl Pts',(-0.208177933625618,0.00749996906351887,
-0.0104116843695746));
#41300=CARTESIAN_POINT('Ctrl Pts',(-0.208191146848798,0.00749999943002881,
-0.0104128609239724));
#41301=CARTESIAN_POINT('Ctrl Pts',(-0.208193400306433,0.00749997664853401,
-0.0104129864827718));
#41302=CARTESIAN_POINT('Ctrl Pts',(-0.208195607948066,0.00749997611037837,
-0.0104130363984175));
#41303=CARTESIAN_POINT('Ctrl Pts',(-0.208182322531234,0.0122530850694677,
-0.00898281054933035));
#41304=CARTESIAN_POINT('Ctrl Pts',(-0.20818229260496,0.012257023594431,
-0.00898906876229917));
#41305=CARTESIAN_POINT('Ctrl Pts',(-0.208183195803744,0.0122615849103819,
-0.00899479795224621));
#41306=CARTESIAN_POINT('Ctrl Pts',(-0.208186999470675,0.0122726329544399,
-0.00900604646900106));
#41307=CARTESIAN_POINT('Ctrl Pts',(-0.208190181165405,0.0122791411220139,
-0.00901114196751426));
#41308=CARTESIAN_POINT('Ctrl Pts',(-0.208200508351318,0.0122966686441179,
-0.00902199162142199));
#41309=CARTESIAN_POINT('Ctrl Pts',(-0.208209267046805,0.0123086484551155,
-0.0090266281316795));
#41310=CARTESIAN_POINT('Ctrl Pts',(-0.208230283270831,0.0123332452203376,
-0.00903118464895189));
#41311=CARTESIAN_POINT('Ctrl Pts',(-0.208241733956362,0.0123450335003312,
-0.00903111298954677));
#41312=CARTESIAN_POINT('Ctrl Pts',(-0.208265092839061,0.0123668754193094,
-0.00902751311489447));
#41313=CARTESIAN_POINT('Ctrl Pts',(-0.208277074431209,0.0123772611298929,
-0.00902388967657451));
#41314=CARTESIAN_POINT('Ctrl Pts',(-0.208291136593539,0.0123877056522628,
-0.00901833269169697));
#41315=CARTESIAN_POINT('Ctrl Pts',(-0.208292766707618,0.012389140227029,
-0.00901750873668517));
#41316=CARTESIAN_POINT('Ctrl Pts',(-0.208294512702006,0.0123904475468134,
-0.00901672948361178));
#41317=CARTESIAN_POINT('Origin',(-0.208345496545884,0.0123375625807303,
-0.00893286285957864));
#41318=CARTESIAN_POINT('Ctrl Pts',(-0.207182081101986,0.0122534241571154,
-0.00896140352867932));
#41319=CARTESIAN_POINT('Ctrl Pts',(-0.207181956278481,0.0122574195556349,
-0.00896791580190798));
#41320=CARTESIAN_POINT('Ctrl Pts',(-0.207181066392585,0.012262110300776,
-0.0089738702636863));
#41321=CARTESIAN_POINT('Ctrl Pts',(-0.207177704706269,0.0122732045720034,
-0.0089850821673224));
#41322=CARTESIAN_POINT('Ctrl Pts',(-0.20717511169926,0.0122796037032122,
-0.00899005505969755));
#41323=CARTESIAN_POINT('Ctrl Pts',(-0.207166687657127,0.0122971375010644,
-0.00900065342756414));
#41324=CARTESIAN_POINT('Ctrl Pts',(-0.207159692854611,0.0123091105651382,
-0.00900503864248638));
#41325=CARTESIAN_POINT('Ctrl Pts',(-0.207143389299496,0.0123332953216799,
-0.00900888483866729));
#41326=CARTESIAN_POINT('Ctrl Pts',(-0.207134724148054,0.0123447752724386,
-0.00900857713229437));
#41327=CARTESIAN_POINT('Ctrl Pts',(-0.207114897742302,0.0123688127376833,
-0.00900405570779137));
#41328=CARTESIAN_POINT('Ctrl Pts',(-0.207105192569871,0.0123790762651988,
-0.00899937093567547));
#41329=CARTESIAN_POINT('Ctrl Pts',(-0.207097899951547,0.0123866015335837,
-0.00899521430276797));
#41330=CARTESIAN_POINT('Ctrl Pts',(-0.207095791256553,0.0123886836581939,
-0.00899403346105137));
#41331=CARTESIAN_POINT('Ctrl Pts',(-0.207093674671486,0.0123907089793412,
-0.0089927704541225));
#41332=CARTESIAN_POINT('Ctrl Pts',(-0.207092867603371,0.0123914974180721,
-0.0089922648645807));
#41333=CARTESIAN_POINT('Ctrl Pts',(-0.208143344830797,0.00801431535345852,
-0.0102963203625224));
#41334=CARTESIAN_POINT('Ctrl Pts',(-0.208140201657287,0.00802007540567886,
-0.010397751642749));
#41335=CARTESIAN_POINT('Ctrl Pts',(-0.208241474571592,0.00801153714660289,
-0.0103997680387923));
#41336=CARTESIAN_POINT('Ctrl Pts',(-0.208054400162267,0.00700150192641365,
-0.0103522839259218));
#41337=CARTESIAN_POINT('Ctrl Pts',(-0.208051234145549,0.00699583305844126,
-0.0104543596381036));
#41338=CARTESIAN_POINT('Ctrl Pts',(-0.208152281685006,0.00698503643943993,
-0.010455282128268));
#41339=CARTESIAN_POINT('Ctrl Pts',(-0.207845968693388,0.00497123137684409,
-0.0101233193244587));
#41340=CARTESIAN_POINT('Ctrl Pts',(-0.207842924905438,0.00494334863064471,
-0.0102228997512816));
#41341=CARTESIAN_POINT('Ctrl Pts',(-0.207945339089887,0.00494393007860572,
-0.0102217144919219));
#41342=CARTESIAN_POINT('Ctrl Pts',(-0.208120104371585,0.00312365367681334,
-0.00925598171762431));
#41343=CARTESIAN_POINT('Ctrl Pts',(-0.208117403181981,0.00307499116185933,
-0.00934585701471216));
#41344=CARTESIAN_POINT('Ctrl Pts',(-0.208217967734135,0.00308783281510984,
-0.00935385714742386));
#41345=CARTESIAN_POINT('Ctrl Pts',(-0.208250100050302,0.0023208742329109,
-0.00870641445993126));
#41346=CARTESIAN_POINT('Ctrl Pts',(-0.208247627110399,0.00226341898325691,
-0.00879022115099646));
#41347=CARTESIAN_POINT('Ctrl Pts',(-0.20834843066501,0.00227365595662788,
-0.0087982762741702));
#41348=CARTESIAN_POINT('Ctrl Pts',(-0.208294284391964,0.0026126423899481,
-0.00901864750601907));
#41349=CARTESIAN_POINT('Ctrl Pts',(-0.208293221456411,0.00261343900871228,
-0.00901912190356573));
#41350=CARTESIAN_POINT('Ctrl Pts',(-0.208290504841601,0.0026154435033703,
-0.00902027778717965));
#41351=CARTESIAN_POINT('Ctrl Pts',(-0.208287795713521,0.00261750700095301,
-0.00902135499508675));
#41352=CARTESIAN_POINT('Ctrl Pts',(-0.20827819847105,0.00262510339882467,
-0.00902522144578501));
#41353=CARTESIAN_POINT('Ctrl Pts',(-0.208265689525886,0.00263532392112371,
-0.00902943085794375));
#41354=CARTESIAN_POINT('Ctrl Pts',(-0.208240476225512,0.0026591282377444,
-0.00903302185679735));
#41355=CARTESIAN_POINT('Ctrl Pts',(-0.208229416121853,0.0026705920051928,
-0.0090329825727401));
#41356=CARTESIAN_POINT('Ctrl Pts',(-0.208208803468976,0.00269480468142731,
-0.00902839576330975));
#41357=CARTESIAN_POINT('Ctrl Pts',(-0.208200111195092,0.00270673906414479,
-0.00902372721040564));
#41358=CARTESIAN_POINT('Ctrl Pts',(-0.208189890950813,0.00272416595776656,
-0.00901286328082817));
#41359=CARTESIAN_POINT('Ctrl Pts',(-0.208186752219044,0.00273061869531979,
-0.00900778421126741));
#41360=CARTESIAN_POINT('Ctrl Pts',(-0.208183000720674,0.00274157311829964,
-0.008996593520968));
#41361=CARTESIAN_POINT('Ctrl Pts',(-0.208182110252984,0.00274609707774618,
-0.00899089919268803));
#41362=CARTESIAN_POINT('Ctrl Pts',(-0.208182139477677,0.00275000626856638,
-0.00898468398557736));
#41363=CARTESIAN_POINT('Ctrl Pts',(-0.207142447083897,0.006992183093808,
-0.0102750218786083));
#41364=CARTESIAN_POINT('Ctrl Pts',(-0.20714006707363,0.00698616230337856,
-0.0103806840105263));
#41365=CARTESIAN_POINT('Ctrl Pts',(-0.207034905932455,0.00697771837226714,
-0.0103717631079065));
#41366=CARTESIAN_POINT('Ctrl Pts',(-0.207054100312034,0.00801199116278463,
-0.01033007892178));
#41367=CARTESIAN_POINT('Ctrl Pts',(-0.207051705141398,0.00801788788449221,
-0.0104364247901112));
#41368=CARTESIAN_POINT('Ctrl Pts',(-0.206946768666599,0.00800656573091688,
-0.0104285255622565));
#41369=CARTESIAN_POINT('Ctrl Pts',(-0.20684533708077,0.0100638006421552,
-0.0100937633659248));
#41370=CARTESIAN_POINT('Ctrl Pts',(-0.206843030517134,0.0100931862263171,
-0.0101974378781082));
#41371=CARTESIAN_POINT('Ctrl Pts',(-0.206736620206684,0.010091652693392,
-0.0101921840430576));
#41372=CARTESIAN_POINT('Ctrl Pts',(-0.207125466271094,0.0119235866362789,
-0.00921573185060216));
#41373=CARTESIAN_POINT('Ctrl Pts',(-0.207123577691201,0.0119749030496809,
-0.00930908688655247));
#41374=CARTESIAN_POINT('Ctrl Pts',(-0.207019198536868,0.0119854727335022,
-0.00929435969050802));
#41375=CARTESIAN_POINT('Ctrl Pts',(-0.207262576286763,0.0127576794032243,
-0.00863412005073474));
#41376=CARTESIAN_POINT('Ctrl Pts',(-0.207260928577023,0.0128184051686157,
-0.00872080512210846));
#41377=CARTESIAN_POINT('Ctrl Pts',(-0.207156193086846,0.012824836055491,
-0.00870680606209627));
#41378=CARTESIAN_POINT('Ctrl Pts',(-0.207097778634823,0.0074999984041968,
-0.0102884291162079));
#41379=CARTESIAN_POINT('Ctrl Pts',(-0.207097617294887,0.00749999849305758,
-0.0102948949871889));
#41380=CARTESIAN_POINT('Ctrl Pts',(-0.207096826594071,0.00749999872193563,
-0.0103013296439083));
#41381=CARTESIAN_POINT('Ctrl Pts',(-0.20709390155598,0.00749999949493435,
-0.0103144375318467));
#41382=CARTESIAN_POINT('Ctrl Pts',(-0.207091677519774,0.00750000005938463,
-0.0103210545038764));
#41383=CARTESIAN_POINT('Ctrl Pts',(-0.207083426652751,0.00750000213865603,
-0.010339102345941));
#41384=CARTESIAN_POINT('Ctrl Pts',(-0.207075853009443,0.00750000401966211,
-0.0103496701497808));
#41385=CARTESIAN_POINT('Ctrl Pts',(-0.207057113766972,0.00750000895351662,
-0.0103673633379332));
#41386=CARTESIAN_POINT('Ctrl Pts',(-0.207046121745384,0.00750001179091493,
-0.010374321862266));
#41387=CARTESIAN_POINT('Ctrl Pts',(-0.207022667760621,0.00750002009313667,
-0.0103834937529816));
#41388=CARTESIAN_POINT('Ctrl Pts',(-0.207011610188164,0.007500002533942,
-0.010385407470795));
#41389=CARTESIAN_POINT('Ctrl Pts',(-0.206999679808045,0.00750005757307741,
-0.0103859295033157));
#41390=CARTESIAN_POINT('Ctrl Pts',(-0.206997334122852,0.00750001932399001,
-0.0103859545510466));
#41391=CARTESIAN_POINT('Ctrl Pts',(-0.206995169267356,0.00750001981683416,
-0.0103859057989294));
#41392=CARTESIAN_POINT('Origin',(-0.207020862424657,0.00266442695171015,
-0.0089078479286756));
#41393=CARTESIAN_POINT('Ctrl Pts',(-0.207181588037537,0.00274982395495244,
-0.00896336710976845));
#41394=CARTESIAN_POINT('Ctrl Pts',(-0.207181460885151,0.00274576262790076,
-0.00896999422727271));
#41395=CARTESIAN_POINT('Ctrl Pts',(-0.207180541651928,0.00274098238846861,
-0.00897604305378098));
#41396=CARTESIAN_POINT('Ctrl Pts',(-0.207177066510391,0.0027296549790865,
-0.00898741356184911));
#41397=CARTESIAN_POINT('Ctrl Pts',(-0.207174383711823,0.0027231128678696,
-0.00899243649753085));
#41398=CARTESIAN_POINT('Ctrl Pts',(-0.207165746028982,0.00270533301997872,
-0.00900299747571993));
#41399=CARTESIAN_POINT('Ctrl Pts',(-0.207158634768288,0.0026932646575399,
-0.00900730024230634));
#41400=CARTESIAN_POINT('Ctrl Pts',(-0.207142021128562,0.00266880706469116,
-0.00901095287902417));
#41401=CARTESIAN_POINT('Ctrl Pts',(-0.207133150573149,0.0026571524192198,
-0.00901049789236432));
#41402=CARTESIAN_POINT('Ctrl Pts',(-0.207115076418399,0.00263545890743936,
-0.00900608900771923));
#41403=CARTESIAN_POINT('Ctrl Pts',(-0.207105920485487,0.00262514686178307,
-0.0090021126094672));
#41404=CARTESIAN_POINT('Ctrl Pts',(-0.207095016218406,0.00261465333045586,
-0.008996083770829));
#41405=CARTESIAN_POINT('Ctrl Pts',(-0.207093747453505,0.00261315504859148,
-0.00899517016771365));
#41406=CARTESIAN_POINT('Ctrl Pts',(-0.207092338322616,0.00261177910282465,
-0.00899428861609635));
#41407=CARTESIAN_POINT('Ctrl Pts',(-0.207261911557155,0.00224487504033121,
-0.00863509602890071));
#41408=CARTESIAN_POINT('Ctrl Pts',(-0.207261061333487,0.00218403251266008,
-0.00872217940345594));
#41409=CARTESIAN_POINT('Ctrl Pts',(-0.207155912480172,0.0021773545685175,
-0.00870850348120737));
#41410=CARTESIAN_POINT('Ctrl Pts',(-0.20712510668135,0.00308209641683207,
-0.0092178996899935));
#41411=CARTESIAN_POINT('Ctrl Pts',(-0.20712401154892,0.00303076155080782,
-0.0093116937851499));
#41412=CARTESIAN_POINT('Ctrl Pts',(-0.20701921751319,0.0030200107749622,
-0.00929732600181945));
#41413=CARTESIAN_POINT('Ctrl Pts',(-0.206845115742223,0.00493737975183436,
-0.0100931217449419));
#41414=CARTESIAN_POINT('Ctrl Pts',(-0.206843618048967,0.00490790247082884,
-0.0101971639881759));
#41415=CARTESIAN_POINT('Ctrl Pts',(-0.206736790651225,0.00490918313827814,
-0.0101922763693325));
#41416=CARTESIAN_POINT('Ctrl Pts',(-0.207054261772577,0.0069945228288837,
-0.0103301552766145));
#41417=CARTESIAN_POINT('Ctrl Pts',(-0.207052663899309,0.00698859617030293,
-0.0104369057642559));
#41418=CARTESIAN_POINT('Ctrl Pts',(-0.206947324401705,0.00700004890355841,
-0.0104294130005563));
#41419=CARTESIAN_POINT('Ctrl Pts',(-0.207143517855953,0.00801628664541418,
-0.0102737391026986));
#41420=CARTESIAN_POINT('Ctrl Pts',(-0.207141937229774,0.0080223612876047,
-0.0103797952379834));
#41421=CARTESIAN_POINT('Ctrl Pts',(-0.207036365988693,0.00803087655515608,
-0.0103712544502575));
#41422=CARTESIAN_POINT('Ctrl Pts',(-0.210235470212884,0.0125831962427011,
-0.00881114272403701));
#41423=CARTESIAN_POINT('Ctrl Pts',(-0.210233811792169,0.0126392072517556,
-0.00889487396476536));
#41424=CARTESIAN_POINT('Ctrl Pts',(-0.210333701636679,0.0126288133946314,
-0.00890292617772176));
#41425=CARTESIAN_POINT('Ctrl Pts',(-0.210109914640351,0.0118029254008048,
-0.00933261880976109));
#41426=CARTESIAN_POINT('Ctrl Pts',(-0.210108040881823,0.0118503934809046,
-0.00942208249800212));
#41427=CARTESIAN_POINT('Ctrl Pts',(-0.2102077892993,0.0118381776955304,
-0.00942974108211226));
#41428=CARTESIAN_POINT('Ctrl Pts',(-0.209858863349157,0.0100626309432614,
-0.0101397859379606));
#41429=CARTESIAN_POINT('Ctrl Pts',(-0.209856688792772,0.0100907353699573,
-0.010238163383176));
#41430=CARTESIAN_POINT('Ctrl Pts',(-0.209958115064439,0.0100898245173313,
-0.0102374345613252));
#41431=CARTESIAN_POINT('Ctrl Pts',(-0.210038384794055,0.00814902869092786,
-0.0103806956142887));
#41432=CARTESIAN_POINT('Ctrl Pts',(-0.210036077908365,0.00815640672945998,
-0.0104816997027483));
#41433=CARTESIAN_POINT('Ctrl Pts',(-0.210136329087176,0.00816633140866834,
-0.0104825258559512));
#41434=CARTESIAN_POINT('Ctrl Pts',(-0.210123208037224,0.00720701508233023,
-0.0103517770571818));
#41435=CARTESIAN_POINT('Ctrl Pts',(-0.210120913424717,0.00720383758858374,
-0.0104524503373305));
#41436=CARTESIAN_POINT('Ctrl Pts',(-0.21022125585175,0.0072127173421066,
-0.0104542782118082));
#41437=CARTESIAN_POINT('Ctrl Pts',(-0.210096834544416,0.00749994081583322,
-0.0103559757400411));
#41438=CARTESIAN_POINT('Ctrl Pts',(-0.210096686633433,0.00749994088263926,
-0.0103625206548424));
#41439=CARTESIAN_POINT('Ctrl Pts',(-0.210097184378745,0.00749994083320546,
-0.0103690638608643));
#41440=CARTESIAN_POINT('Ctrl Pts',(-0.210099528352888,0.00749994050181511,
-0.0103823679829186));
#41441=CARTESIAN_POINT('Ctrl Pts',(-0.21010145164146,0.00749994020608678,
-0.0103890789745933));
#41442=CARTESIAN_POINT('Ctrl Pts',(-0.21010888034258,0.0074999390400106,
-0.0104074816985564));
#41443=CARTESIAN_POINT('Ctrl Pts',(-0.210115970160806,0.00749993789742544,
-0.0104183808246853));
#41444=CARTESIAN_POINT('Ctrl Pts',(-0.210133893814439,0.00749993516413654,
-0.0104369023611447));
#41445=CARTESIAN_POINT('Ctrl Pts',(-0.210144561863844,0.0074999334935551,
-0.0104443501210892));
#41446=CARTESIAN_POINT('Ctrl Pts',(-0.210166481412328,0.00749993137224817,
-0.0104540837252773));
#41447=CARTESIAN_POINT('Ctrl Pts',(-0.210177278352322,0.00749991366139868,
-0.0104568712710575));
#41448=CARTESIAN_POINT('Ctrl Pts',(-0.210190485815975,0.00749994729335911,
-0.0104580473756483));
#41449=CARTESIAN_POINT('Ctrl Pts',(-0.210192746196891,0.00749992280800758,
-0.0104581733219418));
#41450=CARTESIAN_POINT('Ctrl Pts',(-0.210194950898968,0.00749992236667074,
-0.0104582231832109));
#41451=CARTESIAN_POINT('Ctrl Pts',(-0.210183035273252,0.0122509820678714,
-0.00902403648976699));
#41452=CARTESIAN_POINT('Ctrl Pts',(-0.210183004474919,0.0122549334919774,
-0.00903029130710398));
#41453=CARTESIAN_POINT('Ctrl Pts',(-0.210183907816865,0.0122595072821419,
-0.00903601560526435));
#41454=CARTESIAN_POINT('Ctrl Pts',(-0.210187712856156,0.0122705785956896,
-0.00904724790522209));
#41455=CARTESIAN_POINT('Ctrl Pts',(-0.210190895163352,0.0122770963799046,
-0.00905233251787761));
#41456=CARTESIAN_POINT('Ctrl Pts',(-0.210201224090118,0.0122946438148163,
-0.00906315213064524));
#41457=CARTESIAN_POINT('Ctrl Pts',(-0.210209983860423,0.0123066314588125,
-0.0090677677614427));
#41458=CARTESIAN_POINT('Ctrl Pts',(-0.210231026129084,0.0123312626491986,
-0.00907228628335188));
#41459=CARTESIAN_POINT('Ctrl Pts',(-0.210242507315303,0.01234307663651,
-0.00907218824628096));
#41460=CARTESIAN_POINT('Ctrl Pts',(-0.210272325114507,0.012370930810171,
-0.0090675228065052));
#41461=CARTESIAN_POINT('Ctrl Pts',(-0.210287216580575,0.0123822262288944,
-0.00906117162122654));
#41462=CARTESIAN_POINT('Ctrl Pts',(-0.210291961848719,0.0123857329846465,
-0.00905929124963881));
#41463=CARTESIAN_POINT('Ctrl Pts',(-0.21029352851447,0.0123871255042076,
-0.00905848601124937));
#41464=CARTESIAN_POINT('Ctrl Pts',(-0.210295216002383,0.012388387453904,
-0.00905773072421305));
#41465=CARTESIAN_POINT('Origin',(-0.210345973362526,0.0123353396224193,
-0.00897396358652427));
#41466=CARTESIAN_POINT('Ctrl Pts',(-0.209182549309909,0.0122515014451553,
-0.00900247968906914));
#41467=CARTESIAN_POINT('Ctrl Pts',(-0.209182424357049,0.0122555091588162,
-0.00900898508945461));
#41468=CARTESIAN_POINT('Ctrl Pts',(-0.209181534228362,0.0122602114412656,
-0.00901493115388496));
#41469=CARTESIAN_POINT('Ctrl Pts',(-0.209178171837601,0.0122713281354332,
-0.00902612282222287));
#41470=CARTESIAN_POINT('Ctrl Pts',(-0.209175578325821,0.0122777376353018,
-0.00903108372130858));
#41471=CARTESIAN_POINT('Ctrl Pts',(-0.209167153320636,0.012295293505668,
-0.00904164807624254));
#41472=CARTESIAN_POINT('Ctrl Pts',(-0.20916015810978,0.0123072763124866,
-0.00904600973000227));
#41473=CARTESIAN_POINT('Ctrl Pts',(-0.209143853782949,0.0123314717979331,
-0.00904980789329348));
#41474=CARTESIAN_POINT('Ctrl Pts',(-0.209135188499717,0.0123429527526135,
-0.00904947723024575));
#41475=CARTESIAN_POINT('Ctrl Pts',(-0.209115354906058,0.0123669938598687,
-0.00904490615931702));
#41476=CARTESIAN_POINT('Ctrl Pts',(-0.209105645668148,0.0123772529746108,
-0.00904019631515971));
#41477=CARTESIAN_POINT('Ctrl Pts',(-0.209098365777995,0.0123847593086512,
-0.00903603151450798));
#41478=CARTESIAN_POINT('Ctrl Pts',(-0.209096254901744,0.012386841541812,
-0.00903484552833635));
#41479=CARTESIAN_POINT('Ctrl Pts',(-0.209094136097871,0.0123888666300359,
-0.00903357723246944));
#41480=CARTESIAN_POINT('Ctrl Pts',(-0.209093330965559,0.0123896523666189,
-0.00903307128651946));
#41481=CARTESIAN_POINT('Ctrl Pts',(-0.210122790867358,0.00778687461044981,
-0.010351991928395));
#41482=CARTESIAN_POINT('Ctrl Pts',(-0.210120509030329,0.00778997965051194,
-0.0104525808922906));
#41483=CARTESIAN_POINT('Ctrl Pts',(-0.210220759666774,0.00778106815290546,
-0.0104544784162097));
#41484=CARTESIAN_POINT('Ctrl Pts',(-0.21003771958249,0.00684739648040692,
-0.0103800502715855));
#41485=CARTESIAN_POINT('Ctrl Pts',(-0.210035425847737,0.00683998407859043,
-0.0104809600904831));
#41486=CARTESIAN_POINT('Ctrl Pts',(-0.210135588276038,0.00683002917116009,
-0.0104818514875396));
#41487=CARTESIAN_POINT('Ctrl Pts',(-0.209859680423329,0.00494226274913538,
-0.0101407557752523));
#41488=CARTESIAN_POINT('Ctrl Pts',(-0.209857518240127,0.00491423839445973,
-0.0102390594248941));
#41489=CARTESIAN_POINT('Ctrl Pts',(-0.209958850344826,0.00491528136435581,
-0.0102384592310678));
#41490=CARTESIAN_POINT('Ctrl Pts',(-0.210110442658573,0.00320097165849752,
-0.00933430005928662));
#41491=CARTESIAN_POINT('Ctrl Pts',(-0.210108580826121,0.00315358902991755,
-0.00942370536723907));
#41492=CARTESIAN_POINT('Ctrl Pts',(-0.210208251154881,0.00316568454937026,
-0.00943138424087661));
#41493=CARTESIAN_POINT('Ctrl Pts',(-0.210234851606964,0.00242463804919971,
-0.00881636542139056));
#41494=CARTESIAN_POINT('Ctrl Pts',(-0.210233203468192,0.0023687621720114,
-0.00890008212730693));
#41495=CARTESIAN_POINT('Ctrl Pts',(-0.210333010304818,0.00237908946436521,
-0.00890816439708428));
#41496=CARTESIAN_POINT('Ctrl Pts',(-0.210295598600257,0.00261401462196279,
-0.0090592390136268));
#41497=CARTESIAN_POINT('Ctrl Pts',(-0.210294527757695,0.00261481630216766,
-0.00905971848287953));
#41498=CARTESIAN_POINT('Ctrl Pts',(-0.210291818773028,0.00261681405859242,
-0.0090608751759147));
#41499=CARTESIAN_POINT('Ctrl Pts',(-0.210289117458866,0.00261887013661076,
-0.00906195389803063));
#41500=CARTESIAN_POINT('Ctrl Pts',(-0.210279475839446,0.00262649256331565,
-0.0090658514781019));
#41501=CARTESIAN_POINT('Ctrl Pts',(-0.210266998510554,0.00263668469064512,
-0.00907006215183289));
#41502=CARTESIAN_POINT('Ctrl Pts',(-0.210241838214722,0.00266042729560625,
-0.00907369833425217));
#41503=CARTESIAN_POINT('Ctrl Pts',(-0.210230787403518,0.00267187783814618,
-0.00907368640849252));
#41504=CARTESIAN_POINT('Ctrl Pts',(-0.210210167289941,0.00269609427310657,
-0.00906916472948773));
#41505=CARTESIAN_POINT('Ctrl Pts',(-0.210201462620991,0.00270804669853119,
-0.00906452399287538));
#41506=CARTESIAN_POINT('Ctrl Pts',(-0.210191222605049,0.00272551333019873,
-0.00905369442458548));
#41507=CARTESIAN_POINT('Ctrl Pts',(-0.210188075958288,0.00273198594347644,
-0.00904862407492236));
#41508=CARTESIAN_POINT('Ctrl Pts',(-0.210184314434985,0.00274298004307225,
-0.009037441123476));
#41509=CARTESIAN_POINT('Ctrl Pts',(-0.21018342165608,0.00274752263533853,
-0.00903174675206267));
#41510=CARTESIAN_POINT('Ctrl Pts',(-0.210183451653278,0.00275144948649388,
-0.00902552855343153));
#41511=CARTESIAN_POINT('Ctrl Pts',(-0.209142530989361,0.00699231287835271,
-0.0103201859233318));
#41512=CARTESIAN_POINT('Ctrl Pts',(-0.209140159029996,0.00698629063188217,
-0.0104254976026752));
#41513=CARTESIAN_POINT('Ctrl Pts',(-0.209035328768285,0.00697775411075113,
-0.0104169399852814));
#41514=CARTESIAN_POINT('Ctrl Pts',(-0.209052501584123,0.00801199897977874,
-0.0103753688499246));
#41515=CARTESIAN_POINT('Ctrl Pts',(-0.209050114754894,0.00801789659276563,
-0.0104813665305186));
#41516=CARTESIAN_POINT('Ctrl Pts',(-0.208945510592866,0.0080064387339923,
-0.0104738696299997));
#41517=CARTESIAN_POINT('Ctrl Pts',(-0.208843911922949,0.0100634291810789,
-0.0101383603557189));
#41518=CARTESIAN_POINT('Ctrl Pts',(-0.208841612864033,0.010092810496628,
-0.0102416789156079));
#41519=CARTESIAN_POINT('Ctrl Pts',(-0.208735524411325,0.0100916723284601,
-0.0102367238690831));
#41520=CARTESIAN_POINT('Ctrl Pts',(-0.20912641034549,0.0119222931217929,
-0.00925753171213683));
#41521=CARTESIAN_POINT('Ctrl Pts',(-0.209124526741439,0.011973601805003,
-0.00935049411365509));
#41522=CARTESIAN_POINT('Ctrl Pts',(-0.209020465657013,0.011984218099799,
-0.00933612171575852));
#41523=CARTESIAN_POINT('Ctrl Pts',(-0.209262852149274,0.012755138999478,
-0.00867419623553459));
#41524=CARTESIAN_POINT('Ctrl Pts',(-0.209261207617309,0.0128158403474571,
-0.00876047032963096));
#41525=CARTESIAN_POINT('Ctrl Pts',(-0.209156792369228,0.0128224261641587,
-0.00874678973944371));
#41526=CARTESIAN_POINT('Ctrl Pts',(-0.209097174394345,0.00749996481452615,
-0.0103336053964147));
#41527=CARTESIAN_POINT('Ctrl Pts',(-0.209097013698476,0.00749996488422219,
-0.0103400756121614));
#41528=CARTESIAN_POINT('Ctrl Pts',(-0.209096222734907,0.00749996508674242,
-0.0103465146116718));
#41529=CARTESIAN_POINT('Ctrl Pts',(-0.209093296226861,0.00749996579190134,
-0.0103596271412186));
#41530=CARTESIAN_POINT('Ctrl Pts',(-0.209091071696894,0.00749996631386664,
-0.0103662445158202));
#41531=CARTESIAN_POINT('Ctrl Pts',(-0.209082819281554,0.00749996825608746,
-0.0103842927814137));
#41532=CARTESIAN_POINT('Ctrl Pts',(-0.209075244524087,0.00749997002888941,
-0.0103948603774847));
#41533=CARTESIAN_POINT('Ctrl Pts',(-0.209056502939813,0.00749997474929252,
-0.0104125530535077));
#41534=CARTESIAN_POINT('Ctrl Pts',(-0.209045509631471,0.00749997746681514,
-0.0104195111797564));
#41535=CARTESIAN_POINT('Ctrl Pts',(-0.209021616726638,0.00749998590382376,
-0.0104288529900601));
#41536=CARTESIAN_POINT('Ctrl Pts',(-0.20901043096659,0.00749996892955642,
-0.0104306201858471));
#41537=CARTESIAN_POINT('Ctrl Pts',(-0.208999076760909,0.00750002603475989,
-0.0104311167615857));
#41538=CARTESIAN_POINT('Ctrl Pts',(-0.208996706540869,0.00749998403251248,
-0.010431142048249));
#41539=CARTESIAN_POINT('Ctrl Pts',(-0.208994553794872,0.00749998449679488,
-0.0104310935426435));
#41540=CARTESIAN_POINT('Origin',(-0.209022200231755,0.00266602605730765,
-0.00894852322668744));
#41541=CARTESIAN_POINT('Ctrl Pts',(-0.209182662289348,0.00275131519549864,
-0.00900420129328437));
#41542=CARTESIAN_POINT('Ctrl Pts',(-0.209182535027075,0.00274724125113172,
-0.00901082072251512));
#41543=CARTESIAN_POINT('Ctrl Pts',(-0.209181615672769,0.00274244949160901,
-0.00901686048171236));
#41544=CARTESIAN_POINT('Ctrl Pts',(-0.209178140260104,0.00273110039458304,
-0.00902820949029176));
#41545=CARTESIAN_POINT('Ctrl Pts',(-0.209175457304311,0.00272454867617604,
-0.00903321999133582));
#41546=CARTESIAN_POINT('Ctrl Pts',(-0.209166819295205,0.00270674881741965,
-0.00904374696922658));
#41547=CARTESIAN_POINT('Ctrl Pts',(-0.209159707896966,0.00269467240680358,
-0.00904802664813589));
#41548=CARTESIAN_POINT('Ctrl Pts',(-0.209143133038255,0.00267026580891761,
-0.00905162397869498));
#41549=CARTESIAN_POINT('Ctrl Pts',(-0.209134309594035,0.00265866825396765,
-0.00905115969568957));
#41550=CARTESIAN_POINT('Ctrl Pts',(-0.209112873661121,0.00263292743671442,
-0.00904592097808777));
#41551=CARTESIAN_POINT('Ctrl Pts',(-0.209102711421051,0.00262248317195225,
-0.00904033396457725));
#41552=CARTESIAN_POINT('Ctrl Pts',(-0.209096266044791,0.00261624347336712,
-0.0090367573419262));
#41553=CARTESIAN_POINT('Ctrl Pts',(-0.209094901489963,0.00261466852848538,
-0.00903579591927314));
#41554=CARTESIAN_POINT('Ctrl Pts',(-0.209093406978092,0.0026132111295408,
-0.00903485819588743));
#41555=CARTESIAN_POINT('Ctrl Pts',(-0.209262801112433,0.00224697126424917,
-0.00867490866995627));
#41556=CARTESIAN_POINT('Ctrl Pts',(-0.209261929283104,0.00218608218935967,
-0.00876166481462779));
#41557=CARTESIAN_POINT('Ctrl Pts',(-0.20915700285995,0.00217931463768635,
-0.00874818364093454));
#41558=CARTESIAN_POINT('Ctrl Pts',(-0.20912666223509,0.00308301714484159,
-0.00925954111540404));
#41559=CARTESIAN_POINT('Ctrl Pts',(-0.209125547091583,0.00303162849784595,
-0.0093530344837294));
#41560=CARTESIAN_POINT('Ctrl Pts',(-0.209020973849429,0.00302089220559985,
-0.00933889224512626));
#41561=CARTESIAN_POINT('Ctrl Pts',(-0.20884410193955,0.00493732213256617,
-0.0101376857974969));
#41562=CARTESIAN_POINT('Ctrl Pts',(-0.20884258581963,0.00490781537082798,
-0.0102414789789533));
#41563=CARTESIAN_POINT('Ctrl Pts',(-0.208735982101809,0.00490868367757524,
-0.0102367410833359));
#41564=CARTESIAN_POINT('Ctrl Pts',(-0.209052616298212,0.00699464150726956,
-0.0103754833052408));
#41565=CARTESIAN_POINT('Ctrl Pts',(-0.209051000912337,0.0069887103865453,
-0.0104819951718267));
#41566=CARTESIAN_POINT('Ctrl Pts',(-0.208945896242155,0.00700032634036486,
-0.0104747676946981));
#41567=CARTESIAN_POINT('Ctrl Pts',(-0.209143633401348,0.00801615107495887,
-0.0103189165970082));
#41568=CARTESIAN_POINT('Ctrl Pts',(-0.209142034971987,0.00802223475741889,
-0.010424730840755));
#41569=CARTESIAN_POINT('Ctrl Pts',(-0.209036696922337,0.00803083836422602,
-0.0104164124237201));
#41570=CARTESIAN_POINT('Ctrl Pts',(-0.194260566397066,0.0127940739393323,
-0.00836181481645916));
#41571=CARTESIAN_POINT('Ctrl Pts',(-0.194258157740366,0.0128520362452587,
-0.00844683908739088));
#41572=CARTESIAN_POINT('Ctrl Pts',(-0.19436029261288,0.0128412877828854,
-0.00845361523486277));
#41573=CARTESIAN_POINT('Ctrl Pts',(-0.194124314813594,0.0119569377977277,
-0.00893191938984265));
#41574=CARTESIAN_POINT('Ctrl Pts',(-0.194121655647109,0.0120058535938877,
-0.00902316064089455));
#41575=CARTESIAN_POINT('Ctrl Pts',(-0.194223452297076,0.0119915226494169,
-0.00903023491578875));
#41576=CARTESIAN_POINT('Ctrl Pts',(-0.193851105984685,0.0100693098681627,
-0.0098070233056107));
#41577=CARTESIAN_POINT('Ctrl Pts',(-0.193848076892825,0.010097302393308,
-0.00990791370737201));
#41578=CARTESIAN_POINT('Ctrl Pts',(-0.193951811020719,0.0100975879788375,
-0.00990507857556678));
#41579=CARTESIAN_POINT('Ctrl Pts',(-0.194064486196732,0.00799786398926628,
-0.0100356162055956));
#41580=CARTESIAN_POINT('Ctrl Pts',(-0.194061330849289,0.00800343965044749,
-0.0101389739286565));
#41581=CARTESIAN_POINT('Ctrl Pts',(-0.194163719819071,0.00801353727066376,
-0.0101386725304691));
#41582=CARTESIAN_POINT('Ctrl Pts',(-0.194147069647878,0.00697986904195666,
-0.00998010224803608));
#41583=CARTESIAN_POINT('Ctrl Pts',(-0.19414393857776,0.00697412920907708,
-0.0100828290181077));
#41584=CARTESIAN_POINT('Ctrl Pts',(-0.194246550098368,0.00698246049660227,
-0.0100834655870346));
#41585=CARTESIAN_POINT('Ctrl Pts',(-0.194103280095705,0.00750354479393001,
-0.00999450817382853));
#41586=CARTESIAN_POINT('Ctrl Pts',(-0.194103132213932,0.0075035473081524,
-0.0100010515017158));
#41587=CARTESIAN_POINT('Ctrl Pts',(-0.194103629370271,0.007503550039466,
-0.0100075931783246));
#41588=CARTESIAN_POINT('Ctrl Pts',(-0.194105970904067,0.00750355604164788,
-0.0100208940754098));
#41589=CARTESIAN_POINT('Ctrl Pts',(-0.194107892233365,0.00750355931897568,
-0.0100276035503664));
#41590=CARTESIAN_POINT('Ctrl Pts',(-0.194115314414744,0.0075035690321051,
-0.0100460041977227));
#41591=CARTESIAN_POINT('Ctrl Pts',(-0.194122399194833,0.00750357569145501,
-0.0100569038408753));
#41592=CARTESIAN_POINT('Ctrl Pts',(-0.19414031206282,0.00750358897799523,
-0.010075426673766));
#41593=CARTESIAN_POINT('Ctrl Pts',(-0.194150974046746,0.00750359548610248,
-0.010082875676867));
#41594=CARTESIAN_POINT('Ctrl Pts',(-0.194174603735767,0.00750360748583984,
-0.0100933762285736));
#41595=CARTESIAN_POINT('Ctrl Pts',(-0.194187730336832,0.00750377794946251,
-0.0100963594926318));
#41596=CARTESIAN_POINT('Ctrl Pts',(-0.194200912520396,0.00750360613312389,
-0.0100967433641591));
#41597=CARTESIAN_POINT('Ctrl Pts',(-0.194201350069792,0.00750361803291018,
-0.0100967539594273));
#41598=CARTESIAN_POINT('Ctrl Pts',(-0.194177780472304,0.0122674979892277,
-0.00869700656513734));
#41599=CARTESIAN_POINT('Ctrl Pts',(-0.194177756405024,0.0122713482585029,
-0.00870330565303864));
#41600=CARTESIAN_POINT('Ctrl Pts',(-0.194178660379777,0.0122758265372359,
-0.00870908561487317));
#41601=CARTESIAN_POINT('Ctrl Pts',(-0.194182462390553,0.012286723987401,
-0.00872048033693503));
#41602=CARTESIAN_POINT('Ctrl Pts',(-0.194185646336855,0.0122931733460766,
-0.00872566746126095));
#41603=CARTESIAN_POINT('Ctrl Pts',(-0.194195975107812,0.0123105730084261,
-0.00873675093606282));
#41604=CARTESIAN_POINT('Ctrl Pts',(-0.194204729183099,0.0123224980676776,
-0.00874154210222169));
#41605=CARTESIAN_POINT('Ctrl Pts',(-0.194226094161862,0.0123474717938464,
-0.00874649591046643));
#41606=CARTESIAN_POINT('Ctrl Pts',(-0.194237980625125,0.0123596746544839,
-0.00874649211843202));
#41607=CARTESIAN_POINT('Ctrl Pts',(-0.194268231716554,0.0123878641057918,
-0.00874186420697733));
#41608=CARTESIAN_POINT('Ctrl Pts',(-0.194283072567502,0.0123993606550317,
-0.00873548089790034));
#41609=CARTESIAN_POINT('Ctrl Pts',(-0.194287649953457,0.0124023998296309,
-0.00873384454996397));
#41610=CARTESIAN_POINT('Ctrl Pts',(-0.194288254848304,0.0124030132709194,
-0.00873349488248058));
#41611=CARTESIAN_POINT('Ctrl Pts',(-0.194289068674857,0.0124038353634868,
-0.00873302410067472));
#41612=CARTESIAN_POINT('Ctrl Pts',(-0.194289765313071,0.0124043621676603,
-0.00873271973491913));
#41613=CARTESIAN_POINT('Origin',(-0.194340688401695,0.0123526500534516,
-0.00864811707722939));
#41614=CARTESIAN_POINT('Ctrl Pts',(-0.193177319689981,0.0122679027418712,
-0.00867581562949272));
#41615=CARTESIAN_POINT('Ctrl Pts',(-0.193177195620142,0.0122718100036639,
-0.0086823850364032));
#41616=CARTESIAN_POINT('Ctrl Pts',(-0.193176303901968,0.0122764204768761,
-0.00868840561290754));
#41617=CARTESIAN_POINT('Ctrl Pts',(-0.193172933398585,0.0122873646022273,
-0.00869977330013174));
#41618=CARTESIAN_POINT('Ctrl Pts',(-0.19317033287057,0.0122936974996128,
-0.00870483499014074));
#41619=CARTESIAN_POINT('Ctrl Pts',(-0.193161886206775,0.0123110865119641,
-0.00871567327260089));
#41620=CARTESIAN_POINT('Ctrl Pts',(-0.193154873080797,0.0123229982296,-0.00872022208136985));
#41621=CARTESIAN_POINT('Ctrl Pts',(-0.193138530834182,0.0123471213424915,
-0.00872439825343486));
#41622=CARTESIAN_POINT('Ctrl Pts',(-0.193129848577642,0.0123585969399349,
-0.00872424886387294));
#41623=CARTESIAN_POINT('Ctrl Pts',(-0.193109605516503,0.0123831387994624,
-0.00871998396816283));
#41624=CARTESIAN_POINT('Ctrl Pts',(-0.193099863516187,0.0123934072473534,
-0.008715308331385));
#41625=CARTESIAN_POINT('Ctrl Pts',(-0.193093015200619,0.0124005273651118,
-0.00871150359471354));
#41626=CARTESIAN_POINT('Ctrl Pts',(-0.193090844328643,0.0124026776594429,
-0.00871032730139874));
#41627=CARTESIAN_POINT('Ctrl Pts',(-0.193088664937624,0.0124047671675376,
-0.00870906101126539));
#41628=CARTESIAN_POINT('Ctrl Pts',(-0.19308791289601,0.0124055064406691,
-0.00870860142875256));
#41629=CARTESIAN_POINT('Ctrl Pts',(-0.194360584264707,0.0021615829798264,
-0.00845557112034835));
#41630=CARTESIAN_POINT('Ctrl Pts',(-0.194258178150358,0.00215079489622151,
-0.00844888158936903));
#41631=CARTESIAN_POINT('Ctrl Pts',(-0.19426077173291,0.00220889260676681,
-0.00836363109027858));
#41632=CARTESIAN_POINT('Ctrl Pts',(-0.194224163205224,0.00301216227742662,
-0.00903230161285869));
#41633=CARTESIAN_POINT('Ctrl Pts',(-0.194122092678868,0.00299780557649061,
-0.00902532321450204));
#41634=CARTESIAN_POINT('Ctrl Pts',(-0.194124936884012,0.00304683006696333,
-0.00893383915952295));
#41635=CARTESIAN_POINT('Ctrl Pts',(-0.193953562027494,0.00490777775727108,
-0.00990682227567009));
#41636=CARTESIAN_POINT('Ctrl Pts',(-0.193849566274215,0.0049080439579958,
-0.00990973779496289));
#41637=CARTESIAN_POINT('Ctrl Pts',(-0.193852785118349,0.00493605141346052,
-0.00980856626502038));
#41638=CARTESIAN_POINT('Ctrl Pts',(-0.19416412360165,0.00699334436810937,
-0.0101391368498539));
#41639=CARTESIAN_POINT('Ctrl Pts',(-0.194061460165267,0.00700338018321717,
-0.0101395152380399));
#41640=CARTESIAN_POINT('Ctrl Pts',(-0.194064801952071,0.00700887609067415,
-0.0100358889677675));
#41641=CARTESIAN_POINT('Ctrl Pts',(-0.194246312133847,0.00802513287488578,
-0.0100830358876897));
#41642=CARTESIAN_POINT('Ctrl Pts',(-0.19414342831192,0.00803342503477834,
-0.0100824839740061));
#41643=CARTESIAN_POINT('Ctrl Pts',(-0.194146745965864,0.00802757386687429,
-0.00997950098896328));
#41644=CARTESIAN_POINT('Ctrl Pts',(-0.194290187104405,0.00259891113253263,
-0.00873470281275794));
#41645=CARTESIAN_POINT('Ctrl Pts',(-0.194289196087415,0.00259966116357646,
-0.00873513572158582));
#41646=CARTESIAN_POINT('Ctrl Pts',(-0.194286416940508,0.00260172379996549,
-0.008736291057404));
#41647=CARTESIAN_POINT('Ctrl Pts',(-0.194283643828663,0.00260385112950153,
-0.00873736128103573));
#41648=CARTESIAN_POINT('Ctrl Pts',(-0.194274462771107,0.00261119741567337,
-0.00874097761404353));
#41649=CARTESIAN_POINT('Ctrl Pts',(-0.194261757867021,0.00262161302243235,
-0.00874518598693824));
#41650=CARTESIAN_POINT('Ctrl Pts',(-0.19423621646237,0.00264584978012857,
-0.00874846049076316));
#41651=CARTESIAN_POINT('Ctrl Pts',(-0.194225125971027,0.0026573860669246,
-0.00874823380164047));
#41652=CARTESIAN_POINT('Ctrl Pts',(-0.194204592913332,0.00268156106677389,
-0.00874321412099836));
#41653=CARTESIAN_POINT('Ctrl Pts',(-0.194195984267789,0.00269338088257152,
-0.00873835693792421));
#41654=CARTESIAN_POINT('Ctrl Pts',(-0.194185890787921,0.00271055428582041,
-0.00872725214657669));
#41655=CARTESIAN_POINT('Ctrl Pts',(-0.194182801590003,0.00271688086249955,
-0.00872210658747948));
#41656=CARTESIAN_POINT('Ctrl Pts',(-0.194179113423095,0.00272757690945129,
-0.00871084654768075));
#41657=CARTESIAN_POINT('Ctrl Pts',(-0.194178237417962,0.00273197723860756,
-0.00870514428252823));
#41658=CARTESIAN_POINT('Ctrl Pts',(-0.194178261015029,0.00273576742350967,
-0.00869894006840107));
#41659=CARTESIAN_POINT('Ctrl Pts',(-0.193150275258269,0.0128441169814804,
-0.00842880923135799));
#41660=CARTESIAN_POINT('Ctrl Pts',(-0.193256325284946,0.0128379311470973,
-0.00844320696924679));
#41661=CARTESIAN_POINT('Ctrl Pts',(-0.193257206366102,0.0127778410782848,
-0.00835443734984138));
#41662=CARTESIAN_POINT('Ctrl Pts',(-0.193012927796993,0.0119927115204579,
-0.00900510709243607));
#41663=CARTESIAN_POINT('Ctrl Pts',(-0.193118624042428,0.0119821209508065,
-0.0090203118718904));
#41664=CARTESIAN_POINT('Ctrl Pts',(-0.193119759931369,0.0119315097041858,
-0.00892506728326148));
#41665=CARTESIAN_POINT('Ctrl Pts',(-0.192744917262978,0.0100930204918921,
-0.00988017938288733));
#41666=CARTESIAN_POINT('Ctrl Pts',(-0.192852605833001,0.010095868904492,
-0.00988588636415747));
#41667=CARTESIAN_POINT('Ctrl Pts',(-0.192854157456687,0.0100668059221215,
-0.00978080952480875));
#41668=CARTESIAN_POINT('Ctrl Pts',(-0.192955684307683,0.00800473900327279,
-0.0101117489985091));
#41669=CARTESIAN_POINT('Ctrl Pts',(-0.193061940873377,0.00801563509081901,
-0.0101204188260094));
#41670=CARTESIAN_POINT('Ctrl Pts',(-0.193063595677509,0.00800977514437518,
-0.0100127299449779));
#41671=CARTESIAN_POINT('Ctrl Pts',(-0.193039136173225,0.00697204692880732,
-0.0100554625058695));
#41672=CARTESIAN_POINT('Ctrl Pts',(-0.193145616630949,0.00698026662548628,
-0.0100650217034591));
#41673=CARTESIAN_POINT('Ctrl Pts',(-0.193147252943133,0.00698620175694981,
-0.00995799541934645));
#41674=CARTESIAN_POINT('Ctrl Pts',(-0.193103862234772,0.00750326159826634,
-0.00997223502421426));
#41675=CARTESIAN_POINT('Ctrl Pts',(-0.193103696428452,0.00750326382091886,
-0.00997867241877183));
#41676=CARTESIAN_POINT('Ctrl Pts',(-0.19310290699438,0.00750326582245723,
-0.00998507854929882));
#41677=CARTESIAN_POINT('Ctrl Pts',(-0.193099989901722,0.00750326946960355,
-0.00999815742026939));
#41678=CARTESIAN_POINT('Ctrl Pts',(-0.193097767534269,0.0075032710631149,
-0.0100047730394995));
#41679=CARTESIAN_POINT('Ctrl Pts',(-0.193089521905136,0.00750327467609872,
-0.0100228194487802));
#41680=CARTESIAN_POINT('Ctrl Pts',(-0.193081952036663,0.00750327586985883,
-0.0100333879480974));
#41681=CARTESIAN_POINT('Ctrl Pts',(-0.193063220755058,0.0075032758439836,
-0.0100510828272992));
#41682=CARTESIAN_POINT('Ctrl Pts',(-0.193052233129148,0.0075032746140179,
-0.0100580426754926));
#41683=CARTESIAN_POINT('Ctrl Pts',(-0.193020283179751,0.00750326846488784,
-0.0100705448117449));
#41684=CARTESIAN_POINT('Ctrl Pts',(-0.193003724950557,0.00750323391604461,
-0.0100696728225077));
#41685=CARTESIAN_POINT('Ctrl Pts',(-0.193001728824581,0.00750328363033614,
-0.010069640921573));
#41686=CARTESIAN_POINT('Ctrl Pts',(-0.193001286033377,0.00750326128071969,
-0.010069631677871));
#41687=CARTESIAN_POINT('Origin',(-0.193016821989473,0.00264931970905631,
-0.00862349334194056));
#41688=CARTESIAN_POINT('Ctrl Pts',(-0.193178913430778,0.00273545550310997,
-0.00867781944513263));
#41689=CARTESIAN_POINT('Ctrl Pts',(-0.193178786956274,0.00273148399745027,
-0.00868450526830737));
#41690=CARTESIAN_POINT('Ctrl Pts',(-0.193177865206733,0.00272678530631968,
-0.00869062192164722));
#41691=CARTESIAN_POINT('Ctrl Pts',(-0.193174378694683,0.00271560978211082,
-0.00870215245451658));
#41692=CARTESIAN_POINT('Ctrl Pts',(-0.193171686355034,0.00270913420128244,
-0.00870726645002183));
#41693=CARTESIAN_POINT('Ctrl Pts',(-0.193163020358285,0.00269149818684289,
-0.00871807095284634));
#41694=CARTESIAN_POINT('Ctrl Pts',(-0.193155886358353,0.00267948953902128,
-0.00872253867555305));
#41695=CARTESIAN_POINT('Ctrl Pts',(-0.193138925514157,0.00265465328672384,
-0.00872659620125043));
#41696=CARTESIAN_POINT('Ctrl Pts',(-0.193129671497449,0.002642574582794,
-0.00872620641933053));
#41697=CARTESIAN_POINT('Ctrl Pts',(-0.193106181219171,0.00261457933111291,
-0.00872055797890539));
#41698=CARTESIAN_POINT('Ctrl Pts',(-0.193094904929187,0.00260320861244047,
-0.00871383251213535));
#41699=CARTESIAN_POINT('Ctrl Pts',(-0.193091139850869,0.00259998782715419,
-0.00871194606472707));
#41700=CARTESIAN_POINT('Ctrl Pts',(-0.193090658832604,0.0025993312971884,
-0.00871155317921895));
#41701=CARTESIAN_POINT('Ctrl Pts',(-0.193090011126355,0.00259845151805998,
-0.00871102314495721));
#41702=CARTESIAN_POINT('Ctrl Pts',(-0.193089423336345,0.00259787423512406,
-0.00871066459632005));
#41703=CARTESIAN_POINT('Ctrl Pts',(-0.193258176380086,0.00222512554213558,
-0.008356333420045));
#41704=CARTESIAN_POINT('Ctrl Pts',(-0.193257406685722,0.00216515257785461,
-0.00844502540000934));
#41705=CARTESIAN_POINT('Ctrl Pts',(-0.193151455537886,0.00215890244938321,
-0.00843089879221508));
#41706=CARTESIAN_POINT('Ctrl Pts',(-0.193122002439102,0.00307212219069519,
-0.00892699819824813));
#41707=CARTESIAN_POINT('Ctrl Pts',(-0.19312097776627,0.00302162873844681,
-0.00902215789008911));
#41708=CARTESIAN_POINT('Ctrl Pts',(-0.193015373477763,0.00301107658670332,
-0.0090072570423295));
#41709=CARTESIAN_POINT('Ctrl Pts',(-0.192856798552873,0.004938435513375,
-0.00978238514439772));
#41710=CARTESIAN_POINT('Ctrl Pts',(-0.192855360966354,0.00490946584342564,
-0.00988735113571471));
#41711=CARTESIAN_POINT('Ctrl Pts',(-0.192747799146241,0.00491202380037548,
-0.00988180381919543));
#41712=CARTESIAN_POINT('Ctrl Pts',(-0.193063736243557,0.00699648123524497,
-0.0100130244108273));
#41713=CARTESIAN_POINT('Ctrl Pts',(-0.193062194778461,0.00699068968148678,
-0.0101205874911818));
#41714=CARTESIAN_POINT('Ctrl Pts',(-0.192956038359925,0.00700150933952738,
-0.0101121699854943));
#41715=CARTESIAN_POINT('Ctrl Pts',(-0.193146983756164,0.00802059256633889,
-0.00995750851088701));
#41716=CARTESIAN_POINT('Ctrl Pts',(-0.193145461334373,0.0080265884898962,
-0.0100644020028561));
#41717=CARTESIAN_POINT('Ctrl Pts',(-0.19303908563067,0.0080347289111402,
-0.0100550909375128));
#41718=CARTESIAN_POINT('Ctrl Pts',(-0.214216589193599,0.0124501517797991,
-0.00897739024746242));
#41719=CARTESIAN_POINT('Ctrl Pts',(-0.214214906549421,0.0125049445268657,
-0.00906167044569434));
#41720=CARTESIAN_POINT('Ctrl Pts',(-0.214314571072553,0.012494503099187,
-0.00906980642227252));
#41721=CARTESIAN_POINT('Ctrl Pts',(-0.214098604421142,0.0117052239517064,
-0.00946081335779316));
#41722=CARTESIAN_POINT('Ctrl Pts',(-0.214096725093907,0.0117518018313808,
-0.00955043625299295));
#41723=CARTESIAN_POINT('Ctrl Pts',(-0.214196353866795,0.0117403989593848,
-0.00955782479538539));
#41724=CARTESIAN_POINT('Ctrl Pts',(-0.213868936752257,0.0100586906401089,
-0.0102133997812258));
#41725=CARTESIAN_POINT('Ctrl Pts',(-0.213866781074678,0.010086875729085,
-0.0103113719504311));
#41726=CARTESIAN_POINT('Ctrl Pts',(-0.213967915697219,0.0100855217422406,
-0.0103112152848752));
#41727=CARTESIAN_POINT('Ctrl Pts',(-0.214026024666252,0.00825308653731274,
-0.0104575334667986));
#41728=CARTESIAN_POINT('Ctrl Pts',(-0.214023739513263,0.00826164733836335,
-0.0105581758061061));
#41729=CARTESIAN_POINT('Ctrl Pts',(-0.214123819636435,0.00827119179233783,
-0.010559097489943));
#41730=CARTESIAN_POINT('Ctrl Pts',(-0.214108345900493,0.00736178832954375,
-0.0104455690809484));
#41731=CARTESIAN_POINT('Ctrl Pts',(-0.21410606524853,0.00736033884333731,
-0.0105460685302323));
#41732=CARTESIAN_POINT('Ctrl Pts',(-0.214206164582688,0.00736950848589431,
-0.0105479371910573));
#41733=CARTESIAN_POINT('Ctrl Pts',(-0.214095598208164,0.00750036280421892,
-0.0104463507918903));
#41734=CARTESIAN_POINT('Ctrl Pts',(-0.214095450286403,0.00750036319807516,
-0.0104528962354918));
#41735=CARTESIAN_POINT('Ctrl Pts',(-0.214095948235342,0.00750036349347478,
-0.0104594399498248));
#41736=CARTESIAN_POINT('Ctrl Pts',(-0.214098293054094,0.00750036390124496,
-0.0104727451491399));
#41737=CARTESIAN_POINT('Ctrl Pts',(-0.214100217021513,0.00750036399949698,
-0.0104794566463362));
#41738=CARTESIAN_POINT('Ctrl Pts',(-0.214107648000867,0.00750036397740217,
-0.010497860091735));
#41739=CARTESIAN_POINT('Ctrl Pts',(-0.214114739600234,0.0075003635906343,
-0.0105087590474747));
#41740=CARTESIAN_POINT('Ctrl Pts',(-0.2141326670907,0.00750036233657987,
-0.0105272801749843));
#41741=CARTESIAN_POINT('Ctrl Pts',(-0.214143337315054,0.00750036136102943,
-0.0105347275236168));
#41742=CARTESIAN_POINT('Ctrl Pts',(-0.21416526406917,0.00750036056502232,
-0.0105444618788871));
#41743=CARTESIAN_POINT('Ctrl Pts',(-0.214176061651198,0.00750034115386931,
-0.0105472471779442));
#41744=CARTESIAN_POINT('Ctrl Pts',(-0.214189257514336,0.00750038006836895,
-0.0105484223801725));
#41745=CARTESIAN_POINT('Ctrl Pts',(-0.214191531845057,0.0075003523748629,
-0.0105485491122668));
#41746=CARTESIAN_POINT('Ctrl Pts',(-0.214193730602855,0.00750035199462301,
-0.0105485988658817));
#41747=CARTESIAN_POINT('Ctrl Pts',(-0.21418476171475,0.0122470248836337,
-0.00910661242247999));
#41748=CARTESIAN_POINT('Ctrl Pts',(-0.214184729492537,0.0122509958337976,
-0.0091128508218304));
#41749=CARTESIAN_POINT('Ctrl Pts',(-0.21418563061837,0.0122555871063697,
-0.00911855690753845));
#41750=CARTESIAN_POINT('Ctrl Pts',(-0.214189427897225,0.0122666878416324,
-0.00912974237444637));
#41751=CARTESIAN_POINT('Ctrl Pts',(-0.214192602948848,0.0122732155482737,
-0.00913480006953024));
#41752=CARTESIAN_POINT('Ctrl Pts',(-0.214202913814278,0.012290788265655,
-0.00914555709199986));
#41753=CARTESIAN_POINT('Ctrl Pts',(-0.214211662701835,0.0123027879767839,
-0.00915013351377761));
#41754=CARTESIAN_POINT('Ctrl Pts',(-0.214232489475916,0.0123272045160123,
-0.0091545341786767));
#41755=CARTESIAN_POINT('Ctrl Pts',(-0.214243724668783,0.012338802234618,
-0.00915444487536124));
#41756=CARTESIAN_POINT('Ctrl Pts',(-0.214271070311354,0.012364454941799,
-0.00915023794967844));
#41757=CARTESIAN_POINT('Ctrl Pts',(-0.214284343428429,0.0123749399149735,
-0.00914509100745944));
#41758=CARTESIAN_POINT('Ctrl Pts',(-0.214290958431559,0.0123799442675073,
-0.00914245939257118));
#41759=CARTESIAN_POINT('Ctrl Pts',(-0.214293751115597,0.0123821573006203,
-0.00914127256522943));
#41760=CARTESIAN_POINT('Ctrl Pts',(-0.214296544881388,0.0123843107719361,
-0.00913998276525925));
#41761=CARTESIAN_POINT('Ctrl Pts',(-0.214296932467762,0.0123846001898489,
-0.00913980814574909));
#41762=CARTESIAN_POINT('Origin',(-0.214347684294818,0.012331269897534,-0.00905622192851621));
#41763=CARTESIAN_POINT('Ctrl Pts',(-0.213184281197705,0.0122471129150008,
-0.00908524735490702));
#41764=CARTESIAN_POINT('Ctrl Pts',(-0.213184156012283,0.0122511428892307,
-0.0090917377174671));
#41765=CARTESIAN_POINT('Ctrl Pts',(-0.213183265788318,0.012255865025333,
-0.00909766666595631));
#41766=CARTESIAN_POINT('Ctrl Pts',(-0.213179903446603,0.0122670179573602,
-0.00910881858185788));
#41767=CARTESIAN_POINT('Ctrl Pts',(-0.21317731012386,0.0122734428477997,
-0.00911375708486854));
#41768=CARTESIAN_POINT('Ctrl Pts',(-0.213168885194293,0.0122910309742747,
-0.00912426161680266));
#41769=CARTESIAN_POINT('Ctrl Pts',(-0.213161889771395,0.012303025812301,
-0.00912858308631421));
#41770=CARTESIAN_POINT('Ctrl Pts',(-0.213145583015019,0.0123272295859375,
-0.00913230120812302));
#41771=CARTESIAN_POINT('Ctrl Pts',(-0.213136915228883,0.0123387079053039,
-0.00913193227948719));
#41772=CARTESIAN_POINT('Ctrl Pts',(-0.213117167511167,0.0123626169193058,
-0.0091273020756134));
#41773=CARTESIAN_POINT('Ctrl Pts',(-0.213107506698602,0.0123728239002587,
-0.0091226165296789));
#41774=CARTESIAN_POINT('Ctrl Pts',(-0.213100053077068,0.0123804799160748,
-0.00911833344043855));
#41775=CARTESIAN_POINT('Ctrl Pts',(-0.213097967534007,0.0123825341941126,
-0.00911715192851019));
#41776=CARTESIAN_POINT('Ctrl Pts',(-0.213095874558879,0.0123845334039177,
-0.00911589143619706));
#41777=CARTESIAN_POINT('Ctrl Pts',(-0.213095043824064,0.01238534178372,
-0.00911536679023199));
#41778=CARTESIAN_POINT('Ctrl Pts',(-0.214099251930435,0.00754007420866826,
-0.0104463437857496));
#41779=CARTESIAN_POINT('Ctrl Pts',(-0.214096973354194,0.00754042143926795,
-0.010546746497242));
#41780=CARTESIAN_POINT('Ctrl Pts',(-0.214196961785067,0.00753121108484114,
-0.0105486173304038));
#41781=CARTESIAN_POINT('Ctrl Pts',(-0.214020081132227,0.00668104711880522,
-0.01044839731125));
#41782=CARTESIAN_POINT('Ctrl Pts',(-0.214017802600064,0.00667177376162901,
-0.0105488323717457));
#41783=CARTESIAN_POINT('Ctrl Pts',(-0.214117810400573,0.00666260452057459,
-0.0105498212479641));
#41784=CARTESIAN_POINT('Ctrl Pts',(-0.21387699556738,0.00494790676441162,
-0.0102055683200936));
#41785=CARTESIAN_POINT('Ctrl Pts',(-0.213874843443667,0.00491981746697117,
-0.010303350730012));
#41786=CARTESIAN_POINT('Ctrl Pts',(-0.213975820466248,0.00492132683014941,
-0.010303508794821));
#41787=CARTESIAN_POINT('Ctrl Pts',(-0.214092364657753,0.00335460445828704,
-0.00948776443558196));
#41788=CARTESIAN_POINT('Ctrl Pts',(-0.214090476556027,0.00330875018108462,
-0.00957759356201309));
#41789=CARTESIAN_POINT('Ctrl Pts',(-0.214190056939973,0.00331969202055049,
-0.00958478139798083));
#41790=CARTESIAN_POINT('Ctrl Pts',(-0.214205206332109,0.00263311474131057,
-0.00903080833434456));
#41791=CARTESIAN_POINT('Ctrl Pts',(-0.21420350377054,0.0025792983289028,
-0.00911558882921577));
#41792=CARTESIAN_POINT('Ctrl Pts',(-0.214303063785917,0.00258973324630672,
-0.00912369765822408));
#41793=CARTESIAN_POINT('Ctrl Pts',(-0.214298632002388,0.00261569392237272,
-0.00914002695164348));
#41794=CARTESIAN_POINT('Ctrl Pts',(-0.214297526642216,0.00261652006806272,
-0.00914052536543213));
#41795=CARTESIAN_POINT('Ctrl Pts',(-0.214294851212556,0.00261849454413502,
-0.00914167725032275));
#41796=CARTESIAN_POINT('Ctrl Pts',(-0.214292183618819,0.00262052438289603,
-0.00914275417453498));
#41797=CARTESIAN_POINT('Ctrl Pts',(-0.214281346220273,0.00262906971274197,
-0.00914716403535739));
#41798=CARTESIAN_POINT('Ctrl Pts',(-0.214269186343652,0.00263913734339031,
-0.00915106719571335));
#41799=CARTESIAN_POINT('Ctrl Pts',(-0.214244917624073,0.00266202950687075,
-0.00915467550143725));
#41800=CARTESIAN_POINT('Ctrl Pts',(-0.214233875587385,0.00267347135966337,
-0.00915471589753221));
#41801=CARTESIAN_POINT('Ctrl Pts',(-0.214213246240943,0.00269770925175791,
-0.00915031153285751));
#41802=CARTESIAN_POINT('Ctrl Pts',(-0.214204528192406,0.00270969263822594,
-0.00914572400356269));
#41803=CARTESIAN_POINT('Ctrl Pts',(-0.21419426732704,0.00272722439751406,
-0.00913496538472965));
#41804=CARTESIAN_POINT('Ctrl Pts',(-0.214191112262838,0.00273372826159939,
-0.0091299171157316));
#41805=CARTESIAN_POINT('Ctrl Pts',(-0.214187339842144,0.00274478676577278,
-0.00911876281117197));
#41806=CARTESIAN_POINT('Ctrl Pts',(-0.214186444624373,0.00274936038677583,
-0.00911307602768412));
#41807=CARTESIAN_POINT('Ctrl Pts',(-0.214186475873142,0.00275331763246593,
-0.00910686068665908));
#41808=CARTESIAN_POINT('Ctrl Pts',(-0.213142440708018,0.00699294600996641,
-0.0104100731831301));
#41809=CARTESIAN_POINT('Ctrl Pts',(-0.213140554707719,0.00698694437899309,
-0.0105151055519326));
#41810=CARTESIAN_POINT('Ctrl Pts',(-0.213035974700116,0.00697822305542204,
-0.0105073143890869));
#41811=CARTESIAN_POINT('Ctrl Pts',(-0.213049377162493,0.00801213213024399,
-0.0104654545470825));
#41812=CARTESIAN_POINT('Ctrl Pts',(-0.213047475720085,0.00801810774455873,
-0.0105711737868596));
#41813=CARTESIAN_POINT('Ctrl Pts',(-0.212943124439694,0.00800638504375276,
-0.0105645204728977));
#41814=CARTESIAN_POINT('Ctrl Pts',(-0.212842352364478,0.0100623279960898,
-0.0102271605175154));
#41815=CARTESIAN_POINT('Ctrl Pts',(-0.212840544211089,0.01009180188059,
-0.0103301659891579));
#41816=CARTESIAN_POINT('Ctrl Pts',(-0.212734689214167,0.0100914727163342,
-0.0103258499497599));
#41817=CARTESIAN_POINT('Ctrl Pts',(-0.213129014550153,0.0119189081838315,
-0.00934123713579647));
#41818=CARTESIAN_POINT('Ctrl Pts',(-0.213127609118038,0.0119703221605139,
-0.00943382526992674));
#41819=CARTESIAN_POINT('Ctrl Pts',(-0.21302377890995,0.0119811156556074,
-0.00942016863823821));
#41820=CARTESIAN_POINT('Ctrl Pts',(-0.213264216023343,0.0127491362730295,
-0.00875480218796601));
#41821=CARTESIAN_POINT('Ctrl Pts',(-0.213263048470919,0.0128099587344319,
-0.00884064287774012));
#41822=CARTESIAN_POINT('Ctrl Pts',(-0.21315886773292,0.0128169295168079,
-0.00882760092589079));
#41823=CARTESIAN_POINT('Ctrl Pts',(-0.213095880539431,0.00750017780359572,
-0.0104239547305089));
#41824=CARTESIAN_POINT('Ctrl Pts',(-0.213095721214129,0.00750017803487418,
-0.0104304339542255));
#41825=CARTESIAN_POINT('Ctrl Pts',(-0.213094929764227,0.00750017836281809,
-0.0104368819660783));
#41826=CARTESIAN_POINT('Ctrl Pts',(-0.213092000414212,0.00750017925173218,
-0.0104500039596521));
#41827=CARTESIAN_POINT('Ctrl Pts',(-0.213089775050135,0.00750017982542014,
-0.0104566220242013));
#41828=CARTESIAN_POINT('Ctrl Pts',(-0.213081520029726,0.00750018179525219,
-0.0104746710065114));
#41829=CARTESIAN_POINT('Ctrl Pts',(-0.213073943407876,0.00750018343903434,
-0.0104852382500818));
#41830=CARTESIAN_POINT('Ctrl Pts',(-0.213055197914078,0.00750018768424061,
-0.0105029300505066));
#41831=CARTESIAN_POINT('Ctrl Pts',(-0.213044202463265,0.00750019002608837,
-0.0105098875003991));
#41832=CARTESIAN_POINT('Ctrl Pts',(-0.213021135749935,0.00750019768070943,
-0.010518903481104));
#41833=CARTESIAN_POINT('Ctrl Pts',(-0.213010247097905,0.00750017028527798,
-0.0105209450620031));
#41834=CARTESIAN_POINT('Ctrl Pts',(-0.212998853847316,0.00750023690197873,
-0.0105214428636747));
#41835=CARTESIAN_POINT('Ctrl Pts',(-0.212996578829288,0.00750021828623935,
-0.0105215072484914));
#41836=CARTESIAN_POINT('Ctrl Pts',(-0.212994302943105,0.00750019360234278,
-0.0105214911293679));
#41837=CARTESIAN_POINT('Ctrl Pts',(-0.212993240724087,0.00750019377101382,
-0.0105214671686418));
#41838=CARTESIAN_POINT('Origin',(-0.21302517694848,0.00266870828159353,
-0.00902982701552313));
#41839=CARTESIAN_POINT('Ctrl Pts',(-0.213185740409429,0.00275371303653609,
-0.00908578925174014));
#41840=CARTESIAN_POINT('Ctrl Pts',(-0.213185612971838,0.00274961466105284,
-0.00909239231469953));
#41841=CARTESIAN_POINT('Ctrl Pts',(-0.213184693731077,0.0027448011638584,
-0.00909841346185472));
#41842=CARTESIAN_POINT('Ctrl Pts',(-0.213181219083324,0.00273341254387324,
-0.00910971911879428));
#41843=CARTESIAN_POINT('Ctrl Pts',(-0.213178536862202,0.00272684414477028,
-0.00911470522324819));
#41844=CARTESIAN_POINT('Ctrl Pts',(-0.21316990049648,0.00270900982133904,
-0.00912516750127999));
#41845=CARTESIAN_POINT('Ctrl Pts',(-0.213162790186793,0.00269692100329651,
-0.00912940390992292));
#41846=CARTESIAN_POINT('Ctrl Pts',(-0.213146385039236,0.00267275589607126,
-0.0091328790996544));
#41847=CARTESIAN_POINT('Ctrl Pts',(-0.213137764208855,0.00266140345502128,
-0.00913242932358691));
#41848=CARTESIAN_POINT('Ctrl Pts',(-0.213117330046154,0.00263679519310755,
-0.00912750922551879));
#41849=CARTESIAN_POINT('Ctrl Pts',(-0.213107598825345,0.0026266537998736,
-0.00912243605506991));
#41850=CARTESIAN_POINT('Ctrl Pts',(-0.213101358052139,0.00262048871637618,
-0.00911897368291268));
#41851=CARTESIAN_POINT('Ctrl Pts',(-0.213099233398477,0.00261829223696965,
-0.00911770722992886));
#41852=CARTESIAN_POINT('Ctrl Pts',(-0.213097116059384,0.00261614680505331,
-0.0091163440307668));
#41853=CARTESIAN_POINT('Ctrl Pts',(-0.213096483107173,0.0026155313966941,
-0.00911594470885592));
#41854=CARTESIAN_POINT('Ctrl Pts',(-0.213265658282291,0.00225057084676559,
-0.00875447521358358));
#41855=CARTESIAN_POINT('Ctrl Pts',(-0.213264744741185,0.00218980535958929,
-0.008840281993757));
#41856=CARTESIAN_POINT('Ctrl Pts',(-0.213160606268671,0.00218265689036741,
-0.00882751612497404));
#41857=CARTESIAN_POINT('Ctrl Pts',(-0.213130481910092,0.00308438824308471,
-0.00934279710406928));
#41858=CARTESIAN_POINT('Ctrl Pts',(-0.213129329004748,0.00303307556144612,
-0.00943536985701307));
#41859=CARTESIAN_POINT('Ctrl Pts',(-0.213025538625966,0.00302219748557216,
-0.00942202949690465));
#41860=CARTESIAN_POINT('Ctrl Pts',(-0.212843199480043,0.00493694441905841,
-0.0102268568625341));
#41861=CARTESIAN_POINT('Ctrl Pts',(-0.212841649873723,0.00490748256281687,
-0.0103297954986793));
#41862=CARTESIAN_POINT('Ctrl Pts',(-0.212735839420919,0.00490746467376019,
-0.0103257302283149));
#41863=CARTESIAN_POINT('Ctrl Pts',(-0.213049443549872,0.00699508177473748,
-0.0104661729567559));
#41864=CARTESIAN_POINT('Ctrl Pts',(-0.213047796796832,0.00698916624074795,
-0.0105718413687105));
#41865=CARTESIAN_POINT('Ctrl Pts',(-0.212943495631933,0.00700098597986319,
-0.0105655225132302));
#41866=CARTESIAN_POINT('Ctrl Pts',(-0.213143561380097,0.00801624880458188,
-0.0104092466932483));
#41867=CARTESIAN_POINT('Ctrl Pts',(-0.213141931039774,0.00802233257455237,
-0.0105142129384645));
#41868=CARTESIAN_POINT('Ctrl Pts',(-0.213037395151643,0.00803106171242185,
-0.0105067282758358));
#41869=CARTESIAN_POINT('Ctrl Pts',(-0.224249358614769,0.00687656461498104,
-0.0107538129648876));
#41870=CARTESIAN_POINT('Ctrl Pts',(-0.224146963941182,0.00686817072021955,
-0.0107527866925382));
#41871=CARTESIAN_POINT('Ctrl Pts',(-0.22415008400599,0.00687543328094605,
-0.0106503629663698));
#41872=CARTESIAN_POINT('Ctrl Pts',(-0.224132405324884,0.00811458583753748,
-0.0108391610128464));
#41873=CARTESIAN_POINT('Ctrl Pts',(-0.224030296549097,0.00810362852284008,
-0.0108395232823109));
#41874=CARTESIAN_POINT('Ctrl Pts',(-0.224033448292523,0.00809656786194733,
-0.0107360879252381));
#41875=CARTESIAN_POINT('Ctrl Pts',(-0.223994326444125,0.009935896587635,
-0.0105862606529491));
#41876=CARTESIAN_POINT('Ctrl Pts',(-0.223890958264787,0.00993484545827698,
-0.0105884868534941));
#41877=CARTESIAN_POINT('Ctrl Pts',(-0.223894000185458,0.00990727874800546,
-0.0104878558471313));
#41878=CARTESIAN_POINT('Ctrl Pts',(-0.224201625418445,0.0122475977142339,
-0.00950202337095844));
#41879=CARTESIAN_POINT('Ctrl Pts',(-0.224100049629042,0.0122631652037639,
-0.00949385813830566));
#41880=CARTESIAN_POINT('Ctrl Pts',(-0.224102645082168,0.0122087968339061,
-0.00940581812444462));
#41881=CARTESIAN_POINT('Ctrl Pts',(-0.224501872325241,0.0132216434216143,
-0.00877052195614289));
#41882=CARTESIAN_POINT('Ctrl Pts',(-0.224401986451628,0.0132406747202252,
-0.00875564282850734));
#41883=CARTESIAN_POINT('Ctrl Pts',(-0.224404320778191,0.0131754555245871,
-0.00867586502401968));
#41884=CARTESIAN_POINT('Ctrl Pts',(-0.224648451537749,0.0137458892845509,
-0.00827431717742288));
#41885=CARTESIAN_POINT('Ctrl Pts',(-0.224547777311868,0.0137611889470385,
-0.00826038650712441));
#41886=CARTESIAN_POINT('Ctrl Pts',(-0.224549915217777,0.0136899440670359,
-0.00818634870946614));
#41887=CARTESIAN_POINT('Ctrl Pts',(-0.224092579354373,0.00750459639810974,
-0.0106722894261828));
#41888=CARTESIAN_POINT('Ctrl Pts',(-0.224092431483114,0.00750459981467394,
-0.0106788319827509));
#41889=CARTESIAN_POINT('Ctrl Pts',(-0.224092928593908,0.00750460341211288,
-0.0106853728753318));
#41890=CARTESIAN_POINT('Ctrl Pts',(-0.224095269901901,0.00750461110036911,
-0.0106986722511323));
#41891=CARTESIAN_POINT('Ctrl Pts',(-0.224097191048441,0.00750461518650435,
-0.0107053809658855));
#41892=CARTESIAN_POINT('Ctrl Pts',(-0.224104613212024,0.00750462699508637,
-0.0107237815254526));
#41893=CARTESIAN_POINT('Ctrl Pts',(-0.224111698620084,0.0075046347420132,
-0.0107346815510102));
#41894=CARTESIAN_POINT('Ctrl Pts',(-0.224129613368251,0.00750464951718822,
-0.0107532056091582));
#41895=CARTESIAN_POINT('Ctrl Pts',(-0.224140276779664,0.00750465641897557,
-0.010760655223077));
#41896=CARTESIAN_POINT('Ctrl Pts',(-0.224171583971623,0.00750467222431416,
-0.0107745674701099));
#41897=CARTESIAN_POINT('Ctrl Pts',(-0.224188125530322,0.00750471636626934,
-0.0107744642518765));
#41898=CARTESIAN_POINT('Ctrl Pts',(-0.224190207309728,0.00750464935161598,
-0.0107745253241387));
#41899=CARTESIAN_POINT('Ctrl Pts',(-0.224190650439283,0.00750467805224881,
-0.0107745361162036));
#41900=CARTESIAN_POINT('Ctrl Pts',(-0.224391683244397,0.0131382693052084,
-0.00867392737972874));
#41901=CARTESIAN_POINT('Ctrl Pts',(-0.224391710406589,0.0131432890534471,
-0.00867985880287643));
#41902=CARTESIAN_POINT('Ctrl Pts',(-0.22439285769896,0.013148886230224,
-0.00868509490634172));
#41903=CARTESIAN_POINT('Ctrl Pts',(-0.224397561810848,0.0131621998767523,
-0.0086951017775786));
#41904=CARTESIAN_POINT('Ctrl Pts',(-0.224401502093308,0.0131698613595927,
-0.00869933153551708));
#41905=CARTESIAN_POINT('Ctrl Pts',(-0.224413834049809,0.0131895382466903,
-0.00870743881998195));
#41906=CARTESIAN_POINT('Ctrl Pts',(-0.224424065927074,0.0132024287798354,
-0.00871006714770027));
#41907=CARTESIAN_POINT('Ctrl Pts',(-0.224447199176386,0.0132267953095936,
-0.00871030365850119));
#41908=CARTESIAN_POINT('Ctrl Pts',(-0.22445892069036,0.0132375333381397,
-0.00870850297455638));
#41909=CARTESIAN_POINT('Ctrl Pts',(-0.224487116206175,0.013260687524926,
-0.00870100701881826));
#41910=CARTESIAN_POINT('Ctrl Pts',(-0.224500648747928,0.0132697575697264,
-0.00869494905955054));
#41911=CARTESIAN_POINT('Ctrl Pts',(-0.224507713074331,0.0132742734863773,
-0.0086917394312852));
#41912=CARTESIAN_POINT('Ctrl Pts',(-0.224510690885442,0.0132762579354369,
-0.00869030259956035));
#41913=CARTESIAN_POINT('Ctrl Pts',(-0.224513666456228,0.013278172374563,
-0.0086887770895996));
#41914=CARTESIAN_POINT('Ctrl Pts',(-0.224514153384766,0.0132784758635244,
-0.00868853329176699));
#41915=CARTESIAN_POINT('Origin',(-0.224556048942401,0.0132144252691754,
-0.00861251969173161));
#41916=CARTESIAN_POINT('Ctrl Pts',(-0.223392308902647,0.0131383570271638,
-0.00865324427230983));
#41917=CARTESIAN_POINT('Ctrl Pts',(-0.223391478223472,0.0131771638355724,
-0.00870046215078917));
#41918=CARTESIAN_POINT('Ctrl Pts',(-0.223356797911615,0.0132504141439465,
-0.00869020496179645));
#41919=CARTESIAN_POINT('Ctrl Pts',(-0.223310623167959,0.0132796128233705,
-0.00866507631825959));
#41920=CARTESIAN_POINT('Ctrl Pts',(-0.224149821174384,0.00813275279168254,
-0.0106496691093151));
#41921=CARTESIAN_POINT('Ctrl Pts',(-0.224146591069773,0.00814013853683756,
-0.0107523669791903));
#41922=CARTESIAN_POINT('Ctrl Pts',(-0.224249274707641,0.0081317668384709,
-0.0107532183244048));
#41923=CARTESIAN_POINT('Ctrl Pts',(-0.224033317948185,0.00691366701361902,
-0.0107364086467913));
#41924=CARTESIAN_POINT('Ctrl Pts',(-0.224030056465752,0.00690672028603269,
-0.010840132722179));
#41925=CARTESIAN_POINT('Ctrl Pts',(-0.224132456425511,0.00689578562122801,
-0.0108395948104462));
#41926=CARTESIAN_POINT('Ctrl Pts',(-0.223897696321285,0.00510558493206286,
-0.0104908606147091));
#41927=CARTESIAN_POINT('Ctrl Pts',(-0.223894541433537,0.00507809492696955,
-0.0105918081483895));
#41928=CARTESIAN_POINT('Ctrl Pts',(-0.223998190955561,0.00507719189418989,
-0.0105894436356338));
#41929=CARTESIAN_POINT('Ctrl Pts',(-0.224105481204255,0.00280599846767248,
-0.00941458749263377));
#41930=CARTESIAN_POINT('Ctrl Pts',(-0.224102774907629,0.00275163113994665,
-0.00950296080652445));
#41931=CARTESIAN_POINT('Ctrl Pts',(-0.224204631329649,0.00276739369441223,
-0.0095109790856126));
#41932=CARTESIAN_POINT('Ctrl Pts',(-0.224411021980394,0.00183980157657985,
-0.00868815989720544));
#41933=CARTESIAN_POINT('Ctrl Pts',(-0.22440857672183,0.00177455565998491,
-0.00876828274438042));
#41934=CARTESIAN_POINT('Ctrl Pts',(-0.224508648171141,0.00179410941020286,
-0.0087832681782903));
#41935=CARTESIAN_POINT('Ctrl Pts',(-0.224558348333655,0.00132533951310742,
-0.00820104779287608));
#41936=CARTESIAN_POINT('Ctrl Pts',(-0.224556097212922,0.00125406268266188,
-0.00827544837477253));
#41937=CARTESIAN_POINT('Ctrl Pts',(-0.224657001291443,0.00126972303775823,
-0.00828942184362023));
#41938=CARTESIAN_POINT('Ctrl Pts',(-0.224519311691316,0.00173702433405029,
-0.00870149897983172));
#41939=CARTESIAN_POINT('Ctrl Pts',(-0.224519220600312,0.0017372814291356,
-0.00870171019746259));
#41940=CARTESIAN_POINT('Ctrl Pts',(-0.224519216540979,0.00173728966756444,
-0.00870171692049371));
#41941=CARTESIAN_POINT('Ctrl Pts',(-0.224519209013103,0.00173730456980275,
-0.00870172907411826));
#41942=CARTESIAN_POINT('Ctrl Pts',(-0.224519205575119,0.00173731124135664,
-0.00870173451241677));
#41943=CARTESIAN_POINT('Ctrl Pts',(-0.224519199433424,0.00173732293319819,
-0.00870174403826655));
#41944=CARTESIAN_POINT('Ctrl Pts',(-0.224519196754513,0.0017373279604,-0.00870174813260198));
#41945=CARTESIAN_POINT('Ctrl Pts',(-0.224519192095841,0.00173733658188121,
-0.00870175515163127));
#41946=CARTESIAN_POINT('Ctrl Pts',(-0.22451919013177,0.0017373401807803,
-0.00870175808082501));
#41947=CARTESIAN_POINT('Ctrl Pts',(-0.224519186779857,0.00173734626334747,
-0.00870176303019058));
#41948=CARTESIAN_POINT('Ctrl Pts',(-0.224519185400549,0.00173734874963384,
-0.00870176505289937));
#41949=CARTESIAN_POINT('Ctrl Pts',(-0.224519130731885,0.00173744664577636,
-0.00870184468127068));
#41950=CARTESIAN_POINT('Ctrl Pts',(-0.224519065751737,0.00173753884306144,
-0.0087019191232117));
#41951=CARTESIAN_POINT('Ctrl Pts',(-0.2245187439025,0.00173793770533865,
-0.00870223931247735));
#41952=CARTESIAN_POINT('Ctrl Pts',(-0.224518333336278,0.00173830175620587,
-0.00870252700870189));
#41953=CARTESIAN_POINT('Ctrl Pts',(-0.22451681766982,0.00173944371920888,
-0.00870340430495714));
#41954=CARTESIAN_POINT('Ctrl Pts',(-0.224515596397644,0.00174026901686821,
-0.00870401706726192));
#41955=CARTESIAN_POINT('Ctrl Pts',(-0.22451098119199,0.00174338793721464,
-0.00870627295981185));
#41956=CARTESIAN_POINT('Ctrl Pts',(-0.224503345553201,0.00174841869489124,
-0.0087097604492813));
#41957=CARTESIAN_POINT('Ctrl Pts',(-0.224475284124318,0.00176923113819895,
-0.00871980525483996));
#41958=CARTESIAN_POINT('Ctrl Pts',(-0.224458117016968,0.00178426683852684,
-0.00872315665637135));
#41959=CARTESIAN_POINT('Ctrl Pts',(-0.224430992756243,0.00181262222784833,
-0.00872295357100595));
#41960=CARTESIAN_POINT('Ctrl Pts',(-0.224420636237042,0.00182556167036,
-0.00872033878758797));
#41961=CARTESIAN_POINT('Ctrl Pts',(-0.224408119848623,0.001845342440675,
-0.00871221470017523));
#41962=CARTESIAN_POINT('Ctrl Pts',(-0.224404106074721,0.00185306562980442,
-0.00870795611609521));
#41963=CARTESIAN_POINT('Ctrl Pts',(-0.224399315895479,0.00186647544165982,
-0.00869786436819254));
#41964=CARTESIAN_POINT('Ctrl Pts',(-0.224398146464074,0.00187210650834024,
-0.00869258439038758));
#41965=CARTESIAN_POINT('Ctrl Pts',(-0.22439811687663,0.00187715215324153,
-0.0086865994148203));
#41966=CARTESIAN_POINT('Ctrl Pts',(-0.223149962924227,0.00688159725283423,
-0.0106277838502364));
#41967=CARTESIAN_POINT('Ctrl Pts',(-0.223149018566613,0.00687388623400185,
-0.0107379305151485));
#41968=CARTESIAN_POINT('Ctrl Pts',(-0.223039601465183,0.00686565537877052,
-0.0107253915764655));
#41969=CARTESIAN_POINT('Ctrl Pts',(-0.223032133013148,0.00810963982917846,
-0.010712135585432));
#41970=CARTESIAN_POINT('Ctrl Pts',(-0.223031162244556,0.00811737830930937,
-0.0108233620581352));
#41971=CARTESIAN_POINT('Ctrl Pts',(-0.222922021349851,0.00810490151169142,
-0.0108122114891207));
#41972=CARTESIAN_POINT('Ctrl Pts',(-0.222896079921506,0.00990391154468539,
-0.0104620565626817));
#41973=CARTESIAN_POINT('Ctrl Pts',(-0.222895202078949,0.00993344674867837,
-0.0105702383938425));
#41974=CARTESIAN_POINT('Ctrl Pts',(-0.222784776813472,0.00992939962176445,
-0.010561275979829));
#41975=CARTESIAN_POINT('Ctrl Pts',(-0.223098701300928,0.0121793888445334,
-0.00940057916956953));
#41976=CARTESIAN_POINT('Ctrl Pts',(-0.22309832541927,0.0122373659809578,
-0.00949551234578024));
#41977=CARTESIAN_POINT('Ctrl Pts',(-0.222989588048026,0.0122472772909027,
-0.00947737528566851));
#41978=CARTESIAN_POINT('Ctrl Pts',(-0.223394133274712,0.0131415067565888,
-0.00868370116431274));
#41979=CARTESIAN_POINT('Ctrl Pts',(-0.223394073245122,0.0132110639533715,
-0.00876992906736614));
#41980=CARTESIAN_POINT('Ctrl Pts',(-0.223287262630516,0.013224394796061,
-0.00874500740247201));
#41981=CARTESIAN_POINT('Ctrl Pts',(-0.223543103505894,0.0136646114584795,
-0.00819237472604023));
#41982=CARTESIAN_POINT('Ctrl Pts',(-0.223543240367587,0.0137407637285344,
-0.00827241646594224));
#41983=CARTESIAN_POINT('Ctrl Pts',(-0.22343553583012,0.0137491865171251,
-0.00824924824531338));
#41984=CARTESIAN_POINT('Ctrl Pts',(-0.223092860967492,0.00750411360131228,
-0.0106501154996819));
#41985=CARTESIAN_POINT('Ctrl Pts',(-0.223092689252814,0.00750411655891282,
-0.0106565195151663));
#41986=CARTESIAN_POINT('Ctrl Pts',(-0.223091900256382,0.007504119330255,
-0.0106628920790118));
#41987=CARTESIAN_POINT('Ctrl Pts',(-0.223088988672676,0.00750412464538914,
-0.0106759407068649));
#41988=CARTESIAN_POINT('Ctrl Pts',(-0.223086764633423,0.00750412713355253,
-0.0106825582346915));
#41989=CARTESIAN_POINT('Ctrl Pts',(-0.223078514335347,0.00750413331383906,
-0.0107006061115379));
#41990=CARTESIAN_POINT('Ctrl Pts',(-0.22307094167459,0.00750413617150116,
-0.0107111737687284));
#41991=CARTESIAN_POINT('Ctrl Pts',(-0.22305220504925,0.00750413928636017,
-0.0107288662343668));
#41992=CARTESIAN_POINT('Ctrl Pts',(-0.22304121484608,0.00750413950075735,
-0.0107358244608144));
#41993=CARTESIAN_POINT('Ctrl Pts',(-0.223016540981556,0.00750413733438505,
-0.01074547417355));
#41994=CARTESIAN_POINT('Ctrl Pts',(-0.223004164996846,0.00750411469378559,
-0.0107474049779053));
#41995=CARTESIAN_POINT('Ctrl Pts',(-0.222992339708995,0.00750413754074494,
-0.0107474330725274));
#41996=CARTESIAN_POINT('Ctrl Pts',(-0.222991913153699,0.00750413853913309,
-0.0107474311162282));
#41997=CARTESIAN_POINT('Ctrl Pts',(-0.222991332215326,0.00750414349283911,
-0.0107474252051021));
#41998=CARTESIAN_POINT('Ctrl Pts',(-0.222991075316954,0.00750414620344912,
-0.0107474218012963));
#41999=CARTESIAN_POINT('Ctrl Pts',(-0.222990721887929,0.0075041585497481,
-0.0107474159745127));
#42000=CARTESIAN_POINT('Ctrl Pts',(-0.222990363822996,0.00750425357435802,
-0.0107474086907247));
#42001=CARTESIAN_POINT('Origin',(-0.223237220057076,0.00179857992405682,
-0.00859864314724398));
#42002=CARTESIAN_POINT('Ctrl Pts',(-0.223398256964007,0.00187628033601208,
-0.00866522709035868));
#42003=CARTESIAN_POINT('Ctrl Pts',(-0.223398154124069,0.00187143799250317,
-0.00867114607163627));
#42004=CARTESIAN_POINT('Ctrl Pts',(-0.223397350846328,0.00186597106090046,
-0.00867642715907607));
#42005=CARTESIAN_POINT('Ctrl Pts',(-0.223394293473877,0.00185343700847406,
-0.00868604789434846));
#42006=CARTESIAN_POINT('Ctrl Pts',(-0.223391931127745,0.0018464009619336,
-0.00869012656777989));
#42007=CARTESIAN_POINT('Ctrl Pts',(-0.223383990852377,0.0018269365722086,
-0.00869852527535584));
#42008=CARTESIAN_POINT('Ctrl Pts',(-0.223377431966919,0.00181434780212607,
-0.00870103413584041));
#42009=CARTESIAN_POINT('Ctrl Pts',(-0.223362558207148,0.00178986818748107,
-0.00870155486970696));
#42010=CARTESIAN_POINT('Ctrl Pts',(-0.223354229968575,0.00177799425123853,
-0.00869951688709378));
#42011=CARTESIAN_POINT('Ctrl Pts',(-0.22333313535445,0.00175125673571012,
-0.00869015734281729));
#42012=CARTESIAN_POINT('Ctrl Pts',(-0.22332294719884,0.00174102013770642,
-0.00868214080278602));
#42013=CARTESIAN_POINT('Ctrl Pts',(-0.223319160138154,0.00173753989374147,
-0.00867940971146196));
#42014=CARTESIAN_POINT('Ctrl Pts',(-0.223318489660597,0.00173675249287678,
-0.00867877460776524));
#42015=CARTESIAN_POINT('Ctrl Pts',(-0.223317594518492,0.00173570789287372,
-0.0086779195615712));
#42016=CARTESIAN_POINT('Ctrl Pts',(-0.223316845454304,0.00173498134307272,
-0.00867730420572105));
#42017=CARTESIAN_POINT('Ctrl Pts',(-0.22303890850229,0.00814164430623871,
-0.0107248133017441));
#42018=CARTESIAN_POINT('Ctrl Pts',(-0.223148789072647,0.00813348754910934,
-0.0107379204692242));
#42019=CARTESIAN_POINT('Ctrl Pts',(-0.223149727731801,0.00812565130849946,
-0.0106272611136563));
#42020=CARTESIAN_POINT('Ctrl Pts',(-0.22292134689892,0.00690441691685615,
-0.010812507614285));
#42021=CARTESIAN_POINT('Ctrl Pts',(-0.223030955661194,0.00689190154903563,
-0.0108242264473683));
#42022=CARTESIAN_POINT('Ctrl Pts',(-0.223031920968427,0.00689956170670937,
-0.010712472343137));
#42023=CARTESIAN_POINT('Ctrl Pts',(-0.222788348228539,0.00508263051192417,
-0.0105641367381816));
#42024=CARTESIAN_POINT('Ctrl Pts',(-0.222899223939067,0.00507857159790477,
-0.0105737078620945));
#42025=CARTESIAN_POINT('Ctrl Pts',(-0.222900097730721,0.00510809073197549,
-0.0104649776228588));
#42026=CARTESIAN_POINT('Ctrl Pts',(-0.222991460019885,0.00276656231961293,
-0.0094855610854456));
#42027=CARTESIAN_POINT('Ctrl Pts',(-0.223100667398899,0.00277626708247984,
-0.0095041815587128));
#42028=CARTESIAN_POINT('Ctrl Pts',(-0.22310103778877,0.00283435031683848,
-0.00940870301260069));
#42029=CARTESIAN_POINT('Ctrl Pts',(-0.223292840953927,0.00179022353787926,
-0.00875673827642576));
#42030=CARTESIAN_POINT('Ctrl Pts',(-0.223400003218155,0.00180370409004607,
-0.00878241709270048));
#42031=CARTESIAN_POINT('Ctrl Pts',(-0.223400057319882,0.00187340518877495,
-0.00869563469557495));
#42032=CARTESIAN_POINT('Ctrl Pts',(-0.223442953334174,0.00126547903518434,
-0.00826334125889978));
#42033=CARTESIAN_POINT('Ctrl Pts',(-0.22355106295208,0.00127380217909774,
-0.00828714426754558));
#42034=CARTESIAN_POINT('Ctrl Pts',(-0.223550922316616,0.00135012429573583,
-0.00820654454718633));
#42035=CARTESIAN_POINT('Ctrl Pts',(-0.212223744032557,0.0125025714233182,
-0.00890371716457249));
#42036=CARTESIAN_POINT('Ctrl Pts',(-0.212222075153114,0.0125578143517975,
-0.00898781500481288));
#42037=CARTESIAN_POINT('Ctrl Pts',(-0.212321835550297,0.0125473597144221,
-0.00899591238820372));
#42038=CARTESIAN_POINT('Ctrl Pts',(-0.212102724242109,0.0117434852742709,
-0.00940161356959696));
#42039=CARTESIAN_POINT('Ctrl Pts',(-0.2121008512821,0.011790384772016,-0.00949119962975025));
#42040=CARTESIAN_POINT('Ctrl Pts',(-0.212200537118151,0.0117786534455685,
-0.00949867729488359));
#42041=CARTESIAN_POINT('Ctrl Pts',(-0.21186514967656,0.0100599062468189,
-0.0101749354638583));
#42042=CARTESIAN_POINT('Ctrl Pts',(-0.211862990722436,0.0100880414368075,
-0.010273079418359));
#42043=CARTESIAN_POINT('Ctrl Pts',(-0.211964249557042,0.0100869126121601,
-0.0102726729652089));
#42044=CARTESIAN_POINT('Ctrl Pts',(-0.212031119293791,0.00821222072325896,
-0.010417780967713));
#42045=CARTESIAN_POINT('Ctrl Pts',(-0.212028829701335,0.00822031116530004,
-0.0105185764981024));
#42046=CARTESIAN_POINT('Ctrl Pts',(-0.212128989819408,0.00822998234265434,
-0.010519447140182));
#42047=CARTESIAN_POINT('Ctrl Pts',(-0.212114323073989,0.00730098728432662,
-0.0103993599395582));
#42048=CARTESIAN_POINT('Ctrl Pts',(-0.212112040942403,0.00729885878555155,
-0.0104999410658259));
#42049=CARTESIAN_POINT('Ctrl Pts',(-0.212212246789137,0.00730790211731437,
-0.0105017797457116));
#42050=CARTESIAN_POINT('Ctrl Pts',(-0.212096204769044,0.0075000580009567,
-0.0104011630123803));
#42051=CARTESIAN_POINT('Ctrl Pts',(-0.212096056852805,0.00750005816148503,
-0.01040770818223));
#42052=CARTESIAN_POINT('Ctrl Pts',(-0.212096554695983,0.00750005821014383,
-0.0104142516334717));
#42053=CARTESIAN_POINT('Ctrl Pts',(-0.212098899076221,0.0075000580878504,
-0.0104275562750958));
#42054=CARTESIAN_POINT('Ctrl Pts',(-0.21210082269123,0.00750005790295219,
-0.0104342675106612));
#42055=CARTESIAN_POINT('Ctrl Pts',(-0.212108252487303,0.0075000570574498,
-0.0104526705817974));
#42056=CARTESIAN_POINT('Ctrl Pts',(-0.212115343160954,0.00750005612495993,
-0.0104635696258613));
#42057=CARTESIAN_POINT('Ctrl Pts',(-0.212133268656717,0.00750005380450097,
-0.0104820909648401));
#42058=CARTESIAN_POINT('Ctrl Pts',(-0.212143937749959,0.00750005232560142,
-0.010489538526628));
#42059=CARTESIAN_POINT('Ctrl Pts',(-0.212165860746876,0.00750005060557715,
-0.0104992724855804));
#42060=CARTESIAN_POINT('Ctrl Pts',(-0.212176657990042,0.00750003194978452,
-0.0105020589538083));
#42061=CARTESIAN_POINT('Ctrl Pts',(-0.212189859904008,0.00750006809023092,
-0.0105032346276707));
#42062=CARTESIAN_POINT('Ctrl Pts',(-0.212192126960573,0.00750004200194685,
-0.0105033609494816));
#42063=CARTESIAN_POINT('Ctrl Pts',(-0.212194328823658,0.00750004157488686,
-0.0105034107592895));
#42064=CARTESIAN_POINT('Ctrl Pts',(-0.21218385926235,0.0122487198827948,
-0.00906545454917522));
#42065=CARTESIAN_POINT('Ctrl Pts',(-0.212183827797059,0.0122526842341265,
-0.00907170643872819));
#42066=CARTESIAN_POINT('Ctrl Pts',(-0.212184731565329,0.0122572705102556,
-0.00907742635298329));
#42067=CARTESIAN_POINT('Ctrl Pts',(-0.212188538992215,0.0122683657498729,
-0.00908864426940098));
#42068=CARTESIAN_POINT('Ctrl Pts',(-0.212191722914003,0.0122748939085551,
-0.00909371908495357));
#42069=CARTESIAN_POINT('Ctrl Pts',(-0.212202056114265,0.0122924621358694,
-0.00910451018441334));
#42070=CARTESIAN_POINT('Ctrl Pts',(-0.212210818437941,0.0123044575381293,
-0.00910910546837787));
#42071=CARTESIAN_POINT('Ctrl Pts',(-0.212231927329752,0.0123291664640641,
-0.00911359453592));
#42072=CARTESIAN_POINT('Ctrl Pts',(-0.212243486433075,0.0123410475842637,
-0.00911346132650099));
#42073=CARTESIAN_POINT('Ctrl Pts',(-0.212272773255435,0.0123683538825616,
-0.00910877928464044));
#42074=CARTESIAN_POINT('Ctrl Pts',(-0.212287224212214,0.0123794352589682,
-0.00910270522660073));
#42075=CARTESIAN_POINT('Ctrl Pts',(-0.212292284315582,0.0123831279553651,
-0.00910069980871974));
#42076=CARTESIAN_POINT('Ctrl Pts',(-0.212293389463492,0.012384053549551,
-0.00910017313244616));
#42077=CARTESIAN_POINT('Ctrl Pts',(-0.212294871275834,0.0123852874724164,
-0.00909945683622047));
#42078=CARTESIAN_POINT('Ctrl Pts',(-0.212296027595393,0.0123861510372385,
-0.009098937945711));
#42079=CARTESIAN_POINT('Origin',(-0.21234693243841,0.0123329390950867,-0.00901527903468506));
#42080=CARTESIAN_POINT('Ctrl Pts',(-0.211183468881297,0.0122495385747751,
-0.00904367844858987));
#42081=CARTESIAN_POINT('Ctrl Pts',(-0.211183343796021,0.0122535585151899,
-0.00905017738989069));
#42082=CARTESIAN_POINT('Ctrl Pts',(-0.211182453405063,0.0122582724090962,
-0.0090561153782017));
#42083=CARTESIAN_POINT('Ctrl Pts',(-0.211179090245664,0.0122694120307349,
-0.00906728735112201));
#42084=CARTESIAN_POINT('Ctrl Pts',(-0.211176496173649,0.0122758323451357,
-0.00907223640641804));
#42085=CARTESIAN_POINT('Ctrl Pts',(-0.211168070280735,0.0122934113463099,
-0.00908276662220862));
#42086=CARTESIAN_POINT('Ctrl Pts',(-0.211161074881815,0.0123054047079806,
-0.00908710442762168));
#42087=CARTESIAN_POINT('Ctrl Pts',(-0.211144770725815,0.0123296125141419,
-0.00909085366891658));
#42088=CARTESIAN_POINT('Ctrl Pts',(-0.211136106097826,0.0123410951196305,
-0.00909049964893237));
#42089=CARTESIAN_POINT('Ctrl Pts',(-0.211116251718935,0.0123651604647786,
-0.00908587455126835));
#42090=CARTESIAN_POINT('Ctrl Pts',(-0.211106531274097,0.0123754212444389,
-0.00908112970234405));
#42091=CARTESIAN_POINT('Ctrl Pts',(-0.211099292974643,0.0123828819846203,
-0.00907697188113588));
#42092=CARTESIAN_POINT('Ctrl Pts',(-0.211097175768363,0.0123849684867918,
-0.00907577873419521));
#42093=CARTESIAN_POINT('Ctrl Pts',(-0.211095050524522,0.0123869971186745,
-0.00907450260566078));
#42094=CARTESIAN_POINT('Ctrl Pts',(-0.211094251609883,0.0123877761518248,
-0.00907399894463725));
#42095=CARTESIAN_POINT('Ctrl Pts',(-0.212122639608489,0.00778880978652429,
-0.0103971099742313));
#42096=CARTESIAN_POINT('Ctrl Pts',(-0.212120360088168,0.00779194299561869,
-0.0104975869020762));
#42097=CARTESIAN_POINT('Ctrl Pts',(-0.212220489784696,0.00778295730589407,
-0.0104996007168518));
#42098=CARTESIAN_POINT('Ctrl Pts',(-0.212036322893619,0.00684878518939332,
-0.0104254825969592));
#42099=CARTESIAN_POINT('Ctrl Pts',(-0.212034031410779,0.00684136848125649,
-0.0105262845556704));
#42100=CARTESIAN_POINT('Ctrl Pts',(-0.212134071486609,0.00683127857741346,
-0.0105272683569319));
#42101=CARTESIAN_POINT('Ctrl Pts',(-0.211859116564673,0.00494160052946475,
-0.0101852940024049));
#42102=CARTESIAN_POINT('Ctrl Pts',(-0.211856956852588,0.00491351503003851,
-0.0102834759349862));
#42103=CARTESIAN_POINT('Ctrl Pts',(-0.211958176675694,0.00491482182811779,
-0.0102830491123946));
#42104=CARTESIAN_POINT('Ctrl Pts',(-0.212112373295386,0.0032005167473659,
-0.00937556293289828));
#42105=CARTESIAN_POINT('Ctrl Pts',(-0.212110512545602,0.00315302214095645,
-0.00946478708467834));
#42106=CARTESIAN_POINT('Ctrl Pts',(-0.212210070325435,0.00316501813895363,
-0.00947257547566129));
#42107=CARTESIAN_POINT('Ctrl Pts',(-0.212236649846315,0.00242474532205975,
-0.00885552488235436));
#42108=CARTESIAN_POINT('Ctrl Pts',(-0.212235002070394,0.00236874779667176,
-0.00893902616285966));
#42109=CARTESIAN_POINT('Ctrl Pts',(-0.212334697644786,0.00237898510803345,
-0.00894721593752821));
#42110=CARTESIAN_POINT('Ctrl Pts',(-0.212297192971603,0.00261509486573022,
-0.0090997425089851));
#42111=CARTESIAN_POINT('Ctrl Pts',(-0.212296110945992,0.00261590407640106,
-0.00910022856999239));
#42112=CARTESIAN_POINT('Ctrl Pts',(-0.212293412623576,0.00261789339678241,
-0.0091013849447997));
#42113=CARTESIAN_POINT('Ctrl Pts',(-0.21229072211904,0.00261994008618735,
-0.00910246433139768));
#42114=CARTESIAN_POINT('Ctrl Pts',(-0.212279944466258,0.00262844975228672,
-0.00910683558573018));
#42115=CARTESIAN_POINT('Ctrl Pts',(-0.212267736210671,0.00263855465871684,
-0.00911073569201036));
#42116=CARTESIAN_POINT('Ctrl Pts',(-0.212243429959653,0.00266148531971882,
-0.00911429271001131));
#42117=CARTESIAN_POINT('Ctrl Pts',(-0.212232378426442,0.00267293677256201,
-0.00911430297192282));
#42118=CARTESIAN_POINT('Ctrl Pts',(-0.212211756375655,0.00269716377811193,
-0.00910982811301855));
#42119=CARTESIAN_POINT('Ctrl Pts',(-0.21220305063021,0.00270912604835164,
-0.00910521030688519));
#42120=CARTESIAN_POINT('Ctrl Pts',(-0.212192809462358,0.00272661431929928,
-0.00909441411988624));
#42121=CARTESIAN_POINT('Ctrl Pts',(-0.212189662427839,0.00273309690234965,
-0.00908935613340753));
#42122=CARTESIAN_POINT('Ctrl Pts',(-0.212185900147284,0.00274411373944175,
-0.00907819293916975));
#42123=CARTESIAN_POINT('Ctrl Pts',(-0.21218500728268,0.00274866811026422,
-0.00907250584239902));
#42124=CARTESIAN_POINT('Ctrl Pts',(-0.212185037759281,0.00275260737022776,
-0.00906629345677396));
#42125=CARTESIAN_POINT('Ctrl Pts',(-0.211142485728535,0.00699254756608383,
-0.0103648734390101));
#42126=CARTESIAN_POINT('Ctrl Pts',(-0.211140615484092,0.00698654179680735,
-0.0104703120129651));
#42127=CARTESIAN_POINT('Ctrl Pts',(-0.211035650260988,0.00697789315409504,
-0.0104621222159787));
#42128=CARTESIAN_POINT('Ctrl Pts',(-0.21105098460499,0.00801203950050848,
-0.0104201724986889));
#42129=CARTESIAN_POINT('Ctrl Pts',(-0.211049098611664,0.0080180188886255,
-0.0105262966533945));
#42130=CARTESIAN_POINT('Ctrl Pts',(-0.210944361367469,0.00800640351237446,
-0.010519208094519));
#42131=CARTESIAN_POINT('Ctrl Pts',(-0.21084304256263,0.0100629658036953,
-0.0101824905154317));
#42132=CARTESIAN_POINT('Ctrl Pts',(-0.210841251020845,0.0100924675827056,
-0.0102859051076613));
#42133=CARTESIAN_POINT('Ctrl Pts',(-0.210735015997111,0.0100917271809107,
-0.0102812652497566));
#42134=CARTESIAN_POINT('Ctrl Pts',(-0.211127758772214,0.0119207402552615,
-0.00929899445208153));
#42135=CARTESIAN_POINT('Ctrl Pts',(-0.211126372276215,0.0119721993876384,
-0.0093920197491322));
#42136=CARTESIAN_POINT('Ctrl Pts',(-0.211022169348734,0.0119829372674086,
-0.00937797181211293));
#42137=CARTESIAN_POINT('Ctrl Pts',(-0.211263625788997,0.0127522795019374,
-0.00871403619118547));
#42138=CARTESIAN_POINT('Ctrl Pts',(-0.211262479217963,0.0128131718323431,
-0.00880032500501877));
#42139=CARTESIAN_POINT('Ctrl Pts',(-0.211157922926716,0.0128199712353316,
-0.00878693220959459));
#42140=CARTESIAN_POINT('Ctrl Pts',(-0.211096536156126,0.00750001934821516,
-0.0103787795142135));
#42141=CARTESIAN_POINT('Ctrl Pts',(-0.211096376187743,0.00750001946084664,
-0.0103852544749745));
#42142=CARTESIAN_POINT('Ctrl Pts',(-0.211095584978032,0.00750001968840412,
-0.0103916982231778));
#42143=CARTESIAN_POINT('Ctrl Pts',(-0.211092657009911,0.00750002040873107,
-0.0104048157068072));
#42144=CARTESIAN_POINT('Ctrl Pts',(-0.211090432074856,0.00750002091781133,
-0.0104114334162529));
#42145=CARTESIAN_POINT('Ctrl Pts',(-0.211082178394124,0.00750002276793853,
-0.010429482029809));
#42146=CARTESIAN_POINT('Ctrl Pts',(-0.211074602730834,0.00750002441393692,
-0.0104400494546364));
#42147=CARTESIAN_POINT('Ctrl Pts',(-0.211055859246741,0.00750002879137767,
-0.010457741705717));
#42148=CARTESIAN_POINT('Ctrl Pts',(-0.211044864897043,0.00750003127898264,
-0.0104646995036328));
#42149=CARTESIAN_POINT('Ctrl Pts',(-0.211020920185128,0.00750003942093849,
-0.0104740601580318));
#42150=CARTESIAN_POINT('Ctrl Pts',(-0.211009741601578,0.00750002059763051,
-0.0104758093131767));
#42151=CARTESIAN_POINT('Ctrl Pts',(-0.210998442893526,0.00750008203547272,
-0.0104763032297964));
#42152=CARTESIAN_POINT('Ctrl Pts',(-0.210996045383314,0.0075000361891443,
-0.0104763287856277));
#42153=CARTESIAN_POINT('Ctrl Pts',(-0.210993906189512,0.00750003658947422,
-0.0104762805591888));
#42154=CARTESIAN_POINT('Origin',(-0.211023786144693,0.00266742943825413,
-0.00898917183642173));
#42155=CARTESIAN_POINT('Ctrl Pts',(-0.211184235669001,0.00275259873665137,
-0.00904500540329008));
#42156=CARTESIAN_POINT('Ctrl Pts',(-0.211184108309872,0.00274851237207321,
-0.00905161691332531));
#42157=CARTESIAN_POINT('Ctrl Pts',(-0.211183188947385,0.00274370938574701,
-0.00905764748316005));
#42158=CARTESIAN_POINT('Ctrl Pts',(-0.211179713684398,0.00273233943804887,
-0.00906897486538284));
#42159=CARTESIAN_POINT('Ctrl Pts',(-0.211177030906755,0.00272577864903201,
-0.00907397300667125));
#42160=CARTESIAN_POINT('Ctrl Pts',(-0.211168393401542,0.00270795989164768,
-0.00908446663829167));
#42161=CARTESIAN_POINT('Ctrl Pts',(-0.211161282430324,0.00269587613625519,
-0.00908872380984227));
#42162=CARTESIAN_POINT('Ctrl Pts',(-0.211144763685762,0.00267154571914486,
-0.00909226395652573));
#42163=CARTESIAN_POINT('Ctrl Pts',(-0.211136007252681,0.00266002880499524,
-0.00909179650619916));
#42164=CARTESIAN_POINT('Ctrl Pts',(-0.211114293659952,0.00263393192613597,
-0.00908649757919211));
#42165=CARTESIAN_POINT('Ctrl Pts',(-0.21110391131705,0.00262337571113696,
-0.00908068371600419));
#42166=CARTESIAN_POINT('Ctrl Pts',(-0.211098093898507,0.00261770147937051,
-0.00907744793165228));
#42167=CARTESIAN_POINT('Ctrl Pts',(-0.211096595484061,0.00261601608586272,
-0.00907641942581189));
#42168=CARTESIAN_POINT('Ctrl Pts',(-0.211094980169537,0.0026144429765102,
-0.00907540295747494));
#42169=CARTESIAN_POINT('Ctrl Pts',(-0.211264251736995,0.00224882937558932,
-0.00871473025010786));
#42170=CARTESIAN_POINT('Ctrl Pts',(-0.211263315213782,0.00218803254801025,
-0.00880095577930301));
#42171=CARTESIAN_POINT('Ctrl Pts',(-0.211158843112418,0.00218106932820431,
-0.00878785654339923));
#42172=CARTESIAN_POINT('Ctrl Pts',(-0.211128629078001,0.00308374196045554,
-0.00930120455681559));
#42173=CARTESIAN_POINT('Ctrl Pts',(-0.211127451514235,0.0030324147703501,
-0.00939417776413184));
#42174=CARTESIAN_POINT('Ctrl Pts',(-0.211023329710713,0.0030216079367658,
-0.00938046250689989));
#42175=CARTESIAN_POINT('Ctrl Pts',(-0.210843656731025,0.00493713697694662,
-0.0101823031690562));
#42176=CARTESIAN_POINT('Ctrl Pts',(-0.210842079736846,0.00490766886678799,
-0.0102856076466288));
#42177=CARTESIAN_POINT('Ctrl Pts',(-0.210735934247016,0.00490808327359709,
-0.0102812256263012));
#42178=CARTESIAN_POINT('Ctrl Pts',(-0.211051060565633,0.00699481541135514,
-0.0104208672824074));
#42179=CARTESIAN_POINT('Ctrl Pts',(-0.211049386046545,0.00698889960147933,
-0.0105268935653299));
#42180=CARTESIAN_POINT('Ctrl Pts',(-0.210944743332313,0.00700060848094322,
-0.0105201436677757));
#42181=CARTESIAN_POINT('Ctrl Pts',(-0.211143590272674,0.00801614047287985,
-0.010364127037553));
#42182=CARTESIAN_POINT('Ctrl Pts',(-0.211141932328472,0.00802222390702669,
-0.0104694534195357));
#42183=CARTESIAN_POINT('Ctrl Pts',(-0.211037055788434,0.00803088427681597,
-0.0104615756474694));
#42184=CARTESIAN_POINT('Ctrl Pts',(-0.202265290724368,0.0127832636642769,
-0.00852006183626685));
#42185=CARTESIAN_POINT('Ctrl Pts',(-0.202262909678109,0.012841850283284,
-0.00860438640498691));
#42186=CARTESIAN_POINT('Ctrl Pts',(-0.202364791393614,0.0128310798128724,
-0.0086115609851021));
#42187=CARTESIAN_POINT('Ctrl Pts',(-0.202126399278693,0.0119512167802099,
-0.00909768849379822));
#42188=CARTESIAN_POINT('Ctrl Pts',(-0.202123771768196,0.012000709183594,
-0.00918838710668978));
#42189=CARTESIAN_POINT('Ctrl Pts',(-0.202225304576364,0.0119862994107232,
-0.00919586084607411));
#42190=CARTESIAN_POINT('Ctrl Pts',(-0.201846781273398,0.0100683927693504,
-0.0099854198429024));
#42191=CARTESIAN_POINT('Ctrl Pts',(-0.201843792519172,0.0100967254867997,
-0.0100860378814493));
#42192=CARTESIAN_POINT('Ctrl Pts',(-0.201947320966196,0.0100968345400587,
-0.0100833761264778));
#42193=CARTESIAN_POINT('Ctrl Pts',(-0.202060563303902,0.00799480983044915,
-0.0102172781045443));
#42194=CARTESIAN_POINT('Ctrl Pts',(-0.202057447540456,0.00800043688524475,
-0.0103204296036954));
#42195=CARTESIAN_POINT('Ctrl Pts',(-0.202159609967776,0.00801057803168537,
-0.0103203078618906));
#42196=CARTESIAN_POINT('Ctrl Pts',(-0.202143369671317,0.00697652998217102,
-0.0101604268468326));
#42197=CARTESIAN_POINT('Ctrl Pts',(-0.202140278060583,0.00697067620638285,
-0.0102629252905548));
#42198=CARTESIAN_POINT('Ctrl Pts',(-0.20224266649913,0.00697898140682514,
-0.0102637635116727));
#42199=CARTESIAN_POINT('Ctrl Pts',(-0.202099470462991,0.00750048539628712,
-0.0101752292159335));
#42200=CARTESIAN_POINT('Ctrl Pts',(-0.202099322575853,0.00750048571666395,
-0.0101817727997466));
#42201=CARTESIAN_POINT('Ctrl Pts',(-0.20209981982129,0.0075004858146974,
-0.0101883147240483));
#42202=CARTESIAN_POINT('Ctrl Pts',(-0.20210216172605,0.00750048555557407,
-0.010201616141842));
#42203=CARTESIAN_POINT('Ctrl Pts',(-0.202104083353711,0.00750048516985556,
-0.0102083258634756));
#42204=CARTESIAN_POINT('Ctrl Pts',(-0.202111506517437,0.00750048337028386,
-0.0102267268383148));
#42205=CARTESIAN_POINT('Ctrl Pts',(-0.202118592045866,0.00750048137816934,
-0.0102376264068436));
#42206=CARTESIAN_POINT('Ctrl Pts',(-0.202136506508522,0.00750047596863676,
-0.0102561490420348));
#42207=CARTESIAN_POINT('Ctrl Pts',(-0.202147169384737,0.00750047260069426,
-0.0102635978567623));
#42208=CARTESIAN_POINT('Ctrl Pts',(-0.202174878281523,0.00750046356239206,
-0.010275909799322));
#42209=CARTESIAN_POINT('Ctrl Pts',(-0.202188847780365,0.00750044923868025,
-0.0102772242529343));
#42210=CARTESIAN_POINT('Ctrl Pts',(-0.202197059864926,0.00750045701803727,
-0.0102774632695266));
#42211=CARTESIAN_POINT('Ctrl Pts',(-0.202197548253278,0.00750045578297359,
-0.0102774753489076));
#42212=CARTESIAN_POINT('Ctrl Pts',(-0.202180802979017,0.0122592813346522,
-0.00885976042488077));
#42213=CARTESIAN_POINT('Ctrl Pts',(-0.202180775847905,0.0122631848049861,
-0.00886603768293643));
#42214=CARTESIAN_POINT('Ctrl Pts',(-0.202181681606649,0.0122677133629349,
-0.00887178950452203));
#42215=CARTESIAN_POINT('Ctrl Pts',(-0.202185493168263,0.0122787039443237,
-0.00888310262482018));
#42216=CARTESIAN_POINT('Ctrl Pts',(-0.202188683106617,0.0122851909308943,
-0.00888823749218621));
#42217=CARTESIAN_POINT('Ctrl Pts',(-0.202199031228896,0.012302669305196,
-0.00889918392779031));
#42218=CARTESIAN_POINT('Ctrl Pts',(-0.202207803768514,0.0123146277241332,
-0.00890388368097754));
#42219=CARTESIAN_POINT('Ctrl Pts',(-0.202229052741313,0.0123394414366878,
-0.00890861211537678));
#42220=CARTESIAN_POINT('Ctrl Pts',(-0.202240765246994,0.0123514568709592,
-0.00890855459003177));
#42221=CARTESIAN_POINT('Ctrl Pts',(-0.202270373507782,0.0123790254521622,
-0.00890396725067058));
#42222=CARTESIAN_POINT('Ctrl Pts',(-0.202284941527497,0.0123902440180487,
-0.00889785858207483));
#42223=CARTESIAN_POINT('Ctrl Pts',(-0.202290001326585,0.0123938505451035,
-0.00889591408271268));
#42224=CARTESIAN_POINT('Ctrl Pts',(-0.202290902964131,0.0123946426922635,
-0.00889546575730262));
#42225=CARTESIAN_POINT('Ctrl Pts',(-0.202292112602265,0.0123957005749798,
-0.00889485866884196));
#42226=CARTESIAN_POINT('Ctrl Pts',(-0.202293077439418,0.0123964246955439,
-0.00889443257618142));
#42227=CARTESIAN_POINT('Origin',(-0.202343912991874,0.0123440163406885,
-0.00881026170755109));
#42228=CARTESIAN_POINT('Ctrl Pts',(-0.201180514909525,0.0122597855112167,
-0.00883836470388977));
#42229=CARTESIAN_POINT('Ctrl Pts',(-0.201180390511959,0.0122637441796246,
-0.00884489930376825));
#42230=CARTESIAN_POINT('Ctrl Pts',(-0.201179501260221,0.0122684013630966,
-0.00885088006671312));
#42231=CARTESIAN_POINT('Ctrl Pts',(-0.201176141270069,0.0122794323622778,
-0.00886215414657635));
#42232=CARTESIAN_POINT('Ctrl Pts',(-0.201173549386715,0.0122858033738214,
-0.00886716297674856));
#42233=CARTESIAN_POINT('Ctrl Pts',(-0.201165128329775,0.0123032779251533,
-0.00887786039664943));
#42234=CARTESIAN_POINT('Ctrl Pts',(-0.201158135612939,0.0123152267687501,
-0.00888231322892227));
#42235=CARTESIAN_POINT('Ctrl Pts',(-0.201141838373897,0.0123393891695866,
-0.00888629578960458));
#42236=CARTESIAN_POINT('Ctrl Pts',(-0.201133177159222,0.0123508700904303,
-0.00888605332684157));
#42237=CARTESIAN_POINT('Ctrl Pts',(-0.201113045567628,0.0123753147450016,
-0.00888159927525391));
#42238=CARTESIAN_POINT('Ctrl Pts',(-0.201103352145789,0.0123855377193998,
-0.00887687172049721));
#42239=CARTESIAN_POINT('Ctrl Pts',(-0.201096412597187,0.0123927376362332,
-0.00887294806780029));
#42240=CARTESIAN_POINT('Ctrl Pts',(-0.20109426545364,0.0123948624411427,
-0.00887176173410875));
#42241=CARTESIAN_POINT('Ctrl Pts',(-0.201092109876422,0.0123969273961565,
-0.0088704880551081));
#42242=CARTESIAN_POINT('Ctrl Pts',(-0.201091342169912,0.0123976805086701,
-0.00887001123180993));
#42243=CARTESIAN_POINT('Ctrl Pts',(-0.202361917638471,0.00217353042035395,
-0.00861470493313823));
#42244=CARTESIAN_POINT('Ctrl Pts',(-0.202259856285326,0.00216286571190057,
-0.00860743380920193));
#42245=CARTESIAN_POINT('Ctrl Pts',(-0.202262561385939,0.00222152827281342,
-0.0085229612533595));
#42246=CARTESIAN_POINT('Ctrl Pts',(-0.202223288299755,0.00301801026424016,
-0.00919806500274725));
#42247=CARTESIAN_POINT('Ctrl Pts',(-0.202121575048064,0.00300371014208909,
-0.0091904858511563));
#42248=CARTESIAN_POINT('Ctrl Pts',(-0.202124525544528,0.0030532785590825,
-0.0090996406391749));
#42249=CARTESIAN_POINT('Ctrl Pts',(-0.201945891174042,0.00490640788157693,
-0.010083958182011));
#42250=CARTESIAN_POINT('Ctrl Pts',(-0.201842188963288,0.00490652939523789,
-0.0100864703603933));
#42251=CARTESIAN_POINT('Ctrl Pts',(-0.201845506877496,0.00493487034859226,
-0.00998567581196493));
#42252=CARTESIAN_POINT('Ctrl Pts',(-0.202159089889202,0.00699079557499788,
-0.0103202697089951));
#42253=CARTESIAN_POINT('Ctrl Pts',(-0.202056762552271,0.00700105132225664,
-0.0103202502333414));
#42254=CARTESIAN_POINT('Ctrl Pts',(-0.20206020309972,0.00700663927775264,
-0.0102169335833552));
#42255=CARTESIAN_POINT('Ctrl Pts',(-0.20224286412263,0.00802148069263829,
-0.0102637453647374));
#42256=CARTESIAN_POINT('Ctrl Pts',(-0.202140309173562,0.0080298578112884,
-0.0102627524167362));
#42257=CARTESIAN_POINT('Ctrl Pts',(-0.202143726326102,0.00802396304981702,
-0.0101600928451061));
#42258=CARTESIAN_POINT('Ctrl Pts',(-0.20229073304026,0.00260802933164804,
-0.00889712262070968));
#42259=CARTESIAN_POINT('Ctrl Pts',(-0.202289712354061,0.00260879620236029,
-0.00889757326702722));
#42260=CARTESIAN_POINT('Ctrl Pts',(-0.202286953018036,0.00261083227107042,
-0.00889873350857407));
#42261=CARTESIAN_POINT('Ctrl Pts',(-0.202284199630092,0.00261293162289047,
-0.0088998116244581));
#42262=CARTESIAN_POINT('Ctrl Pts',(-0.202274881790007,0.0026203321779655,
-0.00890352576831182));
#42263=CARTESIAN_POINT('Ctrl Pts',(-0.202262295585051,0.00263060385711503,
-0.00890774115835158));
#42264=CARTESIAN_POINT('Ctrl Pts',(-0.202236950697834,0.0026545294227545,
-0.00891122052825115));
#42265=CARTESIAN_POINT('Ctrl Pts',(-0.202225895790699,0.00266597494293841,
-0.00891112273377692));
#42266=CARTESIAN_POINT('Ctrl Pts',(-0.202205263183689,0.00269015250105854,
-0.00890642122194838));
#42267=CARTESIAN_POINT('Ctrl Pts',(-0.2021965521082,0.00270206949852077,
-0.00890169128285083));
#42268=CARTESIAN_POINT('Ctrl Pts',(-0.202186302463196,0.00271945585024983,
-0.00889073024673815));
#42269=CARTESIAN_POINT('Ctrl Pts',(-0.20218315201515,0.0027258921553306,
-0.00888560973687531));
#42270=CARTESIAN_POINT('Ctrl Pts',(-0.202179387654478,0.0027367989427911,
-0.00887434605633525));
#42271=CARTESIAN_POINT('Ctrl Pts',(-0.202178493553465,0.00274129479059584,
-0.00886862285140853));
#42272=CARTESIAN_POINT('Ctrl Pts',(-0.202178520809953,0.00274517218894165,
-0.00886238122749359));
#42273=CARTESIAN_POINT('Ctrl Pts',(-0.201155090292175,0.0128339461321558,
-0.00858641773309735));
#42274=CARTESIAN_POINT('Ctrl Pts',(-0.201260979997059,0.0128276733596081,
-0.008601020897081));
#42275=CARTESIAN_POINT('Ctrl Pts',(-0.201261993178973,0.0127668493824425,
-0.00851290802901172));
#42276=CARTESIAN_POINT('Ctrl Pts',(-0.201015035208462,0.011987649430818,
-0.00917044849004206));
#42277=CARTESIAN_POINT('Ctrl Pts',(-0.201120561593533,0.0119769211070483,
-0.00918585984469463));
#42278=CARTESIAN_POINT('Ctrl Pts',(-0.201121824479614,0.0119256299247488,
-0.00909110167463794));
#42279=CARTESIAN_POINT('Ctrl Pts',(-0.200741069345388,0.0100927310436652,
-0.0100583529007995));
#42280=CARTESIAN_POINT('Ctrl Pts',(-0.200848651520605,0.0100954146705308,
-0.0100640154274109));
#42281=CARTESIAN_POINT('Ctrl Pts',(-0.20085032774782,0.0100659660403532,
-0.00995911849787239));
#42282=CARTESIAN_POINT('Ctrl Pts',(-0.200951730607667,0.0080022228618309,
-0.0102933609042937));
#42283=CARTESIAN_POINT('Ctrl Pts',(-0.201057860798874,0.00801312022949754,
-0.0103020134424343));
#42284=CARTESIAN_POINT('Ctrl Pts',(-0.201059637391599,0.00800721062667035,
-0.0101944359329035));
#42285=CARTESIAN_POINT('Ctrl Pts',(-0.201035042743625,0.00696923703703989,
-0.0102357723537515));
#42286=CARTESIAN_POINT('Ctrl Pts',(-0.201141399474779,0.00697741160227575,
-0.0102453287437788));
#42287=CARTESIAN_POINT('Ctrl Pts',(-0.201143158232884,0.00698347932538022,
-0.0101384386393281));
#42288=CARTESIAN_POINT('Ctrl Pts',(-0.201099840401704,0.00750066861474714,
-0.0101529052072166));
#42289=CARTESIAN_POINT('Ctrl Pts',(-0.201099677169239,0.00750066912054103,
-0.0101593582616468));
#42290=CARTESIAN_POINT('Ctrl Pts',(-0.201098887242449,0.00750066989291298,
-0.0101657801072424));
#42291=CARTESIAN_POINT('Ctrl Pts',(-0.201095966520023,0.00750067202929758,
-0.0101788743168739));
#42292=CARTESIAN_POINT('Ctrl Pts',(-0.20109374392092,0.0075006734288361,
-0.0101854901135771));
#42293=CARTESIAN_POINT('Ctrl Pts',(-0.201085497549442,0.0075006781819555,
-0.010203536733078));
#42294=CARTESIAN_POINT('Ctrl Pts',(-0.201077927130068,0.00750068213977413,
-0.0102141051489183));
#42295=CARTESIAN_POINT('Ctrl Pts',(-0.201059194678892,0.00750069135896144,
-0.0102317998180977));
#42296=CARTESIAN_POINT('Ctrl Pts',(-0.201048206402947,0.00750069653436368,
-0.010238759491104));
#42297=CARTESIAN_POINT('Ctrl Pts',(-0.201021557960836,0.00750070864767776,
-0.0102491862051309));
#42298=CARTESIAN_POINT('Ctrl Pts',(-0.201008029147252,0.00750070956203601,
-0.0102505221971764));
#42299=CARTESIAN_POINT('Ctrl Pts',(-0.20099770582662,0.00750071937682855,
-0.0102503571197901));
#42300=CARTESIAN_POINT('Ctrl Pts',(-0.200997257667548,0.00750071911133179,
-0.0102503477931785));
#42301=CARTESIAN_POINT('Origin',(-0.201017212115499,0.00265911537344352,
-0.00878606880213356));
#42302=CARTESIAN_POINT('Ctrl Pts',(-0.201177754620579,0.0027448415119716,
-0.00884107761226325));
#42303=CARTESIAN_POINT('Ctrl Pts',(-0.201177628042387,0.00274082641373192,
-0.00884771612051796));
#42304=CARTESIAN_POINT('Ctrl Pts',(-0.201176712286097,0.00273609158279732,
-0.008853782822355));
#42305=CARTESIAN_POINT('Ctrl Pts',(-0.201173250003288,0.00272485674829661,
-0.00886520275453687));
#42306=CARTESIAN_POINT('Ctrl Pts',(-0.201170577213625,0.00271835999346171,
-0.00887025880407389));
#42307=CARTESIAN_POINT('Ctrl Pts',(-0.201161962995019,0.00270066932355189,
-0.00888092912017631));
#42308=CARTESIAN_POINT('Ctrl Pts',(-0.201154864234623,0.00268863669597218,
-0.00888531233553696));
#42309=CARTESIAN_POINT('Ctrl Pts',(-0.20113811014608,0.00266397446442915,
-0.00888917124572946));
#42310=CARTESIAN_POINT('Ctrl Pts',(-0.201129051225016,0.00265208658043163,
-0.0088887448390463));
#42311=CARTESIAN_POINT('Ctrl Pts',(-0.201106193044083,0.00262469960299615,
-0.0088831853591339));
#42312=CARTESIAN_POINT('Ctrl Pts',(-0.201095158723894,0.00261358759693136,
-0.00887674001446222));
#42313=CARTESIAN_POINT('Ctrl Pts',(-0.20109109045133,0.00260980814508552,
-0.00887454309705644));
#42314=CARTESIAN_POINT('Ctrl Pts',(-0.201090343739424,0.00260894149648861,
-0.00887402415850547));
#42315=CARTESIAN_POINT('Ctrl Pts',(-0.20108934207694,0.00260778484674993,
-0.00887332012892615));
#42316=CARTESIAN_POINT('Ctrl Pts',(-0.201088523107266,0.00260698192588514,
-0.0088728124292417));
#42317=CARTESIAN_POINT('Ctrl Pts',(-0.201258741752539,0.00223790006051546,
-0.00851599811712773));
#42318=CARTESIAN_POINT('Ctrl Pts',(-0.201257833511546,0.00217713357105664,
-0.00860416818402206));
#42319=CARTESIAN_POINT('Ctrl Pts',(-0.201151914418942,0.00217085125914763,
-0.00858968164457007));
#42320=CARTESIAN_POINT('Ctrl Pts',(-0.201119551825336,0.0030788662053447,
-0.0090932840728631));
#42321=CARTESIAN_POINT('Ctrl Pts',(-0.201118393839695,0.00302763434948745,
-0.00918808984717891));
#42322=CARTESIAN_POINT('Ctrl Pts',(-0.201012835888744,0.00301693193686283,
-0.00917280217687647));
#42323=CARTESIAN_POINT('Ctrl Pts',(-0.200848681291751,0.00493768758826015,
-0.00995971868738787));
#42324=CARTESIAN_POINT('Ctrl Pts',(-0.200847112869582,0.00490827835577488,
-0.0100646364930119));
#42325=CARTESIAN_POINT('Ctrl Pts',(-0.200739509642514,0.00491089619573715,
-0.010059053811372));
#42326=CARTESIAN_POINT('Ctrl Pts',(-0.20105915724458,0.0069945413110089,
-0.0101943176570579));
#42327=CARTESIAN_POINT('Ctrl Pts',(-0.201057487566078,0.006988641463598,
-0.0103019102012954));
#42328=CARTESIAN_POINT('Ctrl Pts',(-0.200951344751406,0.00699964817927347,
-0.0102933594943047));
#42329=CARTESIAN_POINT('Ctrl Pts',(-0.201143595912237,0.00801742258598695,
-0.0101382994581758));
#42330=CARTESIAN_POINT('Ctrl Pts',(-0.201141944150171,0.00802349301337347,
-0.0102452048937045));
#42331=CARTESIAN_POINT('Ctrl Pts',(-0.20103557348225,0.00803175898212767,
-0.0102357331328223));
#42332=CARTESIAN_POINT('Ctrl Pts',(-0.200264188629852,0.0127861801628926,
-0.00848016633972643));
#42333=CARTESIAN_POINT('Ctrl Pts',(-0.200261797905388,0.0128446548055681,
-0.00856471227770291));
#42334=CARTESIAN_POINT('Ctrl Pts',(-0.200363805385546,0.0128338532231718,
-0.00857173926582449));
#42335=CARTESIAN_POINT('Ctrl Pts',(-0.200125964276301,0.0119528335885076,
-0.00905604844208056));
#42336=CARTESIAN_POINT('Ctrl Pts',(-0.200123325889639,0.0120022189944504,
-0.00914693499322317));
#42337=CARTESIAN_POINT('Ctrl Pts',(-0.200224987570178,0.0119877937173126,
-0.00915425753864673));
#42338=CARTESIAN_POINT('Ctrl Pts',(-0.19984820163058,0.0100686222287371,
-0.00994082914119559));
#42339=CARTESIAN_POINT('Ctrl Pts',(-0.199845199470471,0.0100968901927037,
-0.0100415764810079));
#42340=CARTESIAN_POINT('Ctrl Pts',(-0.199948841017887,0.0100970427571912,
-0.0100388081310723));
#42341=CARTESIAN_POINT('Ctrl Pts',(-0.200061564759937,0.00799550694355067,
-0.0101718836147545));
#42342=CARTESIAN_POINT('Ctrl Pts',(-0.200058435840963,0.00800112432784995,
-0.0102751496995788));
#42343=CARTESIAN_POINT('Ctrl Pts',(-0.200160719650638,0.00801122946222692,
-0.0102749241092734));
#42344=CARTESIAN_POINT('Ctrl Pts',(-0.200144097286729,0.00697707856075904,
-0.0101153254435978));
#42345=CARTESIAN_POINT('Ctrl Pts',(-0.200140992571978,0.00697124582500046,
-0.0102179431873745));
#42346=CARTESIAN_POINT('Ctrl Pts',(-0.200243500976602,0.00697954697503826,
-0.0102186691874395));
#42347=CARTESIAN_POINT('Ctrl Pts',(-0.200100331002871,0.00750107109769107,
-0.0101300470129157));
#42348=CARTESIAN_POINT('Ctrl Pts',(-0.200100183117646,0.00750107182035176,
-0.0101365905644933));
#42349=CARTESIAN_POINT('Ctrl Pts',(-0.200100680353927,0.00750107222471504,
-0.0101431324573533));
#42350=CARTESIAN_POINT('Ctrl Pts',(-0.200103022217917,0.00750107239064495,
-0.010156433809306));
#42351=CARTESIAN_POINT('Ctrl Pts',(-0.200104943812047,0.00750107210931998,
-0.0101631434994043));
#42352=CARTESIAN_POINT('Ctrl Pts',(-0.200112366866152,0.00750107027570379,
-0.0101815444323523));
#42353=CARTESIAN_POINT('Ctrl Pts',(-0.200119452311889,0.00750106786353869,
-0.0101924440069437));
#42354=CARTESIAN_POINT('Ctrl Pts',(-0.200137366599506,0.00750106086311714,
-0.0102109666628549));
#42355=CARTESIAN_POINT('Ctrl Pts',(-0.200148029378955,0.00750105633974303,
-0.0102184154983561));
#42356=CARTESIAN_POINT('Ctrl Pts',(-0.200175341152975,0.007501044049354,
-0.0102305511306864));
#42357=CARTESIAN_POINT('Ctrl Pts',(-0.200189126148084,0.00750104583392516,
-0.010232025111573));
#42358=CARTESIAN_POINT('Ctrl Pts',(-0.200197937876526,0.0075010321737249,
-0.0102322815350947));
#42359=CARTESIAN_POINT('Ctrl Pts',(-0.200198408070096,0.00750103283571237,
-0.0102322930866153));
#42360=CARTESIAN_POINT('Ctrl Pts',(-0.200180145804599,0.0122615403574039,
-0.00881880956225188));
#42361=CARTESIAN_POINT('Ctrl Pts',(-0.200180119422939,0.0122654310898583,
-0.00882509212040225));
#42362=CARTESIAN_POINT('Ctrl Pts',(-0.200181024695127,0.012269947624273,
-0.00883085076702477));
#42363=CARTESIAN_POINT('Ctrl Pts',(-0.200184833727551,0.012280916013167,
-0.00884218362675862));
#42364=CARTESIAN_POINT('Ctrl Pts',(-0.200188022040074,0.0122873940992912,
-0.00884733112275432));
#42365=CARTESIAN_POINT('Ctrl Pts',(-0.200198364920575,0.0123048538863272,
-0.00885831053742095));
#42366=CARTESIAN_POINT('Ctrl Pts',(-0.200207132450346,0.0123168044121634,
-0.00886303220381333));
#42367=CARTESIAN_POINT('Ctrl Pts',(-0.200228410920646,0.0123416602759976,
-0.00886781500745342));
#42368=CARTESIAN_POINT('Ctrl Pts',(-0.200240168145585,0.0123537241143239,
-0.00886776943648934));
#42369=CARTESIAN_POINT('Ctrl Pts',(-0.200269920520539,0.0123814322404116,
-0.00886317053365818));
#42370=CARTESIAN_POINT('Ctrl Pts',(-0.20028454807678,0.0123927103831329,
-0.00885700343686482));
#42371=CARTESIAN_POINT('Ctrl Pts',(-0.200289515178599,0.0123962065901031,
-0.00885511747434229));
#42372=CARTESIAN_POINT('Ctrl Pts',(-0.200290340245052,0.0123969503360318,
-0.00885469577831727));
#42373=CARTESIAN_POINT('Ctrl Pts',(-0.200291447572802,0.0123979443029324,
-0.00885412567643322));
#42374=CARTESIAN_POINT('Ctrl Pts',(-0.200292341609995,0.0123986165584613,
-0.00885373182846497));
#42375=CARTESIAN_POINT('Origin',(-0.200343175462262,0.0123463747446592,
-0.0087694564592868));
#42376=CARTESIAN_POINT('Ctrl Pts',(-0.199179785887974,0.0122620277131703,
-0.00879745964969994));
#42377=CARTESIAN_POINT('Ctrl Pts',(-0.199179661572149,0.0122659741273922,
-0.0088040027320839));
#42378=CARTESIAN_POINT('Ctrl Pts',(-0.199178771661386,0.0122706202061008,
-0.00880999314679547));
#42379=CARTESIAN_POINT('Ctrl Pts',(-0.199175408875086,0.0122816306366328,
-0.00882128986615296));
#42380=CARTESIAN_POINT('Ctrl Pts',(-0.199172814695162,0.0122879926693539,
-0.00882631142860891));
#42381=CARTESIAN_POINT('Ctrl Pts',(-0.199164386859704,0.0123054469889948,
-0.0088370426202018));
#42382=CARTESIAN_POINT('Ctrl Pts',(-0.199157388756533,0.012317387084561,
-0.00884151841784895));
#42383=CARTESIAN_POINT('Ctrl Pts',(-0.199141079666825,0.0123415402785929,
-0.00884554723861314));
#42384=CARTESIAN_POINT('Ctrl Pts',(-0.19913241292987,0.0123530199318005,
-0.00884532702339733));
#42385=CARTESIAN_POINT('Ctrl Pts',(-0.199112251006035,0.0123774910375646,
-0.00884091757244983));
#42386=CARTESIAN_POINT('Ctrl Pts',(-0.199102544559066,0.0123877253055016,
-0.00883620109091419));
#42387=CARTESIAN_POINT('Ctrl Pts',(-0.19909563044449,0.0123949022594031,
-0.00883230825180998));
#42388=CARTESIAN_POINT('Ctrl Pts',(-0.199093476999217,0.0123970336359197,
-0.00883112407722527));
#42389=CARTESIAN_POINT('Ctrl Pts',(-0.199091315089946,0.0123991048910834,
-0.00882985186299045));
#42390=CARTESIAN_POINT('Ctrl Pts',(-0.199090551565165,0.0123998542387891,
-0.00882937949458529));
#42391=CARTESIAN_POINT('Ctrl Pts',(-0.200358957134347,0.00217086150225239,
-0.00857490676916749));
#42392=CARTESIAN_POINT('Ctrl Pts',(-0.200256928145031,0.00216031997502484,
-0.00856769265384055));
#42393=CARTESIAN_POINT('Ctrl Pts',(-0.200259634891842,0.00221877287151093,
-0.00848313450138094));
#42394=CARTESIAN_POINT('Ctrl Pts',(-0.200221663577824,0.0030168279086254,
-0.00915662824964644));
#42395=CARTESIAN_POINT('Ctrl Pts',(-0.200119977026507,0.00300268251391842,
-0.00914910188724964));
#42396=CARTESIAN_POINT('Ctrl Pts',(-0.200122930091165,0.0030520580293655,
-0.00905821337665723));
#42397=CARTESIAN_POINT('Ctrl Pts',(-0.199946837716981,0.00490697429828446,
-0.0100396594974494));
#42398=CARTESIAN_POINT('Ctrl Pts',(-0.199843194595014,0.0049071499232358,
-0.0100421011877827));
#42399=CARTESIAN_POINT('Ctrl Pts',(-0.199846517101214,0.00493537109414294,
-0.00994133786826413));
#42400=CARTESIAN_POINT('Ctrl Pts',(-0.200159811015846,0.00699125895088654,
-0.0102749556173087));
#42401=CARTESIAN_POINT('Ctrl Pts',(-0.200057531776169,0.00700151354044847,
-0.0102748800528092));
#42402=CARTESIAN_POINT('Ctrl Pts',(-0.200060976277344,0.00700707046734485,
-0.0101716158500798));
#42403=CARTESIAN_POINT('Ctrl Pts',(-0.2002437246959,0.0080221462246762,
-0.0102185853555578));
#42404=CARTESIAN_POINT('Ctrl Pts',(-0.200141219699188,0.00803052476732281,
-0.0102175393390583));
#42405=CARTESIAN_POINT('Ctrl Pts',(-0.200144640779559,0.00802464727946508,
-0.0101149279193058));
#42406=CARTESIAN_POINT('Ctrl Pts',(-0.200288491918007,0.00260606732410401,
-0.00885652097176724));
#42407=CARTESIAN_POINT('Ctrl Pts',(-0.200287495201655,0.00260681778558282,
-0.0088569600240947));
#42408=CARTESIAN_POINT('Ctrl Pts',(-0.200284717053799,0.00260886972400836,
-0.00885812502365241));
#42409=CARTESIAN_POINT('Ctrl Pts',(-0.200281945029545,0.00261098644985002,
-0.00885920566089888));
#42410=CARTESIAN_POINT('Ctrl Pts',(-0.200272773111516,0.0026182905132756,
-0.00886285415940844));
#42411=CARTESIAN_POINT('Ctrl Pts',(-0.200260149063117,0.00262859824983106,
-0.00886708771969354));
#42412=CARTESIAN_POINT('Ctrl Pts',(-0.200234736915584,0.00265262420116412,
-0.00887052425754006));
#42413=CARTESIAN_POINT('Ctrl Pts',(-0.200223688245904,0.00266407875563347,
-0.00887039745452822));
#42414=CARTESIAN_POINT('Ctrl Pts',(-0.200203089431465,0.0026882458772359,
-0.00886562944497509));
#42415=CARTESIAN_POINT('Ctrl Pts',(-0.200194400332019,0.00270014366015399,
-0.00886087059012383));
#42416=CARTESIAN_POINT('Ctrl Pts',(-0.200184181192038,0.0027174899119063,
-0.00884987271924794));
#42417=CARTESIAN_POINT('Ctrl Pts',(-0.200181042299458,0.00272390595868316,
-0.00884474249216518));
#42418=CARTESIAN_POINT('Ctrl Pts',(-0.200177292150585,0.0027347729314724,
-0.00883346936644047));
#42419=CARTESIAN_POINT('Ctrl Pts',(-0.200176401505629,0.00273925043048663,
-0.00882774489291586));
#42420=CARTESIAN_POINT('Ctrl Pts',(-0.200176428288968,0.00274311030530121,
-0.00882150516518164));
#42421=CARTESIAN_POINT('Ctrl Pts',(-0.199153925914828,0.0128366821545121,
-0.00854669799338706));
#42422=CARTESIAN_POINT('Ctrl Pts',(-0.199259867331971,0.012830442499507,
-0.00856126082459914));
#42423=CARTESIAN_POINT('Ctrl Pts',(-0.199260848897657,0.0127697866181808,
-0.00847297835399615));
#42424=CARTESIAN_POINT('Ctrl Pts',(-0.199014566784101,0.0119891616218098,
-0.00912886879878308));
#42425=CARTESIAN_POINT('Ctrl Pts',(-0.199120147481746,0.0119784757991412,
-0.00914424112649619));
#42426=CARTESIAN_POINT('Ctrl Pts',(-0.199121380077652,0.0119273408354419,
-0.00904935391227361));
#42427=CARTESIAN_POINT('Ctrl Pts',(-0.198742265564451,0.0100930977349455,
-0.0100137054011551));
#42428=CARTESIAN_POINT('Ctrl Pts',(-0.198849884594932,0.0100958392977007,
-0.0100193912995539));
#42429=CARTESIAN_POINT('Ctrl Pts',(-0.198851531194117,0.0100664774230896,
-0.00991443863121942));
#42430=CARTESIAN_POINT('Ctrl Pts',(-0.198952781415296,0.00800322977916761,
-0.0102479430315782));
#42431=CARTESIAN_POINT('Ctrl Pts',(-0.199058955570973,0.00801411281887282,
-0.0102566155570904));
#42432=CARTESIAN_POINT('Ctrl Pts',(-0.199060703267466,0.00800821003159929,
-0.0101489980208889));
#42433=CARTESIAN_POINT('Ctrl Pts',(-0.19903599944403,0.00697025739231732,
-0.010190711247955));
#42434=CARTESIAN_POINT('Ctrl Pts',(-0.199142399146872,0.00697843276992515,
-0.0102002818600052));
#42435=CARTESIAN_POINT('Ctrl Pts',(-0.199144128826406,0.00698446519833132,
-0.0100933452087197));
#42436=CARTESIAN_POINT('Ctrl Pts',(-0.19910085411519,0.00750164267895669,
-0.0101077379174169));
#42437=CARTESIAN_POINT('Ctrl Pts',(-0.199100690234321,0.00750164386369201,
-0.0101141870486527));
#42438=CARTESIAN_POINT('Ctrl Pts',(-0.199099900425191,0.00750164529645312,
-0.010120604956208));
#42439=CARTESIAN_POINT('Ctrl Pts',(-0.199096980593123,0.00750164874874024,
-0.0101336953338829));
#42440=CARTESIAN_POINT('Ctrl Pts',(-0.199094758035115,0.00750165079589565,
-0.0101403110956162));
#42441=CARTESIAN_POINT('Ctrl Pts',(-0.199086511791722,0.0075016572640334,
-0.010158357677076));
#42442=CARTESIAN_POINT('Ctrl Pts',(-0.19907894146395,0.00750166216143604,
-0.0101689261079603));
#42443=CARTESIAN_POINT('Ctrl Pts',(-0.199060209203537,0.00750167281253752,
-0.0101866208178074));
#42444=CARTESIAN_POINT('Ctrl Pts',(-0.199049221031088,0.0075016784662638,
-0.0101935805231524));
#42445=CARTESIAN_POINT('Ctrl Pts',(-0.199020116024875,0.00750169222744614,
-0.0102049685859948));
#42446=CARTESIAN_POINT('Ctrl Pts',(-0.199005661662064,0.00750168698491313,
-0.010205289239491));
#42447=CARTESIAN_POINT('Ctrl Pts',(-0.198998826136759,0.00750170224290608,
-0.0102051799706931));
#42448=CARTESIAN_POINT('Ctrl Pts',(-0.198998273076492,0.00750170106245327,
-0.0102051689708856));
#42449=CARTESIAN_POINT('Origin',(-0.199015196624372,0.00265663137285891,
-0.00874521521192296));
#42450=CARTESIAN_POINT('Ctrl Pts',(-0.199174969366088,0.0027425015311611,
-0.00880006183795226));
#42451=CARTESIAN_POINT('Ctrl Pts',(-0.199174842813697,0.00273849810823364,
-0.00880671010323751));
#42452=CARTESIAN_POINT('Ctrl Pts',(-0.199173925414073,0.0027337733786718,
-0.00881278723753809));
#42453=CARTESIAN_POINT('Ctrl Pts',(-0.199170456542776,0.00272255592635832,
-0.00882423111370532));
#42454=CARTESIAN_POINT('Ctrl Pts',(-0.199167778418797,0.00271606601452812,
-0.00882929991919414));
#42455=CARTESIAN_POINT('Ctrl Pts',(-0.199159149072896,0.00269839144076132,
-0.00884000172480209));
#42456=CARTESIAN_POINT('Ctrl Pts',(-0.199152038592254,0.0026863648561937,
-0.00884440574954461));
#42457=CARTESIAN_POINT('Ctrl Pts',(-0.199135085380916,0.00266145267956537,
-0.00884834654768667));
#42458=CARTESIAN_POINT('Ctrl Pts',(-0.199125804136305,0.00264931689278553,
-0.00884788255368404));
#42459=CARTESIAN_POINT('Ctrl Pts',(-0.19910220100882,0.00262117554154459,
-0.00884201033625836));
#42460=CARTESIAN_POINT('Ctrl Pts',(-0.199090880396505,0.00260977142339133,
-0.00883512294598114));
#42461=CARTESIAN_POINT('Ctrl Pts',(-0.199087183615344,0.00260668440517497,
-0.00883328156483494));
#42462=CARTESIAN_POINT('Ctrl Pts',(-0.199086747113234,0.00260606094030435,
-0.00883290238784639));
#42463=CARTESIAN_POINT('Ctrl Pts',(-0.199086158459772,0.00260522462644416,
-0.00883239115011147));
#42464=CARTESIAN_POINT('Ctrl Pts',(-0.199085607015723,0.00260468401114808,
-0.00883205078672203));
#42465=CARTESIAN_POINT('Ctrl Pts',(-0.199255095029157,0.00223457912828636,
-0.00847572645168213));
#42466=CARTESIAN_POINT('Ctrl Pts',(-0.199254232558087,0.00217396135577984,
-0.00856408799862321));
#42467=CARTESIAN_POINT('Ctrl Pts',(-0.199148223548041,0.00216779022884886,
-0.00854967377101157));
#42468=CARTESIAN_POINT('Ctrl Pts',(-0.19911735452896,0.00307715138405225,
-0.00905153587025602));
#42469=CARTESIAN_POINT('Ctrl Pts',(-0.199116240561307,0.00302606428734341,
-0.00914649828133776));
#42470=CARTESIAN_POINT('Ctrl Pts',(-0.199010586552336,0.00301548895708846,
-0.00913127651739455));
#42471=CARTESIAN_POINT('Ctrl Pts',(-0.198849911128423,0.00493808762162639,
-0.00991542469109674));
#42472=CARTESIAN_POINT('Ctrl Pts',(-0.198848386136249,0.00490876839268646,
-0.0100204318585757));
#42473=CARTESIAN_POINT('Ctrl Pts',(-0.198740725122237,0.00491151346327143,
-0.010014816198803));
#42474=CARTESIAN_POINT('Ctrl Pts',(-0.199060248816942,0.00699530919792622,
-0.0101490071671049));
#42475=CARTESIAN_POINT('Ctrl Pts',(-0.19905862191434,0.00698943349787215,
-0.0102566707772468));
#42476=CARTESIAN_POINT('Ctrl Pts',(-0.19895240571383,0.00700041025111481,
-0.0102480788233023));
#42477=CARTESIAN_POINT('Ctrl Pts',(-0.199144551422616,0.00801857716988301,
-0.0100930718875589));
#42478=CARTESIAN_POINT('Ctrl Pts',(-0.19914294272733,0.00802463741471564,
-0.0102000519321202));
#42479=CARTESIAN_POINT('Ctrl Pts',(-0.19903650115962,0.00803290185070517,
-0.0101905476764064));
#42480=CARTESIAN_POINT('Ctrl Pts',(-0.198263029449118,0.0127889692553363,
-0.00844048161250917));
#42481=CARTESIAN_POINT('Ctrl Pts',(-0.198260630058131,0.0128473039681307,
-0.00852521985761382));
#42482=CARTESIAN_POINT('Ctrl Pts',(-0.198362723942519,0.0128364944620873,
-0.00853213005721722));
#42483=CARTESIAN_POINT('Ctrl Pts',(-0.198125476177104,0.0119543980606105,
-0.00901449391313416));
#42484=CARTESIAN_POINT('Ctrl Pts',(-0.198122828059934,0.0120036536706846,
-0.00910553515936531));
#42485=CARTESIAN_POINT('Ctrl Pts',(-0.198224578879579,0.011989235059393,
-0.00911273974707262));
#42486=CARTESIAN_POINT('Ctrl Pts',(-0.197849387608806,0.01006903040502,
-0.00989615586142495));
#42487=CARTESIAN_POINT('Ctrl Pts',(-0.197846373450675,0.0100972224232102,
-0.00999699320190778));
#42488=CARTESIAN_POINT('Ctrl Pts',(-0.197950089640886,0.0100974185995862,
-0.00999415824051916));
#42489=CARTESIAN_POINT('Ctrl Pts',(-0.198062621662617,0.00799661069352205,
-0.010126450478369));
#42490=CARTESIAN_POINT('Ctrl Pts',(-0.198059480886231,0.00800222051560605,
-0.0102297912470711));
#42491=CARTESIAN_POINT('Ctrl Pts',(-0.198161844756368,0.00801231207768851,
-0.0102294986091472));
#42492=CARTESIAN_POINT('Ctrl Pts',(-0.198145073126219,0.00697819839513995,
-0.0100702620522896));
#42493=CARTESIAN_POINT('Ctrl Pts',(-0.198141956591681,0.00697239573675233,
-0.0101729602259579));
#42494=CARTESIAN_POINT('Ctrl Pts',(-0.198244544135673,0.00698070459421834,
-0.0101736135490439));
#42495=CARTESIAN_POINT('Ctrl Pts',(-0.198101345636185,0.00750214469193914,
-0.0100848681354076));
#42496=CARTESIAN_POINT('Ctrl Pts',(-0.198101197751573,0.00750214617774456,
-0.0100914116445182));
#42497=CARTESIAN_POINT('Ctrl Pts',(-0.19810169497294,0.00750214739593405,
-0.0100979534963226));
#42498=CARTESIAN_POINT('Ctrl Pts',(-0.198104036775493,0.00750214932141574,
-0.0101112547620612));
#42499=CARTESIAN_POINT('Ctrl Pts',(-0.198105958320376,0.00750214998598784,
-0.0101179644113016));
#42500=CARTESIAN_POINT('Ctrl Pts',(-0.198113381212346,0.00750215091575145,
-0.0101363652889876));
#42501=CARTESIAN_POINT('Ctrl Pts',(-0.198120466534415,0.00750215035194178,
-0.0101472648747458));
#42502=CARTESIAN_POINT('Ctrl Pts',(-0.198138380559241,0.00750214695175643,
-0.010165787562833));
#42503=CARTESIAN_POINT('Ctrl Pts',(-0.198149043192216,0.00750214414783725,
-0.0101732364295918));
#42504=CARTESIAN_POINT('Ctrl Pts',(-0.198172674415732,0.00750213659454397,
-0.010183736844365));
#42505=CARTESIAN_POINT('Ctrl Pts',(-0.198185801028644,0.00750218604830201,
-0.0101867199827473));
#42506=CARTESIAN_POINT('Ctrl Pts',(-0.198198986950856,0.00750212258616043,
-0.0101871036401355));
#42507=CARTESIAN_POINT('Ctrl Pts',(-0.198199421593232,0.00750212627687263,
-0.0101871141587648));
#42508=CARTESIAN_POINT('Ctrl Pts',(-0.198179421976457,0.0122637107296257,
-0.00877800506024049));
#42509=CARTESIAN_POINT('Ctrl Pts',(-0.198179396344291,0.0122675886867059,
-0.00878429351810534));
#42510=CARTESIAN_POINT('Ctrl Pts',(-0.198180301295335,0.0122720932380238,
-0.00879005955512643));
#42511=CARTESIAN_POINT('Ctrl Pts',(-0.198184108465672,0.0122830396599457,
-0.0088014133230424));
#42512=CARTESIAN_POINT('Ctrl Pts',(-0.198187295703864,0.01228950904073,
-0.00880657398770549));
#42513=CARTESIAN_POINT('Ctrl Pts',(-0.198197634790808,0.0123069503878714,
-0.0088175872800557));
#42514=CARTESIAN_POINT('Ctrl Pts',(-0.198206398292014,0.012318892994339,
-0.00882233127930981));
#42515=CARTESIAN_POINT('Ctrl Pts',(-0.19822773024133,0.012343816486207,
-0.00882717428033988));
#42516=CARTESIAN_POINT('Ctrl Pts',(-0.198239560095189,0.0123559532208523,
-0.00882713596148907));
#42517=CARTESIAN_POINT('Ctrl Pts',(-0.198269575746573,0.0123838978710278,
-0.00882248937213228));
#42518=CARTESIAN_POINT('Ctrl Pts',(-0.19828431706727,0.0123952751703846,
-0.00881620251558207));
#42519=CARTESIAN_POINT('Ctrl Pts',(-0.198289094376121,0.0123985489069097,
-0.00881443224052086));
#42520=CARTESIAN_POINT('Ctrl Pts',(-0.198289802981431,0.0123992211180763,
-0.00881404902421685));
#42521=CARTESIAN_POINT('Ctrl Pts',(-0.198290754893029,0.0124001206399054,
-0.00881353216580912));
#42522=CARTESIAN_POINT('Ctrl Pts',(-0.198291543142929,0.0124007144452265,
-0.00881318583917323));
#42523=CARTESIAN_POINT('Origin',(-0.198342362989776,0.0123486420924163,
-0.00872880441193628));
#42524=CARTESIAN_POINT('Ctrl Pts',(-0.197178980255201,0.0122642101438025,
-0.00875668392088435));
#42525=CARTESIAN_POINT('Ctrl Pts',(-0.197178856018515,0.0122681440730026,
-0.00876323575792611));
#42526=CARTESIAN_POINT('Ctrl Pts',(-0.197177965413713,0.0122727788823566,
-0.00876923608914849));
#42527=CARTESIAN_POINT('Ctrl Pts',(-0.19717459969814,0.0122837685448601,
-0.00878055600760033));
#42528=CARTESIAN_POINT('Ctrl Pts',(-0.197172003114716,0.0122901215768531,
-0.00878559056959148));
#42529=CARTESIAN_POINT('Ctrl Pts',(-0.197163568261289,0.0123075555926102,
-0.00879635605420354));
#42530=CARTESIAN_POINT('Ctrl Pts',(-0.197156564638062,0.0123194869785333,
-0.00880085511127768));
#42531=CARTESIAN_POINT('Ctrl Pts',(-0.197140243569857,0.0123436310953871,
-0.00880493069090822));
#42532=CARTESIAN_POINT('Ctrl Pts',(-0.197131571370146,0.0123551095223622,
-0.00880473298623716));
#42533=CARTESIAN_POINT('Ctrl Pts',(-0.197111374713174,0.0123796129489924,
-0.00880036789297042));
#42534=CARTESIAN_POINT('Ctrl Pts',(-0.197101653461885,0.0123898598822889,
-0.0087956602818417));
#42535=CARTESIAN_POINT('Ctrl Pts',(-0.197094772849081,0.0123970061969382,
-0.00879180261198509));
#42536=CARTESIAN_POINT('Ctrl Pts',(-0.197092611619732,0.0123991456177334,
-0.00879062001464486));
#42537=CARTESIAN_POINT('Ctrl Pts',(-0.197090441888492,0.0124012245213655,
-0.00878934849827443));
#42538=CARTESIAN_POINT('Ctrl Pts',(-0.197089683999265,0.0124019687088208,
-0.00878888148062584));
#42539=CARTESIAN_POINT('Ctrl Pts',(-0.198355740632463,0.00216798230497538,
-0.00853508005087582));
#42540=CARTESIAN_POINT('Ctrl Pts',(-0.198253891209442,0.00215756142816948,
-0.00852801123984347));
#42541=CARTESIAN_POINT('Ctrl Pts',(-0.198256371022465,0.00221569792273099,
-0.0084434712164535));
#42542=CARTESIAN_POINT('Ctrl Pts',(-0.198220012716574,0.00301557344026443,
-0.00911524185554709));
#42543=CARTESIAN_POINT('Ctrl Pts',(-0.198118497826422,0.00300159238337313,
-0.00910786031377932));
#42544=CARTESIAN_POINT('Ctrl Pts',(-0.198121225337493,0.00305067205412701,
-0.0090170397869099));
#42545=CARTESIAN_POINT('Ctrl Pts',(-0.197948601255717,0.00490772806496031,
-0.00999548097376579));
#42546=CARTESIAN_POINT('Ctrl Pts',(-0.19784517320138,0.00490797639378848,
-0.00999792585786736));
#42547=CARTESIAN_POINT('Ctrl Pts',(-0.197848267709436,0.00493603470329018,
-0.0098973401747785));
#42548=CARTESIAN_POINT('Ctrl Pts',(-0.198160921855801,0.00699217420993246,
-0.0102296850629028));
#42549=CARTESIAN_POINT('Ctrl Pts',(-0.198058837601862,0.0070023676241383,
-0.0102296245765728));
#42550=CARTESIAN_POINT('Ctrl Pts',(-0.198062056014678,0.00700790340885586,
-0.0101265584017485));
#42551=CARTESIAN_POINT('Ctrl Pts',(-0.198244664059479,0.00802338361730227,
-0.0101733946164067));
#42552=CARTESIAN_POINT('Ctrl Pts',(-0.198142357495407,0.00803173061364109,
-0.0101723737755292));
#42553=CARTESIAN_POINT('Ctrl Pts',(-0.198145551970183,0.0080258913884697,
-0.0100699536208949));
#42554=CARTESIAN_POINT('Ctrl Pts',(-0.198286052317126,0.00260395641848403,
-0.00881592224463899));
#42555=CARTESIAN_POINT('Ctrl Pts',(-0.198285052106862,0.002604711795387,
-0.00881636221563572));
#42556=CARTESIAN_POINT('Ctrl Pts',(-0.198282283015153,0.00260676363711584,
-0.00881752172403233));
#42557=CARTESIAN_POINT('Ctrl Pts',(-0.198279520069941,0.00260887968698758,
-0.0088185971915071));
#42558=CARTESIAN_POINT('Ctrl Pts',(-0.198270298464757,0.00261624321829764,
-0.00882225771182116));
#42559=CARTESIAN_POINT('Ctrl Pts',(-0.198257641167467,0.00262660986385978,
-0.00882648360551525));
#42560=CARTESIAN_POINT('Ctrl Pts',(-0.198232181686762,0.0026507514027741,
-0.00882985566173298));
#42561=CARTESIAN_POINT('Ctrl Pts',(-0.198221111224353,0.00266226369413246,
-0.00882968370958079));
#42562=CARTESIAN_POINT('Ctrl Pts',(-0.198200572555613,0.00268644702176355,
-0.00882479161107287));
#42563=CARTESIAN_POINT('Ctrl Pts',(-0.198191945617939,0.00269830091297626,
-0.00881998918431501));
#42564=CARTESIAN_POINT('Ctrl Pts',(-0.198181821514597,0.0027155505425809,
-0.00880895292975098));
#42565=CARTESIAN_POINT('Ctrl Pts',(-0.198178719887895,0.00272191486951209,
-0.00880382552404368));
#42566=CARTESIAN_POINT('Ctrl Pts',(-0.198175014888067,0.00273269000209349,
-0.0087925808302122));
#42567=CARTESIAN_POINT('Ctrl Pts',(-0.198174135307401,0.00273712881468879,
-0.00878687650525372));
#42568=CARTESIAN_POINT('Ctrl Pts',(-0.198174161532551,0.00274095524349409,
-0.00878066434858561));
#42569=CARTESIAN_POINT('Ctrl Pts',(-0.197152676116489,0.0128393614504822,
-0.00850713805088089));
#42570=CARTESIAN_POINT('Ctrl Pts',(-0.197258675429355,0.0128331580754525,
-0.00852166540087489));
#42571=CARTESIAN_POINT('Ctrl Pts',(-0.197259624390767,0.0127726713284735,
-0.00843320519526083));
#42572=CARTESIAN_POINT('Ctrl Pts',(-0.197014015809443,0.0119906110226541,
-0.0090873939546814));
#42573=CARTESIAN_POINT('Ctrl Pts',(-0.19711965698234,0.0119799690509704,
-0.00910273277093066));
#42574=CARTESIAN_POINT('Ctrl Pts',(-0.197120858311449,0.0119289913696173,
-0.00900770887161405));
#42575=CARTESIAN_POINT('Ctrl Pts',(-0.1967434320964,0.010093409573426,-0.0099690764507125));
#42576=CARTESIAN_POINT('Ctrl Pts',(-0.196851094172184,0.0100962166426703,
-0.00997479026530362));
#42577=CARTESIAN_POINT('Ctrl Pts',(-0.196852710184559,0.010066942105563,
-0.00986977505718237));
#42578=CARTESIAN_POINT('Ctrl Pts',(-0.196953826442827,0.00800423429314859,
-0.0102025203427104));
#42579=CARTESIAN_POINT('Ctrl Pts',(-0.197060050666728,0.00801510290894852,
-0.0102112192925465));
#42580=CARTESIAN_POINT('Ctrl Pts',(-0.197061768527618,0.00800920700147784,
-0.0101035551134565));
#42581=CARTESIAN_POINT('Ctrl Pts',(-0.197036943426159,0.00697129173689632,
-0.0101456507615118));
#42582=CARTESIAN_POINT('Ctrl Pts',(-0.19714339221939,0.00697946845198856,
-0.0101552416408534));
#42583=CARTESIAN_POINT('Ctrl Pts',(-0.197145091880529,0.00698546537262034,
-0.0100482517868171));
#42584=CARTESIAN_POINT('Ctrl Pts',(-0.197101862194412,0.00750262265417027,
-0.0100625703142549));
#42585=CARTESIAN_POINT('Ctrl Pts',(-0.197101697671371,0.00750262451484505,
-0.0100690155262311));
#42586=CARTESIAN_POINT('Ctrl Pts',(-0.197100907987531,0.00750262657291193,
-0.0100754295007868));
#42587=CARTESIAN_POINT('Ctrl Pts',(-0.197097989070983,0.00750263120389314,
-0.0100885160265501));
#42588=CARTESIAN_POINT('Ctrl Pts',(-0.197095766578603,0.00750263379167027,
-0.0100951317314081));
#42589=CARTESIAN_POINT('Ctrl Pts',(-0.197087520538495,0.00750264157329612,
-0.0101131782531217));
#42590=CARTESIAN_POINT('Ctrl Pts',(-0.197079950354737,0.00750264703705398,
-0.0101237467095286));
#42591=CARTESIAN_POINT('Ctrl Pts',(-0.197061218392508,0.00750265820233082,
-0.0101414414885696));
#42592=CARTESIAN_POINT('Ctrl Pts',(-0.197050230380519,0.00750266379358303,
-0.0101484012476249));
#42593=CARTESIAN_POINT('Ctrl Pts',(-0.197018045725239,0.00750267810501846,
-0.0101609946010674));
#42594=CARTESIAN_POINT('Ctrl Pts',(-0.197001295227288,0.00750267186841195,
-0.0101600242486746));
#42595=CARTESIAN_POINT('Ctrl Pts',(-0.196999724282808,0.00750269777634812,
-0.0101599991229918));
#42596=CARTESIAN_POINT('Ctrl Pts',(-0.196999282996544,0.00750268375780151,
-0.0101599899221715));
#42597=CARTESIAN_POINT('Origin',(-0.19701266044424,0.00265463512617686,
-0.0087047471371959));
#42598=CARTESIAN_POINT('Ctrl Pts',(-0.197176341115347,0.00274057713674786,
-0.00875946998943032));
#42599=CARTESIAN_POINT('Ctrl Pts',(-0.19717621449323,0.00273658033899075,
-0.00876613764532655));
#42600=CARTESIAN_POINT('Ctrl Pts',(-0.197175294731817,0.00273185885740524,
-0.00877223381232567));
#42601=CARTESIAN_POINT('Ctrl Pts',(-0.197171816455455,0.0027206414947534,
-0.0087837163247442));
#42602=CARTESIAN_POINT('Ctrl Pts',(-0.197169130834591,0.00271414787170457,
-0.0087888035389614));
#42603=CARTESIAN_POINT('Ctrl Pts',(-0.197160484426132,0.00269647084444689,
-0.0087995384357049));
#42604=CARTESIAN_POINT('Ctrl Pts',(-0.197153365839063,0.0026844444832896,
-0.00880395918817329));
#42605=CARTESIAN_POINT('Ctrl Pts',(-0.197136501486506,0.00265967921921435,
-0.00880790583160597));
#42606=CARTESIAN_POINT('Ctrl Pts',(-0.197127339136267,0.00264768562505251,
-0.0088074890418658));
#42607=CARTESIAN_POINT('Ctrl Pts',(-0.197104165460954,0.00261999057037431,
-0.00880186055873384));
#42608=CARTESIAN_POINT('Ctrl Pts',(-0.197093015487574,0.00260875339685481,
-0.00879526794355148));
#42609=CARTESIAN_POINT('Ctrl Pts',(-0.19708909427863,0.00260524930630241,
-0.00879321892863089));
#42610=CARTESIAN_POINT('Ctrl Pts',(-0.197088502629849,0.00260450913545116,
-0.00879277500053084));
#42611=CARTESIAN_POINT('Ctrl Pts',(-0.197087707786473,0.00260351927461845,
-0.00879217488636297));
#42612=CARTESIAN_POINT('Ctrl Pts',(-0.197087026280342,0.00260285013296824,
-0.00879175552978747));
#42613=CARTESIAN_POINT('Ctrl Pts',(-0.197256869972498,0.00223198241721985,
-0.00843619486098983));
#42614=CARTESIAN_POINT('Ctrl Pts',(-0.197256039653172,0.00217143518714522,
-0.00852488462310169));
#42615=CARTESIAN_POINT('Ctrl Pts',(-0.197149825227004,0.00216528939694016,
-0.00851026192212582));
#42616=CARTESIAN_POINT('Ctrl Pts',(-0.197118290041498,0.00307599018027203,
-0.00901018904184981));
#42617=CARTESIAN_POINT('Ctrl Pts',(-0.197117206671809,0.00302497917955987,
-0.00910545043129841));
#42618=CARTESIAN_POINT('Ctrl Pts',(-0.197011351483258,0.00301435832614128,
-0.00909000260578813));
#42619=CARTESIAN_POINT('Ctrl Pts',(-0.196850616071858,0.00493844615024685,
-0.00987108302336436));
#42620=CARTESIAN_POINT('Ctrl Pts',(-0.196849120143893,0.0049091727597524,
-0.00997633168506119));
#42621=CARTESIAN_POINT('Ctrl Pts',(-0.196741239182059,0.00491211626324586,
-0.00997054306786492));
#42622=CARTESIAN_POINT('Ctrl Pts',(-0.197061511162985,0.00699611927119618,
-0.0101037173049972));
#42623=CARTESIAN_POINT('Ctrl Pts',(-0.197059912250147,0.00699026221777102,
-0.0102116100519241));
#42624=CARTESIAN_POINT('Ctrl Pts',(-0.196953483034995,0.00700121689459126,
-0.010202788168383));
#42625=CARTESIAN_POINT('Ctrl Pts',(-0.19714541010813,0.00801971418708215,
-0.0100478527361994));
#42626=CARTESIAN_POINT('Ctrl Pts',(-0.197143829692753,0.00802577303021904,
-0.0101550639206471));
#42627=CARTESIAN_POINT('Ctrl Pts',(-0.19703717377299,0.00803402714762754,
-0.010145346940021));
#42628=CARTESIAN_POINT('Ctrl Pts',(-0.196261785015612,0.0127916962446281,
-0.00840096669647052));
#42629=CARTESIAN_POINT('Ctrl Pts',(-0.196259381274784,0.0128498400502766,
-0.00848583311340328));
#42630=CARTESIAN_POINT('Ctrl Pts',(-0.1963614813015,0.0128390750295401,
-0.00849268564311148));
#42631=CARTESIAN_POINT('Ctrl Pts',(-0.196124943532184,0.0119558621939739,
-0.00897306484675636));
#42632=CARTESIAN_POINT('Ctrl Pts',(-0.19612229019771,0.012004944437071,
-0.00906419088049844));
#42633=CARTESIAN_POINT('Ctrl Pts',(-0.196224049780035,0.0119905847978755,
-0.00907134057560896));
#42634=CARTESIAN_POINT('Ctrl Pts',(-0.195850337444749,0.0100694080936677,
-0.00985151727421576));
#42635=CARTESIAN_POINT('Ctrl Pts',(-0.195847316168474,0.0100974995137687,
-0.00995236546633424));
#42636=CARTESIAN_POINT('Ctrl Pts',(-0.195951025832399,0.0100977416688382,
-0.00994954663897551));
#42637=CARTESIAN_POINT('Ctrl Pts',(-0.196063688383263,0.00799749089638932,
-0.0100810227580311));
#42638=CARTESIAN_POINT('Ctrl Pts',(-0.196060540650448,0.00800308596337127,
-0.0101843566508062));
#42639=CARTESIAN_POINT('Ctrl Pts',(-0.196162901661524,0.0080131845991667,
-0.0101840741728357));
#42640=CARTESIAN_POINT('Ctrl Pts',(-0.196146246896505,0.00697929629222657,
-0.0100252005223376));
#42641=CARTESIAN_POINT('Ctrl Pts',(-0.19614312341995,0.00697352863131464,
-0.0101278980253559));
#42642=CARTESIAN_POINT('Ctrl Pts',(-0.196245707515403,0.00698184995272653,
-0.0101285582070294));
#42643=CARTESIAN_POINT('Ctrl Pts',(-0.196102466660209,0.00750312907896353,
-0.0100396915356686));
#42644=CARTESIAN_POINT('Ctrl Pts',(-0.196102318774524,0.00750313126710287,
-0.0100462350453267));
#42645=CARTESIAN_POINT('Ctrl Pts',(-0.196102815992879,0.00750313328765614,
-0.0100527768981209));
#42646=CARTESIAN_POINT('Ctrl Pts',(-0.196105157785642,0.00750313705085542,
-0.0100660781640112));
#42647=CARTESIAN_POINT('Ctrl Pts',(-0.196107079323156,0.00750313875719901,
-0.0100727878133388));
#42648=CARTESIAN_POINT('Ctrl Pts',(-0.196114502186249,0.00750314287748569,
-0.0100911886823653));
#42649=CARTESIAN_POINT('Ctrl Pts',(-0.196121587480966,0.00750314462020405,
-0.0101020882662016));
#42650=CARTESIAN_POINT('Ctrl Pts',(-0.196139501440965,0.00750314604761364,
-0.0101206109452192));
#42651=CARTESIAN_POINT('Ctrl Pts',(-0.196150164032413,0.00750314572377275,
-0.0101280598096453));
#42652=CARTESIAN_POINT('Ctrl Pts',(-0.196173794669146,0.00750314295768892,
-0.0101385599985622));
#42653=CARTESIAN_POINT('Ctrl Pts',(-0.196186921880472,0.00750331952577555,
-0.0101415431020705));
#42654=CARTESIAN_POINT('Ctrl Pts',(-0.196200104085276,0.00750312471114926,
-0.0101419269254443));
#42655=CARTESIAN_POINT('Ctrl Pts',(-0.196200541288955,0.00750313735745115,
-0.0101419375111811));
#42656=CARTESIAN_POINT('Ctrl Pts',(-0.196178618317942,0.0122657726141079,
-0.00873735943598018));
#42657=CARTESIAN_POINT('Ctrl Pts',(-0.196178593504016,0.0122696352114626,
-0.00874365008834643));
#42658=CARTESIAN_POINT('Ctrl Pts',(-0.196179497116263,0.0122741246939188,
-0.0087494203249196));
#42659=CARTESIAN_POINT('Ctrl Pts',(-0.196183298204856,0.0122850418366192,
-0.00876078948869322));
#42660=CARTESIAN_POINT('Ctrl Pts',(-0.196186480913547,0.0122914983868392,
-0.00876596141165356));
#42661=CARTESIAN_POINT('Ctrl Pts',(-0.196196807521002,0.0123089144864881,
-0.00877700827511887));
#42662=CARTESIAN_POINT('Ctrl Pts',(-0.196205561788726,0.0123208470597291,
-0.00878177623550929));
#42663=CARTESIAN_POINT('Ctrl Pts',(-0.196226774624743,0.0123456471402386,
-0.00878664780234662));
#42664=CARTESIAN_POINT('Ctrl Pts',(-0.196238473381177,0.0123576756480076,
-0.00878665704379384));
#42665=CARTESIAN_POINT('Ctrl Pts',(-0.196268052178449,0.0123853044299795,
-0.00878221469990786));
#42666=CARTESIAN_POINT('Ctrl Pts',(-0.196282603444165,0.0123965725498106,
-0.00877615578657818));
#42667=CARTESIAN_POINT('Ctrl Pts',(-0.196287641730374,0.0124001756233988,
-0.00877423853623206));
#42668=CARTESIAN_POINT('Ctrl Pts',(-0.196288528605167,0.0124009623318482,
-0.00877379890479523));
#42669=CARTESIAN_POINT('Ctrl Pts',(-0.196289718507424,0.0124020131242311,
-0.00877320367624877));
#42670=CARTESIAN_POINT('Ctrl Pts',(-0.196290669616441,0.0124027311765942,
-0.00877278680607922));
#42671=CARTESIAN_POINT('Origin',(-0.196341545593896,0.0123508451352711,
-0.00868829058453999));
#42672=CARTESIAN_POINT('Ctrl Pts',(-0.195178186257962,0.0122660193327441,
-0.00871622481824284));
#42673=CARTESIAN_POINT('Ctrl Pts',(-0.195178062117413,0.0122699395566604,
-0.00872278463078486));
#42674=CARTESIAN_POINT('Ctrl Pts',(-0.19517717113751,0.01227456152034,-0.00872879452985443));
#42675=CARTESIAN_POINT('Ctrl Pts',(-0.195173803716855,0.0122855263357825,
-0.00874013753178816));
#42676=CARTESIAN_POINT('Ctrl Pts',(-0.195171205718012,0.0122918678938226,
-0.00874518558968226));
#42677=CARTESIAN_POINT('Ctrl Pts',(-0.195162766091553,0.0123092764218653,
-0.00875598869146529));
#42678=CARTESIAN_POINT('Ctrl Pts',(-0.195155758242141,0.0123211961066292,
-0.00876051392612621));
#42679=CARTESIAN_POINT('Ctrl Pts',(-0.195139426702041,0.0123453268207502,
-0.00876464314654035));
#42680=CARTESIAN_POINT('Ctrl Pts',(-0.195130748768623,0.0123568030843096,
-0.00876447107949463));
#42681=CARTESIAN_POINT('Ctrl Pts',(-0.195110565284845,0.0123812771519621,
-0.00876016692235031));
#42682=CARTESIAN_POINT('Ctrl Pts',(-0.195100847936894,0.0123915253633481,
-0.0087554973074796));
#42683=CARTESIAN_POINT('Ctrl Pts',(-0.195093918061207,0.0123987217349169,
-0.00875163241365004));
#42684=CARTESIAN_POINT('Ctrl Pts',(-0.195091762741309,0.0124008562183796,
-0.00875045798311553));
#42685=CARTESIAN_POINT('Ctrl Pts',(-0.195089598961392,0.0124029310378485,
-0.00874919540157183));
#42686=CARTESIAN_POINT('Ctrl Pts',(-0.195088833371886,0.0124036830345601,
-0.00874872568289234));
#42687=CARTESIAN_POINT('Ctrl Pts',(-0.196360859055032,0.00216539872082755,
-0.0084957276445973));
#42688=CARTESIAN_POINT('Ctrl Pts',(-0.196258419764256,0.00215450188122847,
-0.00848894461062484));
#42689=CARTESIAN_POINT('Ctrl Pts',(-0.196261052500308,0.0022128124146575,
-0.00840377953460924));
#42690=CARTESIAN_POINT('Ctrl Pts',(-0.196223045774824,0.00301432493259675,
-0.00907396806990626));
#42691=CARTESIAN_POINT('Ctrl Pts',(-0.196120950035656,0.00299980977736295,
-0.00906689178531951));
#42692=CARTESIAN_POINT('Ctrl Pts',(-0.196123832235526,0.00304903240287206,
-0.00897545177118993));
#42693=CARTESIAN_POINT('Ctrl Pts',(-0.195949440420333,0.00490801871463543,
-0.00995116756051316));
#42694=CARTESIAN_POINT('Ctrl Pts',(-0.195845375145333,0.0049082851633093,
-0.00995414531367647));
#42695=CARTESIAN_POINT('Ctrl Pts',(-0.195848630152971,0.00493640698987308,
-0.00985293981030764));
#42696=CARTESIAN_POINT('Ctrl Pts',(-0.196162805580697,0.00699303769490664,
-0.0101844271380545));
#42697=CARTESIAN_POINT('Ctrl Pts',(-0.196060106214048,0.00700321707520669,
-0.0101848308040456));
#42698=CARTESIAN_POINT('Ctrl Pts',(-0.196063484599428,0.00700873741859737,
-0.0100811512250887));
#42699=CARTESIAN_POINT('Ctrl Pts',(-0.196246088270428,0.0080244759576494,
-0.010128210116568));
#42700=CARTESIAN_POINT('Ctrl Pts',(-0.196143162629668,0.0080328845270849,
-0.0101276651591394));
#42701=CARTESIAN_POINT('Ctrl Pts',(-0.19614651707733,0.00802701036852833,
-0.0100246338495604));
#42702=CARTESIAN_POINT('Ctrl Pts',(-0.196289742534361,0.00260194524226652,
-0.00877560306114225));
#42703=CARTESIAN_POINT('Ctrl Pts',(-0.196288786200047,0.00260266660909066,
-0.00877602123122052));
#42704=CARTESIAN_POINT('Ctrl Pts',(-0.196285968132903,0.00260474797982421,
-0.00877719370784045));
#42705=CARTESIAN_POINT('Ctrl Pts',(-0.196283156230408,0.00260689684470671,
-0.00877827782189942));
#42706=CARTESIAN_POINT('Ctrl Pts',(-0.196274251636572,0.0026140066765926,
-0.00878179470519303));
#42707=CARTESIAN_POINT('Ctrl Pts',(-0.196261536227681,0.00262436289230868,
-0.00878607841666256));
#42708=CARTESIAN_POINT('Ctrl Pts',(-0.196235746780876,0.00264877543324927,
-0.0087894236856269));
#42709=CARTESIAN_POINT('Ctrl Pts',(-0.196224650451408,0.00266029252809556,
-0.00878921975691903));
#42710=CARTESIAN_POINT('Ctrl Pts',(-0.196204084518718,0.00268445893936962,
-0.0087842549155602));
#42711=CARTESIAN_POINT('Ctrl Pts',(-0.196195454090691,0.0026962902459704,
-0.00877942124973539));
#42712=CARTESIAN_POINT('Ctrl Pts',(-0.196185330292752,0.00271349490247852,
-0.0087683461936074));
#42713=CARTESIAN_POINT('Ctrl Pts',(-0.196182229953234,0.00271983855251691,
-0.00876320809297492));
#42714=CARTESIAN_POINT('Ctrl Pts',(-0.196178527572347,0.00273057143602513,
-0.00875195367137863));
#42715=CARTESIAN_POINT('Ctrl Pts',(-0.196177648234497,0.00273498997121092,
-0.00874625028219231));
#42716=CARTESIAN_POINT('Ctrl Pts',(-0.196177672764501,0.00273879794676223,
-0.00874004230177787));
#42717=CARTESIAN_POINT('Ctrl Pts',(-0.195151512881996,0.0128416298218532,
-0.00846798718889344));
#42718=CARTESIAN_POINT('Ctrl Pts',(-0.195257533665328,0.0128354320026905,
-0.00848244732337054));
#42719=CARTESIAN_POINT('Ctrl Pts',(-0.195258449269627,0.0127751450299946,
-0.00839383594353875));
#42720=CARTESIAN_POINT('Ctrl Pts',(-0.195013512946357,0.0119916599223204,
-0.00904620160107736));
#42721=CARTESIAN_POINT('Ctrl Pts',(-0.195119177707696,0.0119810415291948,
-0.00906147061869671));
#42722=CARTESIAN_POINT('Ctrl Pts',(-0.195120346851283,0.0119302472688995,
-0.00896634073060416));
#42723=CARTESIAN_POINT('Ctrl Pts',(-0.19474419779016,0.0100934298404086,
-0.00992451520905792));
#42724=CARTESIAN_POINT('Ctrl Pts',(-0.194851869541245,0.0100962523749268,
-0.00993022299987102));
#42725=CARTESIAN_POINT('Ctrl Pts',(-0.194853453840199,0.0100670813731654,
-0.00982518221735306));
#42726=CARTESIAN_POINT('Ctrl Pts',(-0.194954744813264,0.00800503115987945,
-0.01015709544763));
#42727=CARTESIAN_POINT('Ctrl Pts',(-0.195060981356294,0.00801591560822246,
-0.0101657750852207));
#42728=CARTESIAN_POINT('Ctrl Pts',(-0.195062668194003,0.00801003144821768,
-0.0100581030663914));
#42729=CARTESIAN_POINT('Ctrl Pts',(-0.195038043104025,0.00697226031195997,
-0.0101005913568823));
#42730=CARTESIAN_POINT('Ctrl Pts',(-0.195144503954932,0.00698045989555377,
-0.0101101622792698));
#42731=CARTESIAN_POINT('Ctrl Pts',(-0.195146172454993,0.00698641929249386,
-0.0100031578282662));
#42732=CARTESIAN_POINT('Ctrl Pts',(-0.195102857644659,0.00750349585794822,
-0.0100174022791646));
#42733=CARTESIAN_POINT('Ctrl Pts',(-0.195102692485452,0.00750349828746446,
-0.0100238436041747));
#42734=CARTESIAN_POINT('Ctrl Pts',(-0.195101902927751,0.00750350069849524,
-0.0100302536786726));
#42735=CARTESIAN_POINT('Ctrl Pts',(-0.195098984922983,0.00750350560621888,
-0.0100433363955074));
#42736=CARTESIAN_POINT('Ctrl Pts',(-0.195096762496158,0.00750350808045609,
-0.01004995205496));
#42737=CARTESIAN_POINT('Ctrl Pts',(-0.19508851666777,0.00750351480991936,
-0.0100679985225843));
#42738=CARTESIAN_POINT('Ctrl Pts',(-0.195080946642692,0.0075035187252091,
-0.0100785670046555));
#42739=CARTESIAN_POINT('Ctrl Pts',(-0.195062215021252,0.00750352524311888,
-0.0100962618421349));
#42740=CARTESIAN_POINT('Ctrl Pts',(-0.195051227202046,0.00750352777528599,
-0.0101032216500095));
#42741=CARTESIAN_POINT('Ctrl Pts',(-0.195019265131039,0.00750353239339205,
-0.0101157282328778));
#42742=CARTESIAN_POINT('Ctrl Pts',(-0.195002697277718,0.00750350507918231,
-0.0101148512928373));
#42743=CARTESIAN_POINT('Ctrl Pts',(-0.19500072306832,0.00750355266323356,
-0.0101148197542948));
#42744=CARTESIAN_POINT('Ctrl Pts',(-0.195000280301755,0.00750353145507257,
-0.0101148105148487));
#42745=CARTESIAN_POINT('Origin',(-0.195016358203128,0.0026516719625554,
-0.00866391662495163));
#42746=CARTESIAN_POINT('Ctrl Pts',(-0.195178060704217,0.00273781719008554,
-0.00871849522740191));
#42747=CARTESIAN_POINT('Ctrl Pts',(-0.19517762418566,0.00272412448858684,
-0.00874143587971001));
#42748=CARTESIAN_POINT('Ctrl Pts',(-0.195163543470347,0.00269262426172652,
-0.00876037467869015));
#42749=CARTESIAN_POINT('Ctrl Pts',(-0.195146481811715,0.00266914690574364,
-0.00876512160782382));
#42750=CARTESIAN_POINT('Ctrl Pts',(-0.195130973719132,0.00264780730342053,
-0.00876943630067265));
#42751=CARTESIAN_POINT('Ctrl Pts',(-0.19511874958781,0.0026308641930614,
-0.0087672708333908));
#42752=CARTESIAN_POINT('Ctrl Pts',(-0.195095892349715,0.00260729719483703,
-0.0087551043908356));
#42753=CARTESIAN_POINT('Ctrl Pts',(-0.195093602562696,0.00260493630563481,
-0.00875388558381637));
#42754=CARTESIAN_POINT('Ctrl Pts',(-0.195091215951724,0.00260253308819682,
-0.00875252862861909));
#42755=CARTESIAN_POINT('Ctrl Pts',(-0.195088737224831,0.00260009358768204,
-0.00875100653258347));
#42756=CARTESIAN_POINT('Ctrl Pts',(-0.195258515249865,0.00222833195472316,
-0.00839606745134456));
#42757=CARTESIAN_POINT('Ctrl Pts',(-0.195257715261884,0.00216794822738603,
-0.00848493156407439));
#42758=CARTESIAN_POINT('Ctrl Pts',(-0.195151448734371,0.00216179672804389,
-0.00847031066803133));
#42759=CARTESIAN_POINT('Ctrl Pts',(-0.195120023433732,0.00307389698912644,
-0.00896847560096047));
#42760=CARTESIAN_POINT('Ctrl Pts',(-0.195118969009728,0.00302304055807606,
-0.00906387341398073));
#42761=CARTESIAN_POINT('Ctrl Pts',(-0.195013060612715,0.00301242429812119,
-0.00904843195044751));
#42762=CARTESIAN_POINT('Ctrl Pts',(-0.194853142386239,0.00493839989964462,
-0.00982675338910633));
#42763=CARTESIAN_POINT('Ctrl Pts',(-0.194851674310384,0.00490921859900544,
-0.00993206859484722));
#42764=CARTESIAN_POINT('Ctrl Pts',(-0.19474374897434,0.00491214826721647,
-0.00992622756956082));
#42765=CARTESIAN_POINT('Ctrl Pts',(-0.195062706736678,0.00699673232562924,
-0.0100584265394132));
#42766=CARTESIAN_POINT('Ctrl Pts',(-0.195061134895631,0.00699090164734755,
-0.0101663685336579));
#42767=CARTESIAN_POINT('Ctrl Pts',(-0.194954650496018,0.00700179905759746,
-0.0101575132200674));
#42768=CARTESIAN_POINT('Ctrl Pts',(-0.195146170526654,0.00802082773606981,
-0.0100026394254629));
#42769=CARTESIAN_POINT('Ctrl Pts',(-0.195144617516619,0.00802687470231159,
-0.0101099032731655));
#42770=CARTESIAN_POINT('Ctrl Pts',(-0.195037908039177,0.00803507912154476,
-0.0101001626767837));
#42771=CARTESIAN_POINT('Ctrl Pts',(-0.222249881326672,0.00687543454306065,
-0.010708608705939));
#42772=CARTESIAN_POINT('Ctrl Pts',(-0.222147507675063,0.00686704591829485,
-0.0107075587151972));
#42773=CARTESIAN_POINT('Ctrl Pts',(-0.22215063088296,0.00687429739500378,
-0.0106051559466831));
#42774=CARTESIAN_POINT('Ctrl Pts',(-0.22213303026492,0.00811344210707129,
-0.0107938596287791));
#42775=CARTESIAN_POINT('Ctrl Pts',(-0.222030943630378,0.00810248190675591,
-0.010794192368089));
#42776=CARTESIAN_POINT('Ctrl Pts',(-0.222034098562025,0.00809546126778267,
-0.0106907816028563));
#42777=CARTESIAN_POINT('Ctrl Pts',(-0.221994531826128,0.00993476248926103,
-0.0105419142089085));
#42778=CARTESIAN_POINT('Ctrl Pts',(-0.221891182125483,0.00993371370083797,
-0.0105441094985628));
#42779=CARTESIAN_POINT('Ctrl Pts',(-0.221894227111855,0.00990623992118876,
-0.0104434861240904));
#42780=CARTESIAN_POINT('Ctrl Pts',(-0.222202931566564,0.0122478622459772,
-0.00946095837100554));
#42781=CARTESIAN_POINT('Ctrl Pts',(-0.222101383624784,0.0122634552700619,
-0.00945277921907509));
#42782=CARTESIAN_POINT('Ctrl Pts',(-0.222103981254199,0.0122092535606527,
-0.00936466720929235));
#42783=CARTESIAN_POINT('Ctrl Pts',(-0.222503016192992,0.0132233862244586,
-0.00873138285702185));
#42784=CARTESIAN_POINT('Ctrl Pts',(-0.22240314604442,0.0132424080883783,
-0.00871654332699369));
#42785=CARTESIAN_POINT('Ctrl Pts',(-0.222405481336722,0.0131773681473555,
-0.00863664901956425));
#42786=CARTESIAN_POINT('Ctrl Pts',(-0.222649530248401,0.0137486960647823,
-0.00823639965487398));
#42787=CARTESIAN_POINT('Ctrl Pts',(-0.222548877010536,0.0137640118108876,
-0.00822249108542394));
#42788=CARTESIAN_POINT('Ctrl Pts',(-0.222551015132696,0.013692950370958,
-0.00814830722488945));
#42789=CARTESIAN_POINT('Ctrl Pts',(-0.222093148989078,0.00750347905706887,
-0.0106271011600294));
#42790=CARTESIAN_POINT('Ctrl Pts',(-0.222093001117879,0.00750348163845054,
-0.0106336437243019));
#42791=CARTESIAN_POINT('Ctrl Pts',(-0.222093498230638,0.00750348439599822,
-0.0106401846244798));
#42792=CARTESIAN_POINT('Ctrl Pts',(-0.222095839546678,0.00750349036668899,
-0.0106534840158653));
#42793=CARTESIAN_POINT('Ctrl Pts',(-0.222097760699624,0.0075034935809392,
-0.0106601927381583));
#42794=CARTESIAN_POINT('Ctrl Pts',(-0.222105182881688,0.00750350298274059,
-0.0106785933030817));
#42795=CARTESIAN_POINT('Ctrl Pts',(-0.222112268300804,0.00750350928445525,
-0.0106894933245119));
#42796=CARTESIAN_POINT('Ctrl Pts',(-0.222130183071353,0.00750352156683749,
-0.0107080173739093));
#42797=CARTESIAN_POINT('Ctrl Pts',(-0.222140846494675,0.00750352744091401,
-0.0107154669821436));
#42798=CARTESIAN_POINT('Ctrl Pts',(-0.222172223478591,0.00750354134005543,
-0.0107294102153455));
#42799=CARTESIAN_POINT('Ctrl Pts',(-0.222188823735049,0.00750357107008051,
-0.0107292797619568));
#42800=CARTESIAN_POINT('Ctrl Pts',(-0.22219077671284,0.00750352632614256,
-0.0107293370430334));
#42801=CARTESIAN_POINT('Ctrl Pts',(-0.222191219494722,0.00750354683273177,
-0.0107293478392253));
#42802=CARTESIAN_POINT('Ctrl Pts',(-0.222392848909985,0.013140240706079,
-0.0086347107226525));
#42803=CARTESIAN_POINT('Ctrl Pts',(-0.222392878685365,0.0131452498761335,
-0.00864065169899928));
#42804=CARTESIAN_POINT('Ctrl Pts',(-0.222394028589284,0.0131508377990427,
-0.00864589817563944));
#42805=CARTESIAN_POINT('Ctrl Pts',(-0.222398741299102,0.0131641425680373,
-0.00865593592085266));
#42806=CARTESIAN_POINT('Ctrl Pts',(-0.222402690636142,0.0131718061837692,
-0.00866018291654182));
#42807=CARTESIAN_POINT('Ctrl Pts',(-0.222415044365568,0.0131914856188858,
-0.00866832547181801));
#42808=CARTESIAN_POINT('Ctrl Pts',(-0.222425289775166,0.0132043797156318,
-0.00867097294064302));
#42809=CARTESIAN_POINT('Ctrl Pts',(-0.222448469021798,0.0132287804888377,
-0.00867124055874764));
#42810=CARTESIAN_POINT('Ctrl Pts',(-0.222460225938644,0.0132395460799034,
-0.00866944454699309));
#42811=CARTESIAN_POINT('Ctrl Pts',(-0.222488865700657,0.0132630567621544,
-0.00866184603742375));
#42812=CARTESIAN_POINT('Ctrl Pts',(-0.222502612807788,0.0132721998107884,
-0.00865561866607119));
#42813=CARTESIAN_POINT('Ctrl Pts',(-0.222508839896806,0.0132761722127939,
-0.00865279538552127));
#42814=CARTESIAN_POINT('Ctrl Pts',(-0.222511979440178,0.0132782693982421,
-0.00865128616260161));
#42815=CARTESIAN_POINT('Ctrl Pts',(-0.222515313566668,0.0132804052496997,
-0.00864958136878297));
#42816=CARTESIAN_POINT('Origin',(-0.222557069576793,0.0132165166889543,
-0.00857342793229397));
#42817=CARTESIAN_POINT('Ctrl Pts',(-0.221393342144309,0.013140302186429,
-0.00861407581869929));
#42818=CARTESIAN_POINT('Ctrl Pts',(-0.221392512653964,0.0131790082731684,
-0.00866137407639872));
#42819=CARTESIAN_POINT('Ctrl Pts',(-0.221357898020299,0.0132523373781119,
-0.00865122754666828));
#42820=CARTESIAN_POINT('Ctrl Pts',(-0.221311658118836,0.0132815271509267,
-0.00862621264935379));
#42821=CARTESIAN_POINT('Ctrl Pts',(-0.22215041348331,0.0081317000139514,
-0.010604324930572));
#42822=CARTESIAN_POINT('Ctrl Pts',(-0.222146866536432,0.00813909558534202,
-0.0107072984786383));
#42823=CARTESIAN_POINT('Ctrl Pts',(-0.222249835659344,0.00813070245192706,
-0.0107081718331986));
#42824=CARTESIAN_POINT('Ctrl Pts',(-0.222033898159491,0.00691248699556566,
-0.0106906639957997));
#42825=CARTESIAN_POINT('Ctrl Pts',(-0.222030320528098,0.00690556431974724,
-0.0107946638061863));
#42826=CARTESIAN_POINT('Ctrl Pts',(-0.222133004724419,0.00689459044374911,
-0.0107941464062241));
#42827=CARTESIAN_POINT('Ctrl Pts',(-0.2218981179966,0.00510426517379774,
-0.0104455594933188));
#42828=CARTESIAN_POINT('Ctrl Pts',(-0.221894644006361,0.00507676318916403,
-0.0105467911269829));
#42829=CARTESIAN_POINT('Ctrl Pts',(-0.221998582688886,0.00507586896512953,
-0.0105444525401242));
#42830=CARTESIAN_POINT('Ctrl Pts',(-0.222106568628605,0.00280338838995331,
-0.00937174878353225));
#42831=CARTESIAN_POINT('Ctrl Pts',(-0.222103550983437,0.00274895782721167,
-0.00946041018195773));
#42832=CARTESIAN_POINT('Ctrl Pts',(-0.222205687874948,0.00276476336427084,
-0.00946845290383881));
#42833=CARTESIAN_POINT('Ctrl Pts',(-0.222411478982832,0.00183582509294618,
-0.00864683768561999));
#42834=CARTESIAN_POINT('Ctrl Pts',(-0.222408729806004,0.001770486407663,
-0.00872724372961482));
#42835=CARTESIAN_POINT('Ctrl Pts',(-0.222509093970282,0.00179005747630213,
-0.00874221305404969));
#42836=CARTESIAN_POINT('Ctrl Pts',(-0.222558531085189,0.00132037684913637,
-0.00816064415141273));
#42837=CARTESIAN_POINT('Ctrl Pts',(-0.222555975148884,0.00124900577222267,
-0.00823534029207931));
#42838=CARTESIAN_POINT('Ctrl Pts',(-0.222657166444787,0.00126470219399182,
-0.00824931224599372));
#42839=CARTESIAN_POINT('Ctrl Pts',(-0.222519811891068,0.00173281601266729,
-0.00866059802620759));
#42840=CARTESIAN_POINT('Ctrl Pts',(-0.222519711787491,0.00173312127539872,
-0.00866084823972965));
#42841=CARTESIAN_POINT('Ctrl Pts',(-0.222519594558049,0.00173330438501034,
-0.00866099618213166));
#42842=CARTESIAN_POINT('Ctrl Pts',(-0.222519140601718,0.00173381349151495,
-0.00866140162405847));
#42843=CARTESIAN_POINT('Ctrl Pts',(-0.222518709616375,0.00173417891196423,
-0.00866168844501488));
#42844=CARTESIAN_POINT('Ctrl Pts',(-0.222517104151076,0.00173536521354638,
-0.00866259377003072));
#42845=CARTESIAN_POINT('Ctrl Pts',(-0.222515819635713,0.00173622911476649,
-0.00866323065497129));
#42846=CARTESIAN_POINT('Ctrl Pts',(-0.222511061100675,0.00173943859314526,
-0.00866552948731959));
#42847=CARTESIAN_POINT('Ctrl Pts',(-0.222503603668941,0.00174438148073145,
-0.00866891690307697));
#42848=CARTESIAN_POINT('Ctrl Pts',(-0.222475754872163,0.00176507779554153,
-0.00867887860705707));
#42849=CARTESIAN_POINT('Ctrl Pts',(-0.222458582137689,0.00178014243579629,
-0.00868222267468587));
#42850=CARTESIAN_POINT('Ctrl Pts',(-0.222431452624928,0.00180853115651544,
-0.00868199708331077));
#42851=CARTESIAN_POINT('Ctrl Pts',(-0.222421094900015,0.0018214782425271,
-0.00867936980954872));
#42852=CARTESIAN_POINT('Ctrl Pts',(-0.22240857660096,0.00184126011996096,
-0.00867122308273688));
#42853=CARTESIAN_POINT('Ctrl Pts',(-0.222404561479792,0.00184898184210888,
-0.00866695439586749));
#42854=CARTESIAN_POINT('Ctrl Pts',(-0.222399771942874,0.00186237598235397,
-0.00865684643894828));
#42855=CARTESIAN_POINT('Ctrl Pts',(-0.222398602189169,0.00186799481674966,
-0.00865156303303412));
#42856=CARTESIAN_POINT('Ctrl Pts',(-0.222398570120677,0.0018730271297317,
-0.008645575543849));
#42857=CARTESIAN_POINT('Ctrl Pts',(-0.221150464830925,0.00688034370022854,
-0.010582553178107));
#42858=CARTESIAN_POINT('Ctrl Pts',(-0.221149540493208,0.00687264310985869,
-0.0106927174515397));
#42859=CARTESIAN_POINT('Ctrl Pts',(-0.221040105820209,0.00686441410916952,
-0.0106801811534307));
#42860=CARTESIAN_POINT('Ctrl Pts',(-0.221032681327501,0.00810843535542784,
-0.0106668215581535));
#42861=CARTESIAN_POINT('Ctrl Pts',(-0.221031730409529,0.00811613590506075,
-0.0107780620582133));
#42862=CARTESIAN_POINT('Ctrl Pts',(-0.220922572418371,0.00810366232374963,
-0.0107669088928184));
#42863=CARTESIAN_POINT('Ctrl Pts',(-0.220896606320941,0.00990275697441929,
-0.0104177217566761));
#42864=CARTESIAN_POINT('Ctrl Pts',(-0.220895748847351,0.009932200154217,
-0.0105259351302228));
#42865=CARTESIAN_POINT('Ctrl Pts',(-0.220785304732471,0.00992817015338086,
-0.0105169648004527));
#42866=CARTESIAN_POINT('Ctrl Pts',(-0.221099708280645,0.0121797433482338,
-0.00935944466440972));
#42867=CARTESIAN_POINT('Ctrl Pts',(-0.221099353535905,0.0122375562745181,
-0.00945449197733792));
#42868=CARTESIAN_POINT('Ctrl Pts',(-0.220990602690162,0.0122475181246042,
-0.00943636041410781));
#42869=CARTESIAN_POINT('Ctrl Pts',(-0.221395176166451,0.0131433495521379,
-0.00864446468980765));
#42870=CARTESIAN_POINT('Ctrl Pts',(-0.221395137837132,0.0132127320462371,
-0.00873085305611693));
#42871=CARTESIAN_POINT('Ctrl Pts',(-0.221288309650929,0.0132261159542827,
-0.00870596282060123));
#42872=CARTESIAN_POINT('Ctrl Pts',(-0.221544135263697,0.0136675288337307,
-0.00815436056670324));
#42873=CARTESIAN_POINT('Ctrl Pts',(-0.221544294911465,0.0137435040814762,
-0.00823459311628976));
#42874=CARTESIAN_POINT('Ctrl Pts',(-0.221436574138446,0.0137519902155352,
-0.0082114432028954));
#42875=CARTESIAN_POINT('Ctrl Pts',(-0.221093381485671,0.00750288700333877,
-0.0106049435316979));
#42876=CARTESIAN_POINT('Ctrl Pts',(-0.22109320880867,0.00750288906317748,
-0.0106113416698315));
#42877=CARTESIAN_POINT('Ctrl Pts',(-0.221092419982598,0.00750289094644645,
-0.0106177083341688));
#42878=CARTESIAN_POINT('Ctrl Pts',(-0.221089509680449,0.0075028944558648,
-0.0106307512649));
#42879=CARTESIAN_POINT('Ctrl Pts',(-0.22108728565415,0.00750289603503224,
-0.0106373687796944));
#42880=CARTESIAN_POINT('Ctrl Pts',(-0.221079035395588,0.00750289975374608,
-0.0106554166409915));
#42881=CARTESIAN_POINT('Ctrl Pts',(-0.221071462762515,0.00750290119227914,
-0.0106659843001971));
#42882=CARTESIAN_POINT('Ctrl Pts',(-0.221052726190283,0.0075029019784618,
-0.0106836767790163));
#42883=CARTESIAN_POINT('Ctrl Pts',(-0.221041736012401,0.00750290130802815,
-0.0106906350161983));
#42884=CARTESIAN_POINT('Ctrl Pts',(-0.221016461332956,0.00750289787870694,
-0.0107005197427617));
#42885=CARTESIAN_POINT('Ctrl Pts',(-0.221003806041523,0.00750288073417112,
-0.0107022177264459));
#42886=CARTESIAN_POINT('Ctrl Pts',(-0.220992863211399,0.00750289680848803,
-0.0107022436617203));
#42887=CARTESIAN_POINT('Ctrl Pts',(-0.220992438489933,0.00750289754619727,
-0.0107022417574986));
#42888=CARTESIAN_POINT('Ctrl Pts',(-0.220991844919555,0.0075029014952033,
-0.0107022357170612));
#42889=CARTESIAN_POINT('Ctrl Pts',(-0.220991596752038,0.00750290355364233,
-0.0107022324043892));
#42890=CARTESIAN_POINT('Ctrl Pts',(-0.220991244605229,0.00750291318074831,
-0.0107022266022728));
#42891=CARTESIAN_POINT('Ctrl Pts',(-0.220990866858029,0.00750300510925417,
-0.0107022189130647));
#42892=CARTESIAN_POINT('Origin',(-0.221237471898473,0.00179552890401392,
-0.0085587796007864));
#42893=CARTESIAN_POINT('Ctrl Pts',(-0.221399010012836,0.00187318766792258,
-0.00862507770872998));
#42894=CARTESIAN_POINT('Ctrl Pts',(-0.221398907349878,0.00186835774631689,
-0.00863100475221132));
#42895=CARTESIAN_POINT('Ctrl Pts',(-0.22139810388374,0.00186290294648796,
-0.0086362961021297));
#42896=CARTESIAN_POINT('Ctrl Pts',(-0.221395045281478,0.00185039344029363,
-0.00864594208587137));
#42897=CARTESIAN_POINT('Ctrl Pts',(-0.221392681904453,0.0018433694093753,
-0.00865003605187046));
#42898=CARTESIAN_POINT('Ctrl Pts',(-0.221384736880726,0.00182393207571952,
-0.00865848009275339));
#42899=CARTESIAN_POINT('Ctrl Pts',(-0.221378173054657,0.0018113553860032,
-0.00866102038332009));
#42900=CARTESIAN_POINT('Ctrl Pts',(-0.221363548830083,0.00178732269172333,
-0.00866159342441401));
#42901=CARTESIAN_POINT('Ctrl Pts',(-0.2213555333964,0.00177585407827663,
-0.00865973428883798));
#42902=CARTESIAN_POINT('Ctrl Pts',(-0.221335870803864,0.00175074374557391,
-0.00865135187979251));
#42903=CARTESIAN_POINT('Ctrl Pts',(-0.22132649230484,0.00174100645599888,
-0.00864446213309051));
#42904=CARTESIAN_POINT('Ctrl Pts',(-0.22132190932138,0.00173649085409544,
-0.00864108723501383));
#42905=CARTESIAN_POINT('Ctrl Pts',(-0.221319832849445,0.0017343171811537,
-0.00863944412245893));
#42906=CARTESIAN_POINT('Ctrl Pts',(-0.221317763839132,0.00173223151638979,
-0.00863769727779015));
#42907=CARTESIAN_POINT('Ctrl Pts',(-0.221317525382339,0.00173199991205511,
-0.00863750196330413));
#42908=CARTESIAN_POINT('Ctrl Pts',(-0.221039493952704,0.00814028259742471,
-0.0106798048749903));
#42909=CARTESIAN_POINT('Ctrl Pts',(-0.221149177384937,0.00813212789921885,
-0.0106927176453606));
#42910=CARTESIAN_POINT('Ctrl Pts',(-0.221150165198724,0.00812434479483271,
-0.010582274352994));
#42911=CARTESIAN_POINT('Ctrl Pts',(-0.220922252472739,0.00690325684720192,
-0.0107670349642513));
#42912=CARTESIAN_POINT('Ctrl Pts',(-0.22103166212434,0.00689077782194489,
-0.0107785678254041));
#42913=CARTESIAN_POINT('Ctrl Pts',(-0.221032676501381,0.00689840577890317,
-0.0106670390937617));
#42914=CARTESIAN_POINT('Ctrl Pts',(-0.220788221206417,0.00508184180165128,
-0.0105191990487672));
#42915=CARTESIAN_POINT('Ctrl Pts',(-0.220898905314294,0.00507784583507543,
-0.0105285860406717));
#42916=CARTESIAN_POINT('Ctrl Pts',(-0.22089982808778,0.00510723661303933,
-0.0104200629949558));
#42917=CARTESIAN_POINT('Ctrl Pts',(-0.22099337460045,0.00276507260651043,
-0.00944375885445184));
#42918=CARTESIAN_POINT('Ctrl Pts',(-0.221102369107793,0.00277493695513631,
-0.00946223082472947));
#42919=CARTESIAN_POINT('Ctrl Pts',(-0.221102788022272,0.00283275709507392,
-0.00936685532907095));
#42920=CARTESIAN_POINT('Ctrl Pts',(-0.221293701763668,0.00178742795253052,
-0.00871679057028318));
#42921=CARTESIAN_POINT('Ctrl Pts',(-0.221400695380101,0.00180094083600155,
-0.00874219231644764));
#42922=CARTESIAN_POINT('Ctrl Pts',(-0.221400797118254,0.00187034626191687,
-0.00865545652030308));
#42923=CARTESIAN_POINT('Ctrl Pts',(-0.221443367427878,0.00126174482639335,
-0.00822459051870288));
#42924=CARTESIAN_POINT('Ctrl Pts',(-0.221551288994416,0.00127019986002699,
-0.00824817907764156));
#42925=CARTESIAN_POINT('Ctrl Pts',(-0.221551195199306,0.00134620621622744,
-0.00816758272347228));
#42926=CARTESIAN_POINT('Ctrl Pts',(-0.220250306618512,0.0068767635851955,
-0.0106635861607493));
#42927=CARTESIAN_POINT('Ctrl Pts',(-0.220147856493154,0.00686835894786593,
-0.0106626255349507));
#42928=CARTESIAN_POINT('Ctrl Pts',(-0.220150969995606,0.00687557763149086,
-0.0105601412393206));
#42929=CARTESIAN_POINT('Ctrl Pts',(-0.220133883086356,0.00811004854082277,
-0.0107480074268753));
#42930=CARTESIAN_POINT('Ctrl Pts',(-0.220031713557015,0.00809906691085948,
-0.0107484381821638));
#42931=CARTESIAN_POINT('Ctrl Pts',(-0.22003485851762,0.00809210119000192,
-0.0106449585226562));
#42932=CARTESIAN_POINT('Ctrl Pts',(-0.219995660265109,0.00992369026213599,
-0.0104991498138423));
#42933=CARTESIAN_POINT('Ctrl Pts',(-0.21989225493449,0.00992270949191421,
-0.0105013643797054));
#42934=CARTESIAN_POINT('Ctrl Pts',(-0.21989529130248,0.00989542327015895,
-0.0104006294419025));
#42935=CARTESIAN_POINT('Ctrl Pts',(-0.220201022339521,0.0122315251788832,
-0.00942943555407081));
#42936=CARTESIAN_POINT('Ctrl Pts',(-0.220099353543913,0.012246971481956,
-0.00942151978304597));
#42937=CARTESIAN_POINT('Ctrl Pts',(-0.220101943743354,0.012193078903321,
-0.00933313831981191));
#42938=CARTESIAN_POINT('Ctrl Pts',(-0.220498643283846,0.013206679346764,
-0.00870682343419975));
#42939=CARTESIAN_POINT('Ctrl Pts',(-0.220398717237275,0.0132259390201395,
-0.00869206884376114));
#42940=CARTESIAN_POINT('Ctrl Pts',(-0.220401045442068,0.0131612261295782,
-0.00861181318161109));
#42941=CARTESIAN_POINT('Ctrl Pts',(-0.220645208974285,0.0137320975088836,
-0.0082169211442826));
#42942=CARTESIAN_POINT('Ctrl Pts',(-0.220544466885696,0.0137474970413183,
-0.00820318515944086));
#42943=CARTESIAN_POINT('Ctrl Pts',(-0.22054659976056,0.0136767805992873,
-0.00812856487265608));
#42944=CARTESIAN_POINT('Ctrl Pts',(-0.220093677111814,0.00750238403012091,
-0.0105819118104658));
#42945=CARTESIAN_POINT('Ctrl Pts',(-0.220093529239301,0.00750238578936402,
-0.0105884544159041));
#42946=CARTESIAN_POINT('Ctrl Pts',(-0.220094026363594,0.00750238771684917,
-0.0105949953563592));
#42947=CARTESIAN_POINT('Ctrl Pts',(-0.220096367729295,0.00750239198187957,
-0.0106082948310363));
#42948=CARTESIAN_POINT('Ctrl Pts',(-0.220098288922505,0.00750239432577211,
-0.0106150035930982));
#42949=CARTESIAN_POINT('Ctrl Pts',(-0.220105711231248,0.00750240130929248,
-0.0106334041999022));
#42950=CARTESIAN_POINT('Ctrl Pts',(-0.220112796740053,0.00750240614050839,
-0.0106443042059039));
#42951=CARTESIAN_POINT('Ctrl Pts',(-0.220130711695223,0.00750241582164841,
-0.0106628282133226));
#42952=CARTESIAN_POINT('Ctrl Pts',(-0.220141375216936,0.00750242060037397,
-0.0106702777889441));
#42953=CARTESIAN_POINT('Ctrl Pts',(-0.220172641439852,0.00750243204482037,
-0.0106841716126293));
#42954=CARTESIAN_POINT('Ctrl Pts',(-0.220189148542913,0.00750250301964164,
-0.0106840844290246));
#42955=CARTESIAN_POINT('Ctrl Pts',(-0.220191305017738,0.00750239221586241,
-0.0106841477117758));
#42956=CARTESIAN_POINT('Ctrl Pts',(-0.220191748876597,0.00750243783530509,
-0.010684158519063));
#42957=CARTESIAN_POINT('Ctrl Pts',(-0.220393577735485,0.0131409926298503,
-0.00859656506818599));
#42958=CARTESIAN_POINT('Ctrl Pts',(-0.220393600784383,0.0131455013235971,
-0.00860197156800209));
#42959=CARTESIAN_POINT('Ctrl Pts',(-0.220394508723612,0.013150390707749,
-0.00860694383723535));
#42960=CARTESIAN_POINT('Ctrl Pts',(-0.220398273034233,0.0131617074700728,
-0.00861677217987557));
#42961=CARTESIAN_POINT('Ctrl Pts',(-0.22040141745688,0.0131680966885574,
-0.00862129135659766));
#42962=CARTESIAN_POINT('Ctrl Pts',(-0.220411875451266,0.0131850252832542,
-0.00863112133216668));
#42963=CARTESIAN_POINT('Ctrl Pts',(-0.220420838703223,0.0131960597967277,
-0.00863536618801003));
#42964=CARTESIAN_POINT('Ctrl Pts',(-0.220443547262691,0.0132187413918395,
-0.00863979428834782));
#42965=CARTESIAN_POINT('Ctrl Pts',(-0.220456699734264,0.0132295555728947,
-0.00863957428719857));
#42966=CARTESIAN_POINT('Ctrl Pts',(-0.220477028370402,0.0132439117277982,
-0.00863638017660647));
#42967=CARTESIAN_POINT('Ctrl Pts',(-0.220483964499296,0.0132484256939255,
-0.00863482543045935));
#42968=CARTESIAN_POINT('Ctrl Pts',(-0.2204943501556,0.0132546690049436,
-0.00863186022596393));
#42969=CARTESIAN_POINT('Ctrl Pts',(-0.220497771526208,0.0132566431653764,
-0.00863078258852987));
#42970=CARTESIAN_POINT('Ctrl Pts',(-0.220502900998905,0.013259490106136,
-0.00862901351443286));
#42971=CARTESIAN_POINT('Ctrl Pts',(-0.220504589263189,0.013260407142419,
-0.00862840655268303));
#42972=CARTESIAN_POINT('Ctrl Pts',(-0.220507103876826,0.0132617598017022,
-0.00862745672848966));
#42973=CARTESIAN_POINT('Ctrl Pts',(-0.220507997798412,0.01326223654587,
-0.00862711078108925));
#42974=CARTESIAN_POINT('Ctrl Pts',(-0.220509361404001,0.0132629886447625,
-0.00862654885235569));
#42975=CARTESIAN_POINT('Ctrl Pts',(-0.220509756647642,0.0132632201317573,
-0.00862637051561302));
#42976=CARTESIAN_POINT('Ctrl Pts',(-0.22051016964372,0.0132635045056427,
-0.00862614893167951));
#42977=CARTESIAN_POINT('Ctrl Pts',(-0.220510279030594,0.0132635929926122,
-0.00862607912610677));
#42978=CARTESIAN_POINT('Ctrl Pts',(-0.220510520647363,0.0132639284950142,
-0.0086258093258324));
#42979=CARTESIAN_POINT('Ctrl Pts',(-0.219280593258087,0.0129089030369612,
-0.0087540208922909));
#42980=CARTESIAN_POINT('Ctrl Pts',(-0.219279471351069,0.0129697183219162,
-0.00883447223599688));
#42981=CARTESIAN_POINT('Ctrl Pts',(-0.219232227122818,0.01303995698963,
-0.00877963895487713));
#42982=CARTESIAN_POINT('Ctrl Pts',(-0.219480859972423,0.0129956387985517,
-0.00869259253052726));
#42983=CARTESIAN_POINT('Ctrl Pts',(-0.219479765662262,0.0130574432834654,
-0.0087722973921775));
#42984=CARTESIAN_POINT('Ctrl Pts',(-0.219432533921543,0.0131270216872618,
-0.00871660628740151));
#42985=CARTESIAN_POINT('Ctrl Pts',(-0.219777491499906,0.0131256379037001,
-0.00859541257530931));
#42986=CARTESIAN_POINT('Ctrl Pts',(-0.21977673918151,0.0131889796566377,
-0.00867405729017068));
#42987=CARTESIAN_POINT('Ctrl Pts',(-0.219731924878373,0.01326225933775,
-0.0086132441302433));
#42988=CARTESIAN_POINT('Ctrl Pts',(-0.220181220363713,0.0131791518408284,
-0.00855905807384794));
#42989=CARTESIAN_POINT('Ctrl Pts',(-0.220179703043079,0.0132430749198211,
-0.0086374684420407));
#42990=CARTESIAN_POINT('Ctrl Pts',(-0.220187007242741,0.0133222515952173,
-0.00857148014111763));
#42991=CARTESIAN_POINT('Ctrl Pts',(-0.220388732889043,0.0131402149694449,
-0.00859463791750654));
#42992=CARTESIAN_POINT('Ctrl Pts',(-0.220387054388994,0.0132037278064557,
-0.00867326792055314));
#42993=CARTESIAN_POINT('Ctrl Pts',(-0.220408297394784,0.0132801431120848,
-0.00861058770866753));
#42994=CARTESIAN_POINT('Ctrl Pts',(-0.220499526505995,0.013122678869508,
-0.00861080275449944));
#42995=CARTESIAN_POINT('Ctrl Pts',(-0.220497842335634,0.0131860042786699,
-0.0086895830169195));
#42996=CARTESIAN_POINT('Ctrl Pts',(-0.220519081583513,0.0132625694282041,
-0.00862708545017783));
#42997=CARTESIAN_POINT('Ctrl Pts',(-0.219329717540431,0.0129304387340275,
-0.00873922893714474));
#42998=CARTESIAN_POINT('Ctrl Pts',(-0.219329619304978,0.0129346525482004,
-0.0087447320476796));
#42999=CARTESIAN_POINT('Ctrl Pts',(-0.219328881296596,0.0129392175326603,
-0.00874991025846167));
#43000=CARTESIAN_POINT('Ctrl Pts',(-0.219326066620048,0.0129492576252757,
-0.00875981945591603));
#43001=CARTESIAN_POINT('Ctrl Pts',(-0.219323909241627,0.0129547202760547,
-0.00876443358395337));
#43002=CARTESIAN_POINT('Ctrl Pts',(-0.219316118880593,0.0129704063023137,
-0.0087757011237742));
#43003=CARTESIAN_POINT('Ctrl Pts',(-0.219309194587094,0.0129807551150745,
-0.00878091792349644));
#43004=CARTESIAN_POINT('Ctrl Pts',(-0.219292289600658,0.013001250202485,
-0.00878728601601963));
#43005=CARTESIAN_POINT('Ctrl Pts',(-0.21928234369875,0.0130111975838273,
-0.00878821585785464));
#43006=CARTESIAN_POINT('Ctrl Pts',(-0.219260891119607,0.013029288793666,
-0.00878572430074405));
#43007=CARTESIAN_POINT('Ctrl Pts',(-0.219251496806023,0.0130355885641391,
-0.00878249392109267));
#43008=CARTESIAN_POINT('Ctrl Pts',(-0.219243411968739,0.0130407035975206,
-0.00877917947485082));
#43009=CARTESIAN_POINT('Ctrl Pts',(-0.21924126324647,0.0130419515911249,
-0.00877827875086926));
#43010=CARTESIAN_POINT('Ctrl Pts',(-0.219239363903856,0.0130430555261411,
-0.00877739438131471));
#43011=CARTESIAN_POINT('Ctrl Pts',(-0.220150919053116,0.00813012261928148,
-0.0105594969353601));
#43012=CARTESIAN_POINT('Ctrl Pts',(-0.220147560322325,0.00813744816509899,
-0.010662288922204));
#43013=CARTESIAN_POINT('Ctrl Pts',(-0.220250337214706,0.00812906192089311,
-0.0106631669086847));
#43014=CARTESIAN_POINT('Ctrl Pts',(-0.220034517280683,0.00691186126661964,
-0.0106452660313614));
#43015=CARTESIAN_POINT('Ctrl Pts',(-0.220031127462352,0.00690494866270766,
-0.0107490709111982));
#43016=CARTESIAN_POINT('Ctrl Pts',(-0.220133619056969,0.00689398622454344,
-0.0107485661923428));
#43017=CARTESIAN_POINT('Ctrl Pts',(-0.219898176228963,0.00510523286236233,
-0.0104011082367351));
#43018=CARTESIAN_POINT('Ctrl Pts',(-0.219894892210515,0.00507786839668421,
-0.0105021637906976));
#43019=CARTESIAN_POINT('Ctrl Pts',(-0.219998638957578,0.00507695382070288,
-0.0104998409426915));
#43020=CARTESIAN_POINT('Ctrl Pts',(-0.220106792893513,0.0028045235466563,
-0.00933167834600581));
#43021=CARTESIAN_POINT('Ctrl Pts',(-0.220103961877512,0.00275039714016751,
-0.00942029587214831));
#43022=CARTESIAN_POINT('Ctrl Pts',(-0.220205907292707,0.0027661935911115,
-0.00942830878118668));
#43023=CARTESIAN_POINT('Ctrl Pts',(-0.220411551979736,0.00183607302071643,
-0.00860959612604254));
#43024=CARTESIAN_POINT('Ctrl Pts',(-0.220408986658667,0.00177108263111936,
-0.00869003939775851));
#43025=CARTESIAN_POINT('Ctrl Pts',(-0.220509160419223,0.0017906577512894,
-0.00870494804850675));
#43026=CARTESIAN_POINT('Ctrl Pts',(-0.220558570384699,0.00131983115813253,
-0.00812527721236594));
#43027=CARTESIAN_POINT('Ctrl Pts',(-0.220556199753953,0.00124882039973508,
-0.00820005680446187));
#43028=CARTESIAN_POINT('Ctrl Pts',(-0.220657200684646,0.00126452842110998,
-0.00821397254802884));
#43029=CARTESIAN_POINT('Ctrl Pts',(-0.220398945127186,0.00187230965206566,
-0.00860743240415377));
#43030=CARTESIAN_POINT('Ctrl Pts',(-0.220398970043393,0.00186866745817968,
-0.00861178659251786));
#43031=CARTESIAN_POINT('Ctrl Pts',(-0.220399593273686,0.00186470597500052,
-0.00861579151699209));
#43032=CARTESIAN_POINT('Ctrl Pts',(-0.220402930635403,0.00185273261831202,
-0.0086261078828164));
#43033=CARTESIAN_POINT('Ctrl Pts',(-0.220406868913276,0.00184442241414017,
-0.00863127211875914));
#43034=CARTESIAN_POINT('Ctrl Pts',(-0.220418894088141,0.00182454980589882,
-0.00864039997366899));
#43035=CARTESIAN_POINT('Ctrl Pts',(-0.220428439657727,0.00181219952729001,
-0.00864351310290853));
#43036=CARTESIAN_POINT('Ctrl Pts',(-0.220452242219434,0.0017865171103747,
-0.00864509456873525));
#43037=CARTESIAN_POINT('Ctrl Pts',(-0.220465792372549,0.00177414120939264,
-0.00864328267353371));
#43038=CARTESIAN_POINT('Ctrl Pts',(-0.220486501745454,0.00175742793939046,
-0.00863784249252514));
#43039=CARTESIAN_POINT('Ctrl Pts',(-0.220493602587884,0.00175206904922223,
-0.00863552670233257));
#43040=CARTESIAN_POINT('Ctrl Pts',(-0.220504215447333,0.00174455715684026,
-0.00863145439251244));
#43041=CARTESIAN_POINT('Ctrl Pts',(-0.22050771555906,0.00174215999883712,
-0.00863001397738395));
#43042=CARTESIAN_POINT('Ctrl Pts',(-0.220512959035891,0.00173867870828759,
-0.00862770839708991));
#43043=CARTESIAN_POINT('Ctrl Pts',(-0.220514685798646,0.00173755168528413,
-0.00862692540284276));
#43044=CARTESIAN_POINT('Ctrl Pts',(-0.220517267823617,0.00173587973325043,
-0.00862571017892817));
#43045=CARTESIAN_POINT('Ctrl Pts',(-0.220518176036435,0.00173529568430238,
-0.00862527475663612));
#43046=CARTESIAN_POINT('Ctrl Pts',(-0.220519572749422,0.00173437365590044,
-0.00862457224594662));
#43047=CARTESIAN_POINT('Ctrl Pts',(-0.220519976590864,0.00173409409974473,
-0.00862435421538105));
#43048=CARTESIAN_POINT('Ctrl Pts',(-0.220520438475924,0.00173372995230389,
-0.00862406799262633));
#43049=CARTESIAN_POINT('Ctrl Pts',(-0.22052056788612,0.0017336078325201,
-0.0086239708361658));
#43050=CARTESIAN_POINT('Ctrl Pts',(-0.220520758525357,0.00173330231663648,
-0.00862372404872762));
#43051=CARTESIAN_POINT('Ctrl Pts',(-0.219148515071371,0.00691048297255687,
-0.0105396975990103));
#43052=CARTESIAN_POINT('Ctrl Pts',(-0.219147356380851,0.00690322974884955,
-0.0106487703174557));
#43053=CARTESIAN_POINT('Ctrl Pts',(-0.219038955168735,0.00689487685220507,
-0.010637242672756));
#43054=CARTESIAN_POINT('Ctrl Pts',(-0.219036137036226,0.00807747716428064,
-0.0106153242780037));
#43055=CARTESIAN_POINT('Ctrl Pts',(-0.219034955335834,0.00808468304500183,
-0.0107253460856709));
#43056=CARTESIAN_POINT('Ctrl Pts',(-0.218926799334561,0.00807242090324395,
-0.0107151659237768));
#43057=CARTESIAN_POINT('Ctrl Pts',(-0.218905132240887,0.00977915705389375,
-0.0103918892388122));
#43058=CARTESIAN_POINT('Ctrl Pts',(-0.218904029998625,0.00980665680374094,
-0.0104992708126475));
#43059=CARTESIAN_POINT('Ctrl Pts',(-0.218794734263875,0.0098026290016253,
-0.0104909783450489));
#43060=CARTESIAN_POINT('Ctrl Pts',(-0.219071089153358,0.0119671367922082,
-0.00943613238649878));
#43061=CARTESIAN_POINT('Ctrl Pts',(-0.219070437343078,0.0120216325715906,
-0.00953173065297142));
#43062=CARTESIAN_POINT('Ctrl Pts',(-0.218962442721151,0.0120305426252144,
-0.00951571104175434));
#43063=CARTESIAN_POINT('Ctrl Pts',(-0.21932523698136,0.0129089558008521,
-0.00878419964750562));
#43064=CARTESIAN_POINT('Ctrl Pts',(-0.21932487961028,0.0129746248050434,
-0.00887199152970325));
#43065=CARTESIAN_POINT('Ctrl Pts',(-0.219218564468832,0.0129875068392683,
-0.00884975676863126));
#43066=CARTESIAN_POINT('Ctrl Pts',(-0.219454102120046,0.0134244664873124,
-0.00833869489519783));
#43067=CARTESIAN_POINT('Ctrl Pts',(-0.21945392109255,0.0134964707033814,
-0.00842100564533139));
#43068=CARTESIAN_POINT('Ctrl Pts',(-0.219346826781403,0.0135047144980998,
-0.00840040661615055));
#43069=CARTESIAN_POINT('Ctrl Pts',(-0.219093941307367,0.00750191211356895,
-0.0105597759983895));
#43070=CARTESIAN_POINT('Ctrl Pts',(-0.219093767460342,0.00750191339671021,
-0.0105661672114314));
#43071=CARTESIAN_POINT('Ctrl Pts',(-0.219092978750846,0.00750191452875406,
-0.0105725269115254));
#43072=CARTESIAN_POINT('Ctrl Pts',(-0.219090069650718,0.0075019165336753,
-0.0105855632853716));
#43073=CARTESIAN_POINT('Ctrl Pts',(-0.219087845371762,0.00750191736905565,
-0.010592180920131));
#43074=CARTESIAN_POINT('Ctrl Pts',(-0.219079594227124,0.00750191908697261,
-0.0106102290130474));
#43075=CARTESIAN_POINT('Ctrl Pts',(-0.219072020861462,0.00750191940049146,
-0.0106207966092312));
#43076=CARTESIAN_POINT('Ctrl Pts',(-0.219053282710123,0.00750191812597504,
-0.010638488913879));
#43077=CARTESIAN_POINT('Ctrl Pts',(-0.219042291643416,0.0075019166823333,
-0.0106454469725408));
#43078=CARTESIAN_POINT('Ctrl Pts',(-0.21901994966729,0.00750191087528336,
-0.0106541838284163));
#43079=CARTESIAN_POINT('Ctrl Pts',(-0.21900904021347,0.00750192874869014,
-0.0106564768272035));
#43080=CARTESIAN_POINT('Ctrl Pts',(-0.218995822383935,0.00750187995871182,
-0.0106570539596742));
#43081=CARTESIAN_POINT('Ctrl Pts',(-0.218993530792735,0.00750190999230115,
-0.0106570779154422));
#43082=CARTESIAN_POINT('Ctrl Pts',(-0.218991340185995,0.00750190949851256,
-0.0106570284103405));
#43083=CARTESIAN_POINT('Ctrl Pts',(-0.220657718078581,0.0018751479361439,
-0.00861162539660087));
#43084=CARTESIAN_POINT('Ctrl Pts',(-0.220656233896277,0.00181097856082264,
-0.00869193835890256));
#43085=CARTESIAN_POINT('Ctrl Pts',(-0.220658316110286,0.00173232387629273,
-0.00862547314886965));
#43086=CARTESIAN_POINT('Ctrl Pts',(-0.22038644554275,0.00187704155792308,
-0.00860803515775927));
#43087=CARTESIAN_POINT('Ctrl Pts',(-0.220384869594419,0.00181290856447447,
-0.00868834779106167));
#43088=CARTESIAN_POINT('Ctrl Pts',(-0.220387269569338,0.00173488744681977,
-0.0086225160123027));
#43089=CARTESIAN_POINT('Ctrl Pts',(-0.220000575954751,0.00185543408637361,
-0.00858349740986387));
#43090=CARTESIAN_POINT('Ctrl Pts',(-0.219999192384961,0.001791130697238,
-0.00866379310111029));
#43091=CARTESIAN_POINT('Ctrl Pts',(-0.220002878180249,0.00171042904111559,
-0.00859532149219416));
#43092=CARTESIAN_POINT('Ctrl Pts',(-0.219511028165309,0.00195343846120863,
-0.00865283203789838));
#43093=CARTESIAN_POINT('Ctrl Pts',(-0.219510389522585,0.00189013343318333,
-0.00873358372156444));
#43094=CARTESIAN_POINT('Ctrl Pts',(-0.21946299979619,0.00181705681249047,
-0.00867264489778598));
#43095=CARTESIAN_POINT('Ctrl Pts',(-0.21933003719857,0.00208585294127225,
-0.00875179762193781));
#43096=CARTESIAN_POINT('Ctrl Pts',(-0.219329139091007,0.00202413227238718,
-0.0088332651959512));
#43097=CARTESIAN_POINT('Ctrl Pts',(-0.219257176298931,0.00196751447944682,
-0.00878690909359569));
#43098=CARTESIAN_POINT('Ctrl Pts',(-0.219194504687458,0.00217281033445456,
-0.00881277285849614));
#43099=CARTESIAN_POINT('Ctrl Pts',(-0.219193456552492,0.00211219507604886,
-0.00889529739755567));
#43100=CARTESIAN_POINT('Ctrl Pts',(-0.219134455871745,0.0020464823948761,
-0.00884311272090225));
#43101=CARTESIAN_POINT('Ctrl Pts',(-0.219334416590634,0.00208138222259607,
-0.00874824491983627));
#43102=CARTESIAN_POINT('Ctrl Pts',(-0.219334320063737,0.00207729391397082,
-0.00875360873145552));
#43103=CARTESIAN_POINT('Ctrl Pts',(-0.219333604008012,0.0020729254234734,
-0.00875871456669258));
#43104=CARTESIAN_POINT('Ctrl Pts',(-0.219330873127534,0.00206344571171821,
-0.00876859253859587));
#43105=CARTESIAN_POINT('Ctrl Pts',(-0.21932878304817,0.0020583446652351,
-0.00877327424185474));
#43106=CARTESIAN_POINT('Ctrl Pts',(-0.219321082227192,0.00204357506471506,
-0.00878514705354778));
#43107=CARTESIAN_POINT('Ctrl Pts',(-0.219314085814434,0.00203382895482756,
-0.00879102793417479));
#43108=CARTESIAN_POINT('Ctrl Pts',(-0.219296933162624,0.00201489256784713,
-0.00879883654619196));
#43109=CARTESIAN_POINT('Ctrl Pts',(-0.219286886376862,0.00200588731369565,
-0.00880062956795521));
#43110=CARTESIAN_POINT('Ctrl Pts',(-0.219267063004303,0.00199122629751845,
-0.00880003617161851));
#43111=CARTESIAN_POINT('Ctrl Pts',(-0.219257585685345,0.00198532728737071,
-0.00879831194460528));
#43112=CARTESIAN_POINT('Ctrl Pts',(-0.219246107062773,0.00197933492943865,
-0.0087945788756421));
#43113=CARTESIAN_POINT('Ctrl Pts',(-0.219244027871131,0.00197832881338241,
-0.00879386553455533));
#43114=CARTESIAN_POINT('Ctrl Pts',(-0.219242032666924,0.00197738200797957,
-0.00879310436763141));
#43115=CARTESIAN_POINT('Ctrl Pts',(-0.219456692804946,0.00160111516560854,
-0.00836091035860459));
#43116=CARTESIAN_POINT('Ctrl Pts',(-0.219456067988,0.00152938117372744,
-0.00844342455429431));
#43117=CARTESIAN_POINT('Ctrl Pts',(-0.21934905497045,0.00152127094901417,
-0.00842244164486835));
#43118=CARTESIAN_POINT('Ctrl Pts',(-0.219328501201104,0.00210658569623933,
-0.00879635302666999));
#43119=CARTESIAN_POINT('Ctrl Pts',(-0.219327710138628,0.0020410357238593,
-0.00888421377064837));
#43120=CARTESIAN_POINT('Ctrl Pts',(-0.219221528779172,0.00202801777676731,
-0.00886143697198539));
#43121=CARTESIAN_POINT('Ctrl Pts',(-0.219071052564132,0.00305712341290254,
-0.00945029735204128));
#43122=CARTESIAN_POINT('Ctrl Pts',(-0.219069957508154,0.00300287510524064,
-0.00954601666865521));
#43123=CARTESIAN_POINT('Ctrl Pts',(-0.218961981689591,0.00299433920943247,
-0.00952977548234196));
#43124=CARTESIAN_POINT('Ctrl Pts',(-0.21890924160936,0.00523430232329638,
-0.0103936309275109));
#43125=CARTESIAN_POINT('Ctrl Pts',(-0.218907695683505,0.00520698605406793,
-0.0105010210078774));
#43126=CARTESIAN_POINT('Ctrl Pts',(-0.218798486649354,0.00521092820910359,
-0.0104921956534221));
#43127=CARTESIAN_POINT('Ctrl Pts',(-0.219035732064863,0.00692495059794331,
-0.0106157551916045));
#43128=CARTESIAN_POINT('Ctrl Pts',(-0.219034112291182,0.0069178206797144,
-0.0107257579164001));
#43129=CARTESIAN_POINT('Ctrl Pts',(-0.218926003176411,0.00693008662460253,
-0.0107151679806557));
#43130=CARTESIAN_POINT('Ctrl Pts',(-0.21914839349402,0.00809331137238897,
-0.0105399211052043));
#43131=CARTESIAN_POINT('Ctrl Pts',(-0.219146795855022,0.00810064627671322,
-0.0106489679471506));
#43132=CARTESIAN_POINT('Ctrl Pts',(-0.219038451062826,0.00810890497429706,
-0.0106370139428235));
#43133=CARTESIAN_POINT('Ctrl Pts',(-0.218366734177772,0.0131720326746961,
-0.00853098609508188));
#43134=CARTESIAN_POINT('Ctrl Pts',(-0.218364368788007,0.0132365740471837,
-0.0086106656298705));
#43135=CARTESIAN_POINT('Ctrl Pts',(-0.218465622250289,0.0132237145107785,
-0.00862087933247721));
#43136=CARTESIAN_POINT('Ctrl Pts',(-0.218264676471441,0.0126816728273647,
-0.00892565173193766));
#43137=CARTESIAN_POINT('Ctrl Pts',(-0.218262150148847,0.0127406029499428,
-0.00900985123627725));
#43138=CARTESIAN_POINT('Ctrl Pts',(-0.218362864026326,0.0127246548055583,
-0.00902087117030197));
#43139=CARTESIAN_POINT('Ctrl Pts',(-0.218046218879305,0.011755491836367,
-0.00952662103886202));
#43140=CARTESIAN_POINT('Ctrl Pts',(-0.218043459768016,0.0118040969683048,
-0.00961757890671437));
#43141=CARTESIAN_POINT('Ctrl Pts',(-0.218145341696559,0.0117918242380693,
-0.00962344777185459));
#43142=CARTESIAN_POINT('Ctrl Pts',(-0.21791304015827,0.00964780445850701,
-0.0103903848894813));
#43143=CARTESIAN_POINT('Ctrl Pts',(-0.217909924561879,0.00967207053712899,
-0.0104913089502273));
#43144=CARTESIAN_POINT('Ctrl Pts',(-0.218012908881215,0.00967428276848505,
-0.0104896633779764));
#43145=CARTESIAN_POINT('Ctrl Pts',(-0.218040716494051,0.00803350871449782,
-0.0105873246231014));
#43146=CARTESIAN_POINT('Ctrl Pts',(-0.218037511620459,0.00803976883496589,
-0.0106904112618394));
#43147=CARTESIAN_POINT('Ctrl Pts',(-0.218139463091569,0.00805065232707797,
-0.0106903621342042));
#43148=CARTESIAN_POINT('Ctrl Pts',(-0.218146767290287,0.00693520855091888,
-0.0105189682128489));
#43149=CARTESIAN_POINT('Ctrl Pts',(-0.218143588420993,0.00692870570122577,
-0.0106212622622081));
#43150=CARTESIAN_POINT('Ctrl Pts',(-0.218245775367947,0.00693731273779504,
-0.010622470145281));
#43151=CARTESIAN_POINT('Ctrl Pts',(-0.218192328823198,0.00750145352954351,
-0.0106389704498565));
#43152=CARTESIAN_POINT('Ctrl Pts',(-0.2181543005054,0.00750020162177904,
-0.0106381076224975));
#43153=CARTESIAN_POINT('Ctrl Pts',(-0.218121876716844,0.00749892202213666,
-0.0106133962756449));
#43154=CARTESIAN_POINT('Ctrl Pts',(-0.218107640280115,0.00749903957930803,
-0.0105885851589611));
#43155=CARTESIAN_POINT('Ctrl Pts',(-0.218097198595685,0.00749912580136693,
-0.0105703874978662));
#43156=CARTESIAN_POINT('Ctrl Pts',(-0.218094029014762,0.00749974391570192,
-0.0105524213574574));
#43157=CARTESIAN_POINT('Ctrl Pts',(-0.218094302309927,0.00750066584756617,
-0.0105367248189618));
#43158=CARTESIAN_POINT('Ctrl Pts',(-0.218256492401995,0.012654359922174,
-0.00892058569152569));
#43159=CARTESIAN_POINT('Ctrl Pts',(-0.218256481075259,0.0126585238231222,
-0.00892637097765501));
#43160=CARTESIAN_POINT('Ctrl Pts',(-0.218257350196721,0.0126631391930071,
-0.00893172184708259));
#43161=CARTESIAN_POINT('Ctrl Pts',(-0.218261001203897,0.0126739431288319,
-0.00894229936358914));
#43162=CARTESIAN_POINT('Ctrl Pts',(-0.218264045113842,0.0126801169194239,
-0.00894718999230209));
#43163=CARTESIAN_POINT('Ctrl Pts',(-0.218274189130881,0.0126966972458564,
-0.00895796495222554));
#43164=CARTESIAN_POINT('Ctrl Pts',(-0.21828289381032,0.0127077179240462,
-0.00896277666495482));
#43165=CARTESIAN_POINT('Ctrl Pts',(-0.218303764735828,0.0127295276295352,
-0.00896800026065576));
#43166=CARTESIAN_POINT('Ctrl Pts',(-0.218315084933949,0.0127396308911177,
-0.00896847361115103));
#43167=CARTESIAN_POINT('Ctrl Pts',(-0.218338385874436,0.0127579969737962,
-0.00896614627596395));
#43168=CARTESIAN_POINT('Ctrl Pts',(-0.218350528380616,0.0127663971078985,
-0.0089633590109566));
#43169=CARTESIAN_POINT('Ctrl Pts',(-0.218365200384923,0.0127753616348796,
-0.00895831830330567));
#43170=CARTESIAN_POINT('Ctrl Pts',(-0.2183677753286,0.0127768749342853,
-0.00895738426770429));
#43171=CARTESIAN_POINT('Ctrl Pts',(-0.21837031549238,0.0127783363881555,
-0.00895639440167604));
#43172=CARTESIAN_POINT('Ctrl Pts',(-0.217040091656276,0.012403843259427,
-0.00906292069881238));
#43173=CARTESIAN_POINT('Ctrl Pts',(-0.217038761654309,0.0124598798457787,
-0.00914919008978224));
#43174=CARTESIAN_POINT('Ctrl Pts',(-0.216999104629513,0.012537682949266,
-0.00909454615819164));
#43175=CARTESIAN_POINT('Ctrl Pts',(-0.217281733864375,0.0124892414562469,
-0.00901276450047278));
#43176=CARTESIAN_POINT('Ctrl Pts',(-0.217280397845029,0.0125462736073253,
-0.00909836481671279));
#43177=CARTESIAN_POINT('Ctrl Pts',(-0.217239846774433,0.0126225707764438,
-0.00904344449318198));
#43178=CARTESIAN_POINT('Ctrl Pts',(-0.217615520035054,0.0126222176898706,
-0.0089287395813754));
#43179=CARTESIAN_POINT('Ctrl Pts',(-0.217614512072917,0.0126808196249854,
-0.00901335824389992));
#43180=CARTESIAN_POINT('Ctrl Pts',(-0.21757524696877,0.0127590442565254,
-0.00895505101893103));
#43181=CARTESIAN_POINT('Ctrl Pts',(-0.218095966824174,0.012688547985487,
-0.00889135063154049));
#43182=CARTESIAN_POINT('Ctrl Pts',(-0.218094341784189,0.0127478797061336,
-0.00897567723691454));
#43183=CARTESIAN_POINT('Ctrl Pts',(-0.218097022661123,0.0128322256816752,
-0.00891246103404046));
#43184=CARTESIAN_POINT('Ctrl Pts',(-0.218326482347675,0.0126415268496617,
-0.0089289208830992));
#43185=CARTESIAN_POINT('Ctrl Pts',(-0.218324514240548,0.0127003721197212,
-0.00901344065888466));
#43186=CARTESIAN_POINT('Ctrl Pts',(-0.218351703750586,0.0127806085914963,
-0.00895449084106678));
#43187=CARTESIAN_POINT('Ctrl Pts',(-0.218486740291147,0.0126204219818312,
-0.00894655101177062));
#43188=CARTESIAN_POINT('Ctrl Pts',(-0.21848498462662,0.0126790186976341,
-0.00903130724294094));
#43189=CARTESIAN_POINT('Ctrl Pts',(-0.218499591342393,0.0127613749089422,
-0.00897089160770076));
#43190=CARTESIAN_POINT('Ctrl Pts',(-0.217213461658688,0.0124664448294026,
-0.0090260632281852));
#43191=CARTESIAN_POINT('Ctrl Pts',(-0.21721334964017,0.0124703852687589,
-0.00903197163158273));
#43192=CARTESIAN_POINT('Ctrl Pts',(-0.217212551997362,0.0124747370879997,
-0.00903753852187564));
#43193=CARTESIAN_POINT('Ctrl Pts',(-0.217209524833361,0.0124844786784638,
-0.0090482314753298));
#43194=CARTESIAN_POINT('Ctrl Pts',(-0.217207205691832,0.0124898587949991,
-0.00905321498766304));
#43195=CARTESIAN_POINT('Ctrl Pts',(-0.217198995661428,0.0125052463498904,
-0.00906521834175148));
#43196=CARTESIAN_POINT('Ctrl Pts',(-0.217191850065853,0.0125154539764049,
-0.00907075651121354));
#43197=CARTESIAN_POINT('Ctrl Pts',(-0.217174446413349,0.0125361395163697,
-0.00907780358828333));
#43198=CARTESIAN_POINT('Ctrl Pts',(-0.217164146319917,0.01254643804596,
-0.00907897566944418));
#43199=CARTESIAN_POINT('Ctrl Pts',(-0.217144783322987,0.0125631339420775,
-0.0090770720803645));
#43200=CARTESIAN_POINT('Ctrl Pts',(-0.217135986280563,0.0125698791697788,
-0.00907488480431806));
#43201=CARTESIAN_POINT('Ctrl Pts',(-0.217125162398161,0.0125771752050296,
-0.00907073982030332));
#43202=CARTESIAN_POINT('Ctrl Pts',(-0.217123134210988,0.0125785287737803,
-0.00906988376298916));
#43203=CARTESIAN_POINT('Ctrl Pts',(-0.217121145625652,0.0125797949708599,
-0.00906899621093816));
#43204=CARTESIAN_POINT('Origin',(-0.221715499787086,0.00708341181933542,
-0.00318613591211986));
#43205=CARTESIAN_POINT('Ctrl Pts',(-0.218253133205786,0.00235141097830992,
-0.0089245544184659));
#43206=CARTESIAN_POINT('Ctrl Pts',(-0.218253410928626,0.00234810267626737,
-0.00892913201349592));
#43207=CARTESIAN_POINT('Ctrl Pts',(-0.218254239150138,0.00234445216715201,
-0.00893336289573748));
#43208=CARTESIAN_POINT('Ctrl Pts',(-0.218257213663284,0.00233570235473179,
-0.00894198142806612));
#43209=CARTESIAN_POINT('Ctrl Pts',(-0.218259582821079,0.00233056670380563,
-0.00894608123347948));
#43210=CARTESIAN_POINT('Ctrl Pts',(-0.218268103529493,0.00231517587711936,
-0.00895624950748682));
#43211=CARTESIAN_POINT('Ctrl Pts',(-0.218276029056875,0.0023039815039752,
-0.00896105351889245));
#43212=CARTESIAN_POINT('Ctrl Pts',(-0.218298885248443,0.00227709004331209,
-0.00896741642455435));
#43213=CARTESIAN_POINT('Ctrl Pts',(-0.218313668431264,0.00226278335865085,
-0.00896712995333946));
#43214=CARTESIAN_POINT('Ctrl Pts',(-0.218339073783571,0.00224206387255127,
-0.00896359231248858));
#43215=CARTESIAN_POINT('Ctrl Pts',(-0.218349354969513,0.00223499767086404,
-0.00896112793673578));
#43216=CARTESIAN_POINT('Ctrl Pts',(-0.218361577669561,0.00222939301302785,
-0.00895902039524703));
#43217=CARTESIAN_POINT('Ctrl Pts',(-0.218364773986022,0.00222841493280178,
-0.00895862510642795));
#43218=CARTESIAN_POINT('Ctrl Pts',(-0.218368303205535,0.00222784554213887,
-0.008958425171701));
#43219=CARTESIAN_POINT('Ctrl Pts',(-0.218368983786652,0.00222776219852354,
-0.00895839830988281));
#43220=CARTESIAN_POINT('Ctrl Pts',(-0.218370051622135,0.00222767735278557,
-0.00895837687448052));
#43221=CARTESIAN_POINT('Ctrl Pts',(-0.218370435101234,0.00222765604199265,
-0.0089583733051086));
#43222=CARTESIAN_POINT('Ctrl Pts',(-0.218370898995356,0.00222764180170897,
-0.00895837421103516));
#43223=CARTESIAN_POINT('Ctrl Pts',(-0.218370978719185,0.00222763976512466,
-0.00895837455258704));
#43224=CARTESIAN_POINT('Ctrl Pts',(-0.218371097454342,0.00222763734785523,
-0.00895837534004206));
#43225=CARTESIAN_POINT('Ctrl Pts',(-0.218371136455611,0.00222763665277974,
-0.00895837564347949));
#43226=CARTESIAN_POINT('Ctrl Pts',(-0.218371194729898,0.00222763576250506,
-0.00895837616398511));
#43227=CARTESIAN_POINT('Ctrl Pts',(-0.21837121400151,0.00222763549231493,
-0.00895837634708607));
#43228=CARTESIAN_POINT('Ctrl Pts',(-0.21837157020395,0.00222763094680333,
-0.00895837993439936));
#43229=CARTESIAN_POINT('Ctrl Pts',(-0.218371906861464,0.00222763406685814,
-0.00895838668294486));
#43230=CARTESIAN_POINT('Ctrl Pts',(-0.21837272401761,0.00222766001051709,
-0.00895841136466877));
#43231=CARTESIAN_POINT('Ctrl Pts',(-0.218373202789348,0.00222769062793541,
-0.00895843279476503));
#43232=CARTESIAN_POINT('Ctrl Pts',(-0.218374162278603,0.00222778845837024,
-0.00895849206198491));
#43233=CARTESIAN_POINT('Ctrl Pts',(-0.217137975046077,0.00696793545844773,
-0.010498682606056));
#43234=CARTESIAN_POINT('Ctrl Pts',(-0.217136098788072,0.00696139686822146,
-0.0106072154889929));
#43235=CARTESIAN_POINT('Ctrl Pts',(-0.217028226897065,0.00695342027943268,
-0.0105957515286141));
#43236=CARTESIAN_POINT('Ctrl Pts',(-0.217053838228916,0.00803642449059388,
-0.0105608338666006));
#43237=CARTESIAN_POINT('Ctrl Pts',(-0.217051942792171,0.00804295377515252,
-0.0106701621405877));
#43238=CARTESIAN_POINT('Ctrl Pts',(-0.216944315818264,0.00803207665662111,
-0.0106595760977952));
#43239=CARTESIAN_POINT('Ctrl Pts',(-0.216834062029484,0.0101942506675489,
-0.0102951033665484));
#43240=CARTESIAN_POINT('Ctrl Pts',(-0.216832278499687,0.0102265108470005,
-0.0104012659729614));
#43241=CARTESIAN_POINT('Ctrl Pts',(-0.216723046287982,0.0102229255069439,
-0.0103943346079308));
#43242=CARTESIAN_POINT('Ctrl Pts',(-0.217139620528726,0.0121082417373667,
-0.00931994380391762));
#43243=CARTESIAN_POINT('Ctrl Pts',(-0.217138290003539,0.0121639970902703,
-0.00941421194997972));
#43244=CARTESIAN_POINT('Ctrl Pts',(-0.217031554121602,0.0121751503709153,
-0.00939571084227512));
#43245=CARTESIAN_POINT('Ctrl Pts',(-0.217302514187605,0.0129451438661898,
-0.00868850801833797));
#43246=CARTESIAN_POINT('Ctrl Pts',(-0.21730144433856,0.0130107637348759,
-0.0087752130077434));
#43247=CARTESIAN_POINT('Ctrl Pts',(-0.217194260965553,0.0130166427226768,
-0.00875779847180095));
#43248=CARTESIAN_POINT('Ctrl Pts',(-0.217094602028452,0.00750113053183012,
-0.0105144286534109));
#43249=CARTESIAN_POINT('Ctrl Pts',(-0.217094437212978,0.00750113150038833,
-0.0105208711260764));
#43250=CARTESIAN_POINT('Ctrl Pts',(-0.217093647894512,0.0075011323107023,
-0.0105272823912877));
#43251=CARTESIAN_POINT('Ctrl Pts',(-0.217090730637772,0.00750113367523198,
-0.0105403653760066));
#43252=CARTESIAN_POINT('Ctrl Pts',(-0.217088509145498,0.00750113419953919,
-0.0105469802676839));
#43253=CARTESIAN_POINT('Ctrl Pts',(-0.217080266267631,0.00750113521677092,
-0.0105650259084567));
#43254=CARTESIAN_POINT('Ctrl Pts',(-0.217072698383241,0.00750113526272342,
-0.0105755947798971));
#43255=CARTESIAN_POINT('Ctrl Pts',(-0.217053971209092,0.00750113485315194,
-0.0105932906477769));
#43256=CARTESIAN_POINT('Ctrl Pts',(-0.217042985779792,0.0075011340222172,
-0.0106002512537286));
#43257=CARTESIAN_POINT('Ctrl Pts',(-0.217017963698496,0.00750113668349459,
-0.0106100456301875));
#43258=CARTESIAN_POINT('Ctrl Pts',(-0.217006490540518,0.00750110816344995,
-0.0106114329679777));
#43259=CARTESIAN_POINT('Ctrl Pts',(-0.216997738159605,0.00750119231094314,
-0.0106118147301237));
#43260=CARTESIAN_POINT('Ctrl Pts',(-0.216995365374494,0.00750115899475884,
-0.0106118866829067));
#43261=CARTESIAN_POINT('Ctrl Pts',(-0.216992999839987,0.00750111626434787,
-0.0106118648816169));
#43262=CARTESIAN_POINT('Ctrl Pts',(-0.216992039095986,0.00750111592075218,
-0.0106118432044358));
#43263=CARTESIAN_POINT('Ctrl Pts',(-0.218512610680756,0.00234799200238128,
-0.00892513212683489));
#43264=CARTESIAN_POINT('Ctrl Pts',(-0.218510961166635,0.00228569700038617,
-0.00901443661716485));
#43265=CARTESIAN_POINT('Ctrl Pts',(-0.218510479461922,0.00220162766540384,
-0.00894450423745255));
#43266=CARTESIAN_POINT('Ctrl Pts',(-0.218253521679468,0.00235591056916128,
-0.00892562091397768));
#43267=CARTESIAN_POINT('Ctrl Pts',(-0.218251625806045,0.00229376201742538,
-0.00901496892835533));
#43268=CARTESIAN_POINT('Ctrl Pts',(-0.218250013232297,0.0022113668624948,
-0.00894636662237075));
#43269=CARTESIAN_POINT('Ctrl Pts',(-0.217710461308748,0.00233840441957516,
-0.00890257715584968));
#43270=CARTESIAN_POINT('Ctrl Pts',(-0.217709301310539,0.00227593220586861,
-0.00899202305588306));
#43271=CARTESIAN_POINT('Ctrl Pts',(-0.217717598087536,0.00218340813805773,
-0.00891627557236298));
#43272=CARTESIAN_POINT('Ctrl Pts',(-0.217289578618135,0.00247969338690751,
-0.008992986854597));
#43273=CARTESIAN_POINT('Ctrl Pts',(-0.217288486176955,0.00241901651396548,
-0.00908277776569406));
#43274=CARTESIAN_POINT('Ctrl Pts',(-0.217215756044667,0.00235437055333393,
-0.00902768579769387));
#43275=CARTESIAN_POINT('Ctrl Pts',(-0.217070832594413,0.00262754346735014,
-0.00908405008417822));
#43276=CARTESIAN_POINT('Ctrl Pts',(-0.21706937681227,0.00256874785681079,
-0.00917523660469239));
#43277=CARTESIAN_POINT('Ctrl Pts',(-0.217012813213666,0.00249727254229426,
-0.00911768489661139));
#43278=CARTESIAN_POINT('Ctrl Pts',(-0.217217202596967,0.0025390925417853,
-0.00902979181142551));
#43279=CARTESIAN_POINT('Ctrl Pts',(-0.217217093433627,0.00253527919148381,
-0.00903552446223438));
#43280=CARTESIAN_POINT('Ctrl Pts',(-0.217216329286209,0.00253113398466886,
-0.00904098318928687));
#43281=CARTESIAN_POINT('Ctrl Pts',(-0.217213429525352,0.0025219928280744,
-0.00905156722422215));
#43282=CARTESIAN_POINT('Ctrl Pts',(-0.217211212022842,0.00251700491423114,
-0.009056582169978));
#43283=CARTESIAN_POINT('Ctrl Pts',(-0.217203165994395,0.00250257048297124,
-0.00906915389328079));
#43284=CARTESIAN_POINT('Ctrl Pts',(-0.217195977250999,0.00249296457500099,
-0.0090753340588464));
#43285=CARTESIAN_POINT('Ctrl Pts',(-0.21717841474632,0.00247391188454135,
-0.00908372182048253));
#43286=CARTESIAN_POINT('Ctrl Pts',(-0.217168087826125,0.00246464189341527,
-0.0090857168567731));
#43287=CARTESIAN_POINT('Ctrl Pts',(-0.217148131929838,0.00244954809164539,
-0.00908536881790682));
#43288=CARTESIAN_POINT('Ctrl Pts',(-0.217138815370543,0.0024434373481414,
-0.00908379239471274));
#43289=CARTESIAN_POINT('Ctrl Pts',(-0.217127386079639,0.00243704830970052,
-0.00908029240560058));
#43290=CARTESIAN_POINT('Ctrl Pts',(-0.21712532989568,0.00243592263217277,
-0.00907959027446985));
#43291=CARTESIAN_POINT('Ctrl Pts',(-0.217123295418768,0.00243486422508496,
-0.00907884373636323));
#43292=CARTESIAN_POINT('Ctrl Pts',(-0.217305590590327,0.00206475955975603,
-0.00869612615818939));
#43293=CARTESIAN_POINT('Ctrl Pts',(-0.217304725296217,0.00199931848412992,
-0.00878289128905937));
#43294=CARTESIAN_POINT('Ctrl Pts',(-0.217197584750829,0.00199323238160935,
-0.00876569203822327));
#43295=CARTESIAN_POINT('Ctrl Pts',(-0.217140314114961,0.00291363579254913,
-0.00933321669145991));
#43296=CARTESIAN_POINT('Ctrl Pts',(-0.217139184840844,0.002858204433682,
-0.00942760897514758));
#43297=CARTESIAN_POINT('Ctrl Pts',(-0.217032492189526,0.00284685187725704,
-0.00940936648213871));
#43298=CARTESIAN_POINT('Ctrl Pts',(-0.216837373073137,0.00481822843586069,
-0.010296613574004));
#43299=CARTESIAN_POINT('Ctrl Pts',(-0.216835800873413,0.00478613513583303,
-0.0104027295262049));
#43300=CARTESIAN_POINT('Ctrl Pts',(-0.216726609134844,0.00478956143554811,
-0.0103960267216009));
#43301=CARTESIAN_POINT('Ctrl Pts',(-0.217054377111761,0.00697128504474957,
-0.0105604810661386));
#43302=CARTESIAN_POINT('Ctrl Pts',(-0.217052690956768,0.00696483378685744,
-0.0106697439278292));
#43303=CARTESIAN_POINT('Ctrl Pts',(-0.216945096195469,0.00697563227639263,
-0.0106594296379724));
#43304=CARTESIAN_POINT('Ctrl Pts',(-0.217137406949296,0.00802996460581778,
-0.0104984600401621));
#43305=CARTESIAN_POINT('Ctrl Pts',(-0.217135740417579,0.00803645694558565,
-0.0106069320876849));
#43306=CARTESIAN_POINT('Ctrl Pts',(-0.21702790179751,0.00804439497834719,
-0.0105957520847982));
#43307=CARTESIAN_POINT('Ctrl Pts',(-0.216282845990138,0.0128929856408761,
-0.00870791588407719));
#43308=CARTESIAN_POINT('Ctrl Pts',(-0.21628054597117,0.0129542040883401,
-0.00879035739816422));
#43309=CARTESIAN_POINT('Ctrl Pts',(-0.216382357754694,0.0129431688471136,
-0.00879814483003904));
#43310=CARTESIAN_POINT('Ctrl Pts',(-0.216133718571471,0.012057373323281,
-0.00932799336983377));
#43311=CARTESIAN_POINT('Ctrl Pts',(-0.216131165247688,0.0121092546354352,
-0.00941743508173665));
#43312=CARTESIAN_POINT('Ctrl Pts',(-0.216232605411869,0.0120943919614193,
-0.00942553527241766));
#43313=CARTESIAN_POINT('Ctrl Pts',(-0.215835443717348,0.0101441471812373,
-0.0102857637590424));
#43314=CARTESIAN_POINT('Ctrl Pts',(-0.215832522774285,0.0101740039538028,
-0.0103861540384211));
#43315=CARTESIAN_POINT('Ctrl Pts',(-0.215936094441128,0.0101739288277866,
-0.0103832444006597));
#43316=CARTESIAN_POINT('Ctrl Pts',(-0.216055651587784,0.00800709561225113,
-0.0105372628493557));
#43317=CARTESIAN_POINT('Ctrl Pts',(-0.216052594542648,0.00801302128485416,
-0.0106404734829225));
#43318=CARTESIAN_POINT('Ctrl Pts',(-0.216154763548897,0.00802309106962762,
-0.0106402736064033));
#43319=CARTESIAN_POINT('Ctrl Pts',(-0.216139422648866,0.00696389597780172,
-0.0104755961789519));
#43320=CARTESIAN_POINT('Ctrl Pts',(-0.216136391047069,0.00695775334100502,
-0.0105780830921685));
#43321=CARTESIAN_POINT('Ctrl Pts',(-0.216238791290835,0.00696598534872043,
-0.0105788762726166));
#43322=CARTESIAN_POINT('Ctrl Pts',(-0.216094904650184,0.00750081531065442,
-0.0104915380007917));
#43323=CARTESIAN_POINT('Ctrl Pts',(-0.216094756795897,0.00750081620795364,
-0.0104980811404747));
#43324=CARTESIAN_POINT('Ctrl Pts',(-0.216095253916839,0.00750081722356874,
-0.0105046226317289));
#43325=CARTESIAN_POINT('Ctrl Pts',(-0.216097595249637,0.00750081955421988,
-0.0105179231430352));
#43326=CARTESIAN_POINT('Ctrl Pts',(-0.21609951640324,0.00750082087733701,
-0.0105246324342848));
#43327=CARTESIAN_POINT('Ctrl Pts',(-0.216106938011482,0.00750082498061469,
-0.0105430328719986));
#43328=CARTESIAN_POINT('Ctrl Pts',(-0.216114022367117,0.00750082798353315,
-0.0105539325807752));
#43329=CARTESIAN_POINT('Ctrl Pts',(-0.216131934369291,0.00750083480936225,
-0.0105724556140836));
#43330=CARTESIAN_POINT('Ctrl Pts',(-0.21614259590609,0.00750083832245985,
-0.0105799047757781));
#43331=CARTESIAN_POINT('Ctrl Pts',(-0.216167838768553,0.00750084939658654,
-0.0105911228479625));
#43332=CARTESIAN_POINT('Ctrl Pts',(-0.216179521428449,0.00750084106413271,
-0.0105928076172997));
#43333=CARTESIAN_POINT('Ctrl Pts',(-0.2161873624299,0.00750089292605126,
-0.0105935055836128));
#43334=CARTESIAN_POINT('Ctrl Pts',(-0.21618964357311,0.00750087208550254,
-0.0105936739646218));
#43335=CARTESIAN_POINT('Ctrl Pts',(-0.216191922147214,0.00750084456948937,
-0.0105937600086224));
#43336=CARTESIAN_POINT('Ctrl Pts',(-0.216192970650498,0.00750084471341908,
-0.0105937837104633));
#43337=CARTESIAN_POINT('Ctrl Pts',(-0.216191694510709,0.012362961460189,
-0.0090741750090641));
#43338=CARTESIAN_POINT('Ctrl Pts',(-0.216191822194119,0.0123768807643042,
-0.00909512604910344));
#43339=CARTESIAN_POINT('Ctrl Pts',(-0.216210230367078,0.012406465199571,
-0.00911336004700776));
#43340=CARTESIAN_POINT('Ctrl Pts',(-0.216228375424446,0.0124310958868995,
-0.0091172997600751));
#43341=CARTESIAN_POINT('Ctrl Pts',(-0.216230005813432,0.0124333090296043,
-0.00911765375536227));
#43342=CARTESIAN_POINT('Ctrl Pts',(-0.216231634734948,0.0124354692167458,
-0.00911792635430594));
#43343=CARTESIAN_POINT('Ctrl Pts',(-0.216233248932233,0.0124375588927111,
-0.00911812893263417));
#43344=CARTESIAN_POINT('Ctrl Pts',(-0.216251094709426,0.0124606613300867,
-0.00912036853974034));
#43345=CARTESIAN_POINT('Ctrl Pts',(-0.21626716337826,0.0124750802192241,
-0.00911813030457629));
#43346=CARTESIAN_POINT('Ctrl Pts',(-0.216295540195969,0.01249768233462,
-0.00910640980901082));
#43347=CARTESIAN_POINT('Ctrl Pts',(-0.216298702098623,0.0125002007878656,
-0.00910510384629096));
#43348=CARTESIAN_POINT('Ctrl Pts',(-0.216302017321607,0.0125028010528426,
-0.00910363126631569));
#43349=CARTESIAN_POINT('Ctrl Pts',(-0.216305506198624,0.0125054790081327,
-0.00910194677041158));
#43350=CARTESIAN_POINT('Origin',(-0.216343159043645,0.0124520636670066,
-0.00901812198471994));
#43351=CARTESIAN_POINT('Ctrl Pts',(-0.215095414441432,0.0124591460413101,
-0.00910819331956975));
#43352=CARTESIAN_POINT('Ctrl Pts',(-0.215120401030406,0.0124359848540545,
-0.00912362130480649));
#43353=CARTESIAN_POINT('Ctrl Pts',(-0.215133772132029,0.0124182892002308,
-0.00912603088362709));
#43354=CARTESIAN_POINT('Ctrl Pts',(-0.215148702658334,0.0123986783815203,
-0.00912385037729619));
#43355=CARTESIAN_POINT('Ctrl Pts',(-0.215150299639797,0.0123965807921044,
-0.0091236171485326));
#43356=CARTESIAN_POINT('Ctrl Pts',(-0.215151915486707,0.0123944349474128,
-0.00912329023287928));
#43357=CARTESIAN_POINT('Ctrl Pts',(-0.215153554980737,0.0123922157146173,
-0.00912285148268702));
#43358=CARTESIAN_POINT('Ctrl Pts',(-0.215170522460296,0.0123692483927538,
-0.00911831076172079));
#43359=CARTESIAN_POINT('Ctrl Pts',(-0.215184387550774,0.0123381808782917,
-0.00909998527609093));
#43360=CARTESIAN_POINT('Ctrl Pts',(-0.215184823658102,0.0123239090545933,
-0.00907757182940712));
#43361=CARTESIAN_POINT('Ctrl Pts',(-0.216139285036328,0.00803827977272542,
-0.0104749865165695));
#43362=CARTESIAN_POINT('Ctrl Pts',(-0.216135584338956,0.00804453914118892,
-0.0105781229455219));
#43363=CARTESIAN_POINT('Ctrl Pts',(-0.216238660816216,0.00803629527470715,
-0.0105788969339609));
#43364=CARTESIAN_POINT('Ctrl Pts',(-0.216055763094736,0.00699299166987041,
-0.0105363034745261));
#43365=CARTESIAN_POINT('Ctrl Pts',(-0.21605203840423,0.00698709339425489,
-0.0106401704688209));
#43366=CARTESIAN_POINT('Ctrl Pts',(-0.216154883042114,0.00697697631507577,
-0.0106399414472133));
#43367=CARTESIAN_POINT('Ctrl Pts',(-0.215836736738016,0.00486495828754412,
-0.0102881783975672));
#43368=CARTESIAN_POINT('Ctrl Pts',(-0.215833138858722,0.00483500982269961,
-0.010389261864091));
#43369=CARTESIAN_POINT('Ctrl Pts',(-0.215937390039039,0.00483525154752722,
-0.0103863545090138));
#43370=CARTESIAN_POINT('Ctrl Pts',(-0.216137707812793,0.00294240207909308,
-0.00932702833761163));
#43371=CARTESIAN_POINT('Ctrl Pts',(-0.216134494712672,0.00289008833417827,
-0.00941698370469411));
#43372=CARTESIAN_POINT('Ctrl Pts',(-0.216236595839286,0.00290507470426125,
-0.00942512670023606));
#43373=CARTESIAN_POINT('Ctrl Pts',(-0.216285909883727,0.00211376764744365,
-0.00871193737699649));
#43374=CARTESIAN_POINT('Ctrl Pts',(-0.216282947197694,0.00205216060863476,
-0.00879490657085487));
#43375=CARTESIAN_POINT('Ctrl Pts',(-0.216385423407197,0.00206332475774103,
-0.00880273997904361));
#43376=CARTESIAN_POINT('Ctrl Pts',(-0.216308829828652,0.00249826452155856,
-0.00910474619664736));
#43377=CARTESIAN_POINT('Ctrl Pts',(-0.216277540774277,0.00252224331941416,
-0.00911980910851503));
#43378=CARTESIAN_POINT('Ctrl Pts',(-0.216259966794798,0.00253762812048443,
-0.00912198916335422));
#43379=CARTESIAN_POINT('Ctrl Pts',(-0.216242133257728,0.00255926286473761,
-0.00912127524977043));
#43380=CARTESIAN_POINT('Ctrl Pts',(-0.216240281249037,0.00256150962791337,
-0.00912120111001024));
#43381=CARTESIAN_POINT('Ctrl Pts',(-0.216238426704362,0.00256383525815522,
-0.00912105340666394));
#43382=CARTESIAN_POINT('Ctrl Pts',(-0.216236553900389,0.00256625758763653,
-0.00912081190907445));
#43383=CARTESIAN_POINT('Ctrl Pts',(-0.216218499535794,0.00258960953490383,
-0.00911848380341484));
#43384=CARTESIAN_POINT('Ctrl Pts',(-0.216198685889085,0.00262068047583808,
-0.00910311875075495));
#43385=CARTESIAN_POINT('Ctrl Pts',(-0.216195457832998,0.00263678928674248,
-0.00908219213157078));
#43386=CARTESIAN_POINT('Ctrl Pts',(-0.216195172748967,0.00263821192768416,
-0.00908034400849087));
#43387=CARTESIAN_POINT('Ctrl Pts',(-0.216195017839807,0.00263953714974432,
-0.00907848253511195));
#43388=CARTESIAN_POINT('Ctrl Pts',(-0.216195006323166,0.00264076383020346,
-0.00907662663635085));
#43389=CARTESIAN_POINT('Ctrl Pts',(-0.215138268707419,0.00698344596248103,
-0.0104545905660588));
#43390=CARTESIAN_POINT('Ctrl Pts',(-0.215136339427148,0.00697718956481417,
-0.0105617541112084));
#43391=CARTESIAN_POINT('Ctrl Pts',(-0.21502973621825,0.0069690563131557,
-0.0105517156694489));
#43392=CARTESIAN_POINT('Ctrl Pts',(-0.215054198986798,0.00802081780291805,
-0.0105125259768653));
#43393=CARTESIAN_POINT('Ctrl Pts',(-0.215052252505421,0.00802704965957652,
-0.0106204194577288));
#43394=CARTESIAN_POINT('Ctrl Pts',(-0.214945873650048,0.00801615691193827,
-0.010611304630013));
#43395=CARTESIAN_POINT('Ctrl Pts',(-0.214841832736404,0.0101088263597614,
-0.0102648137814259));
#43396=CARTESIAN_POINT('Ctrl Pts',(-0.214839986037366,0.0101395482971445,
-0.0103698202132453));
#43397=CARTESIAN_POINT('Ctrl Pts',(-0.214732131678294,0.0101366736980693,
-0.0103638814523754));
#43398=CARTESIAN_POINT('Ctrl Pts',(-0.215123122693411,0.0119899129679057,
-0.00934455275222973));
#43399=CARTESIAN_POINT('Ctrl Pts',(-0.215121700939607,0.0120433858470247,
-0.00943849044895999));
#43400=CARTESIAN_POINT('Ctrl Pts',(-0.215015985777715,0.0120539646858002,
-0.00942223756738649));
#43401=CARTESIAN_POINT('Ctrl Pts',(-0.215268700133232,0.0128245611985155,
-0.00873920920956725));
#43402=CARTESIAN_POINT('Ctrl Pts',(-0.215267527785315,0.0128877157588611,
-0.00882601519127026));
#43403=CARTESIAN_POINT('Ctrl Pts',(-0.215161434357862,0.0128936434211584,
-0.00881066198364404));
#43404=CARTESIAN_POINT('Ctrl Pts',(-0.21509521040637,0.00750052117343929,
-0.0104691577567921));
#43405=CARTESIAN_POINT('Ctrl Pts',(-0.215095050257003,0.00750052168721324,
-0.0104756287762937));
#43406=CARTESIAN_POINT('Ctrl Pts',(-0.215094259973477,0.00750052209497991,
-0.0104820686809155));
#43407=CARTESIAN_POINT('Ctrl Pts',(-0.215091335823137,0.00750052273780868,
-0.0104951798602485));
#43408=CARTESIAN_POINT('Ctrl Pts',(-0.215089113650354,0.00750052295534443,
-0.0105017952878704));
#43409=CARTESIAN_POINT('Ctrl Pts',(-0.215080868589627,0.00750052329951441,
-0.0105198415751402));
#43410=CARTESIAN_POINT('Ctrl Pts',(-0.21507329908319,0.00750052316019882,
-0.0105304102155527));
#43411=CARTESIAN_POINT('Ctrl Pts',(-0.215054568613045,0.00750052282350388,
-0.0105481053155121));
#43412=CARTESIAN_POINT('Ctrl Pts',(-0.215043581478387,0.00750052228908468,
-0.0105550653082537));
#43413=CARTESIAN_POINT('Ctrl Pts',(-0.2150187109435,0.00750052547626067,
-0.0105647979495009));
#43414=CARTESIAN_POINT('Ctrl Pts',(-0.215007311554113,0.00750049889594075,
-0.0105662330298729));
#43415=CARTESIAN_POINT('Ctrl Pts',(-0.214998322630719,0.00750057650214591,
-0.010566627439243));
#43416=CARTESIAN_POINT('Ctrl Pts',(-0.214995979516134,0.00750054677270074,
-0.0105666968728011));
#43417=CARTESIAN_POINT('Ctrl Pts',(-0.214993635413369,0.00750050836006935,
-0.010566677172531));
#43418=CARTESIAN_POINT('Ctrl Pts',(-0.21499263918831,0.00750050820908203,
-0.0105666547606325));
#43419=CARTESIAN_POINT('Origin',(-0.215029774015556,0.00259990999948959,
-0.00902581867692437));
#43420=CARTESIAN_POINT('Ctrl Pts',(-0.215187397287789,0.00267846401374506,
-0.0090791176475646));
#43421=CARTESIAN_POINT('Ctrl Pts',(-0.21518696968744,0.00266415867860654,
-0.00910150656180909));
#43422=CARTESIAN_POINT('Ctrl Pts',(-0.215173125231804,0.00263299596606228,
-0.00911976224472072));
#43423=CARTESIAN_POINT('Ctrl Pts',(-0.215156200020307,0.00261007761913271,
-0.00912431726791484));
#43424=CARTESIAN_POINT('Ctrl Pts',(-0.215141017916609,0.00258951960603424,
-0.00912840317458063));
#43425=CARTESIAN_POINT('Ctrl Pts',(-0.215129066319246,0.00257341534231338,
-0.00912637292740067));
#43426=CARTESIAN_POINT('Ctrl Pts',(-0.215106261349755,0.00255100317834008,
-0.0091144188949001));
#43427=CARTESIAN_POINT('Ctrl Pts',(-0.215103643035173,0.00254842996306945,
-0.00911304641257252));
#43428=CARTESIAN_POINT('Ctrl Pts',(-0.21510089371507,0.0025458066359998,
-0.00911149443871825));
#43429=CARTESIAN_POINT('Ctrl Pts',(-0.21509802079524,0.00254314437078809,
-0.00910972203361875));
#43430=CARTESIAN_POINT('Ctrl Pts',(-0.215271626585773,0.00217581993097967,
-0.0087395861630685));
#43431=CARTESIAN_POINT('Ctrl Pts',(-0.215270612896943,0.00211272999214843,
-0.00882634758645658));
#43432=CARTESIAN_POINT('Ctrl Pts',(-0.215164580280835,0.00210664128134,
-0.00881118174408626));
#43433=CARTESIAN_POINT('Ctrl Pts',(-0.215125355803509,0.00301599520621347,
-0.00934778240909707));
#43434=CARTESIAN_POINT('Ctrl Pts',(-0.215124091178223,0.00296265152479492,
-0.00944170503104277));
#43435=CARTESIAN_POINT('Ctrl Pts',(-0.215018435808979,0.00295196260828074,
-0.00942567372829455));
#43436=CARTESIAN_POINT('Ctrl Pts',(-0.214843449546337,0.00488752405156655,
-0.0102630167362636));
#43437=CARTESIAN_POINT('Ctrl Pts',(-0.214841765608511,0.00485677866707993,
-0.0103679243946987));
#43438=CARTESIAN_POINT('Ctrl Pts',(-0.214733971784369,0.00485940615041609,
-0.0103621640961027));
#43439=CARTESIAN_POINT('Ctrl Pts',(-0.215054296090415,0.00698177131318153,
-0.0105127506298666));
#43440=CARTESIAN_POINT('Ctrl Pts',(-0.215052509277578,0.00697555952124977,
-0.0106205720293646));
#43441=CARTESIAN_POINT('Ctrl Pts',(-0.214946183406747,0.00698642042182544,
-0.0106117051843749));
#43442=CARTESIAN_POINT('Ctrl Pts',(-0.215138102089214,0.008016862224145,
-0.0104542932258017));
#43443=CARTESIAN_POINT('Ctrl Pts',(-0.215136333069552,0.00802310475840938,
-0.0105613805147221));
#43444=CARTESIAN_POINT('Ctrl Pts',(-0.21502978407555,0.00803120569858454,
-0.0105515845758995));
#43445=CARTESIAN_POINT('Ctrl Pts',(-0.1924290089395,0.0029155191620011,
-0.0087649001815275));
#43446=CARTESIAN_POINT('Ctrl Pts',(-0.192427813903335,0.00286412403846673,
-0.00885788426072911));
#43447=CARTESIAN_POINT('Ctrl Pts',(-0.192388140977693,0.00278108903612549,
-0.00880417838622631));
#43448=CARTESIAN_POINT('Ctrl Pts',(-0.192151357383384,0.00302045420861078,
-0.00881768715629337));
#43449=CARTESIAN_POINT('Ctrl Pts',(-0.192149891191152,0.00297037731033976,
-0.0089113558197304));
#43450=CARTESIAN_POINT('Ctrl Pts',(-0.192109318357643,0.0028883972306172,
-0.0088594852174804));
#43451=CARTESIAN_POINT('Ctrl Pts',(-0.191564370518527,0.00320957432995767,
-0.0089069598377226));
#43452=CARTESIAN_POINT('Ctrl Pts',(-0.19156378155172,0.00316120722641246,
-0.0090017598976799));
#43453=CARTESIAN_POINT('Ctrl Pts',(-0.191530402374114,0.00306724379457668,
-0.00894702953336356));
#43454=CARTESIAN_POINT('Ctrl Pts',(-0.191125263038703,0.0035084303185505,
-0.00904496669604534));
#43455=CARTESIAN_POINT('Ctrl Pts',(-0.191124237464691,0.00346354789673269,
-0.00914061051655912));
#43456=CARTESIAN_POINT('Ctrl Pts',(-0.191035800399296,0.00341041835692548,
-0.00910842868632399));
#43457=CARTESIAN_POINT('Ctrl Pts',(-0.190937017957496,0.0037465261723087,
-0.0091449485015039));
#43458=CARTESIAN_POINT('Ctrl Pts',(-0.190935691282421,0.00370453581711239,
-0.00924202969982603));
#43459=CARTESIAN_POINT('Ctrl Pts',(-0.190858333402855,0.00364208478676822,
-0.00920738829771903));
#43460=CARTESIAN_POINT('Ctrl Pts',(-0.190965502145366,0.00353026999546062,
-0.00915929064154693));
#43461=CARTESIAN_POINT('Ctrl Pts',(-0.190965605451063,0.00353079645007945,
-0.00915951112912086));
#43462=CARTESIAN_POINT('Ctrl Pts',(-0.190965733635172,0.00353130737617717,
-0.00915972129380536));
#43463=CARTESIAN_POINT('Ctrl Pts',(-0.190966490909549,0.00353376944855981,
-0.00916071300828134));
#43464=CARTESIAN_POINT('Ctrl Pts',(-0.190967482378507,0.00353551921344156,
-0.00916135128342715));
#43465=CARTESIAN_POINT('Ctrl Pts',(-0.190971146089304,0.0035400391972326,
-0.00916272934769088));
#43466=CARTESIAN_POINT('Ctrl Pts',(-0.190974269748778,0.00354238079049634,
-0.00916309172510267));
#43467=CARTESIAN_POINT('Ctrl Pts',(-0.19098337409412,0.00354882134562363,
-0.00916350304047491));
#43468=CARTESIAN_POINT('Ctrl Pts',(-0.190992994450311,0.00355431796352706,
-0.00916254541256994));
#43469=CARTESIAN_POINT('Ctrl Pts',(-0.191014214843227,0.00356811463625413,
-0.00915492575966953));
#43470=CARTESIAN_POINT('Ctrl Pts',(-0.191023999687439,0.00357530482732608,
-0.00914874127804869));
#43471=CARTESIAN_POINT('Ctrl Pts',(-0.191038764613866,0.00358848101622443,
-0.00913369118535732));
#43472=CARTESIAN_POINT('Ctrl Pts',(-0.191044168965102,0.00359437633404391,
-0.00912547730853556));
#43473=CARTESIAN_POINT('Ctrl Pts',(-0.191051371066627,0.00360489423478907,
-0.00910776989774631));
#43474=CARTESIAN_POINT('Ctrl Pts',(-0.191053379384272,0.00360949977795018,
-0.00909857985643356));
#43475=CARTESIAN_POINT('Ctrl Pts',(-0.191053878207127,0.00361347960381807,
-0.00908895687335754));
#43476=CARTESIAN_POINT('Ctrl Pts',(-0.192132462182123,0.00302309075119266,
-0.00882016247897886));
#43477=CARTESIAN_POINT('Ctrl Pts',(-0.192132442819634,0.00302125537502577,
-0.00882340434178846));
#43478=CARTESIAN_POINT('Ctrl Pts',(-0.192132668003466,0.0030191530391176,
-0.00882646181140498));
#43479=CARTESIAN_POINT('Ctrl Pts',(-0.192133661041556,0.0030140373109328,
-0.00883271844226365));
#43480=CARTESIAN_POINT('Ctrl Pts',(-0.192134510220713,0.00301097864583467,
-0.00883578008871502));
#43481=CARTESIAN_POINT('Ctrl Pts',(-0.192138197164547,0.0030000437412503,
-0.00884498967153028));
#43482=CARTESIAN_POINT('Ctrl Pts',(-0.192142128390703,0.00299134690026601,
-0.00884964983556151));
#43483=CARTESIAN_POINT('Ctrl Pts',(-0.192154479741903,0.00296719877950705,
-0.00885874451096875));
#43484=CARTESIAN_POINT('Ctrl Pts',(-0.1921653336808,0.00294909544095686,
-0.00886129523940827));
#43485=CARTESIAN_POINT('Ctrl Pts',(-0.192196429509983,0.00290264262977971,
-0.00885915219647058));
#43486=CARTESIAN_POINT('Ctrl Pts',(-0.192217925314133,0.00287403243266648,
-0.00885152302894445));
#43487=CARTESIAN_POINT('Ctrl Pts',(-0.1922431894099,0.00284378191811412,
-0.00883670835956577));
#43488=CARTESIAN_POINT('Ctrl Pts',(-0.192245761353967,0.00284072455684682,
-0.00883512844000508));
#43489=CARTESIAN_POINT('Ctrl Pts',(-0.192248330636423,0.00283771782980501,
-0.00883349208308415));
#43490=CARTESIAN_POINT('Ctrl Pts',(-0.192146295419618,0.007998500997684,
-0.00993609477708802));
#43491=CARTESIAN_POINT('Ctrl Pts',(-0.192143163680161,0.00800393442705837,
-0.0100379107780708));
#43492=CARTESIAN_POINT('Ctrl Pts',(-0.192244833050654,0.00799565242682731,
-0.0100394822591525));
#43493=CARTESIAN_POINT('Ctrl Pts',(-0.192066759891807,0.00703646350569687,
-0.00998607675950129));
#43494=CARTESIAN_POINT('Ctrl Pts',(-0.192063607017836,0.00703133130810636,
-0.0100884494227043));
#43495=CARTESIAN_POINT('Ctrl Pts',(-0.192165083030494,0.0070212017559552,
-0.0100890993436359));
#43496=CARTESIAN_POINT('Ctrl Pts',(-0.191868670782975,0.00507862867971864,
-0.00978403360874624));
#43497=CARTESIAN_POINT('Ctrl Pts',(-0.191865622779181,0.00505262673975468,
-0.00988428333480491));
#43498=CARTESIAN_POINT('Ctrl Pts',(-0.191968270900675,0.00505204884076484,
-0.00988281487389815));
#43499=CARTESIAN_POINT('Ctrl Pts',(-0.19209757540129,0.00327314217054443,
-0.00900318967073468));
#43500=CARTESIAN_POINT('Ctrl Pts',(-0.19209486680983,0.00322733400399338,
-0.00909490321918779));
#43501=CARTESIAN_POINT('Ctrl Pts',(-0.192196050463947,0.00323906751335872,
-0.00910136943874098));
#43502=CARTESIAN_POINT('Ctrl Pts',(-0.192205000280064,0.0024605199261876,
-0.00849014764764348));
#43503=CARTESIAN_POINT('Ctrl Pts',(-0.192202514426249,0.00240604705426371,
-0.00857635021631835));
#43504=CARTESIAN_POINT('Ctrl Pts',(-0.192303953731296,0.00241478292287016,
-0.00858251379116096));
#43505=CARTESIAN_POINT('Ctrl Pts',(-0.192104402373237,0.00750389176243192,
-0.00994933158139058));
#43506=CARTESIAN_POINT('Ctrl Pts',(-0.192103979165972,0.00750527449581046,
-0.00997324593122452));
#43507=CARTESIAN_POINT('Ctrl Pts',(-0.192111890405995,0.00750588809089745,
-0.0100049234964412));
#43508=CARTESIAN_POINT('Ctrl Pts',(-0.192141219896257,0.0075050875176516,
-0.0100289357476997));
#43509=CARTESIAN_POINT('Ctrl Pts',(-0.192157040747162,0.00750465567414363,
-0.0100418883849151));
#43510=CARTESIAN_POINT('Ctrl Pts',(-0.192179303563212,0.00750379772760193,
-0.0100510538033473));
#43511=CARTESIAN_POINT('Ctrl Pts',(-0.192202406927022,0.00750306323134365,
-0.0100515763887981));
#43512=CARTESIAN_POINT('Origin',(-0.194542786613652,0.00713436881430736,
-0.00197293957666947));
#43513=CARTESIAN_POINT('Ctrl Pts',(-0.191102282748796,0.00750206962804297,
-0.00992689565167905));
#43514=CARTESIAN_POINT('Ctrl Pts',(-0.19110084689697,0.00750224800180091,
-0.00995579396725443));
#43515=CARTESIAN_POINT('Ctrl Pts',(-0.191084835201888,0.00750291681681606,
-0.00999379021915688));
#43516=CARTESIAN_POINT('Ctrl Pts',(-0.191046197864609,0.00750287758542002,
-0.01001378202915));
#43517=CARTESIAN_POINT('Ctrl Pts',(-0.191033355225391,0.00750286454532199,
-0.0100204270937726));
#43518=CARTESIAN_POINT('Ctrl Pts',(-0.191018294913059,0.00750280309028856,
-0.0100247834669135));
#43519=CARTESIAN_POINT('Ctrl Pts',(-0.191002128651513,0.0075027969382303,
-0.0100254082193667));
#43520=CARTESIAN_POINT('Origin',(-0.195908379925447,0.00793866795006121,
-0.00229708592964099));
#43521=CARTESIAN_POINT('Ctrl Pts',(-0.192244563328644,0.012158535091762,
-0.00883493377276686));
#43522=CARTESIAN_POINT('Ctrl Pts',(-0.192244179096753,0.012158413276973,
-0.00883499662067414));
#43523=CARTESIAN_POINT('Ctrl Pts',(-0.192244009117953,0.0121583548679729,
-0.00883502642875641));
#43524=CARTESIAN_POINT('Ctrl Pts',(-0.192243835442115,0.0121582916006088,
-0.00883505847795769));
#43525=CARTESIAN_POINT('Ctrl Pts',(-0.192243830465275,0.0121582897845668,
-0.00883505939771415));
#43526=CARTESIAN_POINT('Ctrl Pts',(-0.192243820502454,0.0121582861430353,
-0.00883506124162917));
#43527=CARTESIAN_POINT('Ctrl Pts',(-0.192243815516433,0.0121582843175171,
-0.00883506216580142));
#43528=CARTESIAN_POINT('Ctrl Pts',(-0.192243719827578,0.0121582492244368,
-0.00883507992807604));
#43529=CARTESIAN_POINT('Ctrl Pts',(-0.192243629519956,0.0121582150908203,
-0.00883509714156986));
#43530=CARTESIAN_POINT('Ctrl Pts',(-0.192243318166538,0.0121580940099678,
-0.00883515799640806));
#43531=CARTESIAN_POINT('Ctrl Pts',(-0.192243099165596,0.0121580028658637,
-0.00883520345347272));
#43532=CARTESIAN_POINT('Ctrl Pts',(-0.192242404343482,0.0121576961340143,
-0.00883535544509771));
#43533=CARTESIAN_POINT('Ctrl Pts',(-0.192241937163062,0.0121574629129843,
-0.00883546958366822));
#43534=CARTESIAN_POINT('Ctrl Pts',(-0.192232139839439,0.0121521069651809,
-0.00883806590403842));
#43535=CARTESIAN_POINT('Ctrl Pts',(-0.192217601244657,0.0121348786044592,
-0.00884610483975265));
#43536=CARTESIAN_POINT('Ctrl Pts',(-0.192183260265204,0.0120914561509524,
-0.00885704352957424));
#43537=CARTESIAN_POINT('Ctrl Pts',(-0.192167589750093,0.0120694134393657,
-0.00885892799173005));
#43538=CARTESIAN_POINT('Ctrl Pts',(-0.192144836873875,0.0120336815526016,
-0.00885476525831273));
#43539=CARTESIAN_POINT('Ctrl Pts',(-0.192136970607259,0.0120197474923018,
-0.00885049237666547));
#43540=CARTESIAN_POINT('Ctrl Pts',(-0.192128650361237,0.0120021571809274,
-0.00884064170141953));
#43541=CARTESIAN_POINT('Ctrl Pts',(-0.192126285923881,0.0119964577393178,
-0.00883653504531708));
#43542=CARTESIAN_POINT('Ctrl Pts',(-0.192123366403244,0.0119873004964977,
-0.00882746897412633));
#43543=CARTESIAN_POINT('Ctrl Pts',(-0.1921225745397,0.0119837180093985,
-0.00882293875239021));
#43544=CARTESIAN_POINT('Ctrl Pts',(-0.192122375507901,0.0119807553525039,
-0.00881789966923123));
#43545=CARTESIAN_POINT('Origin',(-0.194558258525404,0.00786744520569803,
-0.00198084692036992));
#43546=CARTESIAN_POINT('Ctrl Pts',(-0.191053647336185,0.011398350991669,
-0.00908383078920412));
#43547=CARTESIAN_POINT('Ctrl Pts',(-0.191051239176385,0.0114090168040769,
-0.00912362545786433));
#43548=CARTESIAN_POINT('Ctrl Pts',(-0.191015561786232,0.0114450835541685,
-0.00917073228352145));
#43549=CARTESIAN_POINT('Ctrl Pts',(-0.190954180653395,0.0114759554932708,
-0.00915737097626284));
#43550=CARTESIAN_POINT('Ctrl Pts',(-0.1909336611347,0.0112622521590659,
-0.00914107486762373));
#43551=CARTESIAN_POINT('Ctrl Pts',(-0.190932330870403,0.0113043272600339,
-0.00923806989977741));
#43552=CARTESIAN_POINT('Ctrl Pts',(-0.19085519609301,0.0113669344340182,
-0.00920333160470119));
#43553=CARTESIAN_POINT('Ctrl Pts',(-0.191122119826402,0.0114988266428744,
-0.00904149146625021));
#43554=CARTESIAN_POINT('Ctrl Pts',(-0.191121088423278,0.0115437728913739,
-0.00913705611144188));
#43555=CARTESIAN_POINT('Ctrl Pts',(-0.191032928044611,0.0115971369215591,
-0.0091047534093575));
#43556=CARTESIAN_POINT('Ctrl Pts',(-0.191561405133145,0.0117972153315813,
-0.00890344882356972));
#43557=CARTESIAN_POINT('Ctrl Pts',(-0.191560810155806,0.0118456413151578,
-0.00899816312114753));
#43558=CARTESIAN_POINT('Ctrl Pts',(-0.191527443414654,0.011939457961494,
-0.00894345319026215));
#43559=CARTESIAN_POINT('Ctrl Pts',(-0.192148825589603,0.0119861110815885,
-0.00881409348298998));
#43560=CARTESIAN_POINT('Ctrl Pts',(-0.192147358846835,0.0120362465102458,
-0.00890767634883105));
#43561=CARTESIAN_POINT('Ctrl Pts',(-0.192106861687747,0.0121182030755903,
-0.00885578258088416));
#43562=CARTESIAN_POINT('Ctrl Pts',(-0.192426465779805,0.0120908510696967,
-0.00876130870259275));
#43563=CARTESIAN_POINT('Ctrl Pts',(-0.192425268473339,0.0121423011087959,
-0.00885420723634552));
#43564=CARTESIAN_POINT('Ctrl Pts',(-0.192385661689457,0.0122252927060059,
-0.00880048787717269));
#43565=CARTESIAN_POINT('Ctrl Pts',(-0.203143265159837,0.00801633370630912,
0.0101836825777989));
#43566=CARTESIAN_POINT('Ctrl Pts',(-0.203141479769113,0.00802239493892441,
0.0102900229538855));
#43567=CARTESIAN_POINT('Ctrl Pts',(-0.203035639253689,0.00803068137178952,
0.0102810066415951));
#43568=CARTESIAN_POINT('Ctrl Pts',(-0.203057840262184,0.00699344469555275,
0.0102395505548407));
#43569=CARTESIAN_POINT('Ctrl Pts',(-0.203056037604557,0.00698755444036989,
0.0103465767165832));
#43570=CARTESIAN_POINT('Ctrl Pts',(-0.202950424815462,0.00699862012239534,
0.0103385142775995));
#43571=CARTESIAN_POINT('Ctrl Pts',(-0.202848073423076,0.00493786641202183,
0.010005192713933));
#43572=CARTESIAN_POINT('Ctrl Pts',(-0.20284636887628,0.00490851213721418,
0.0101095556223153));
#43573=CARTESIAN_POINT('Ctrl Pts',(-0.202739295599067,0.00491062963068159,
0.0101043323211961));
#43574=CARTESIAN_POINT('Ctrl Pts',(-0.20312347492238,0.00307357464602607,
0.00913154713288676));
#43575=CARTESIAN_POINT('Ctrl Pts',(-0.203122182207117,0.00302234432021556,
0.00922571364394402));
#43576=CARTESIAN_POINT('Ctrl Pts',(-0.203017150689644,0.00301157267859386,
0.00921085094367838));
#43577=CARTESIAN_POINT('Ctrl Pts',(-0.203261837521653,0.00223709682645751,
0.00855350483889566));
#43578=CARTESIAN_POINT('Ctrl Pts',(-0.203260791220819,0.00217640800752592,
0.00864104067122755));
#43579=CARTESIAN_POINT('Ctrl Pts',(-0.203155400916974,0.00216992139680255,
0.00862693547917218));
#43580=CARTESIAN_POINT('Ctrl Pts',(-0.203091794492762,0.00260433584368978,
0.00891063288456858));
#43581=CARTESIAN_POINT('Ctrl Pts',(-0.203092578852937,0.0026051042160043,
0.00891112148092724));
#43582=CARTESIAN_POINT('Ctrl Pts',(-0.203094718463783,0.00260715346510506,
0.00891239001105441));
#43583=CARTESIAN_POINT('Ctrl Pts',(-0.203096849812164,0.00260926123651513,
0.00891357333550009));
#43584=CARTESIAN_POINT('Ctrl Pts',(-0.203103814059988,0.00261647262656566,
0.00891752136660277));
#43585=CARTESIAN_POINT('Ctrl Pts',(-0.203113335016935,0.00262651213720627,
0.00892216941256439));
#43586=CARTESIAN_POINT('Ctrl Pts',(-0.2031331443551,0.00265049040226918,
0.00892670658809943));
#43587=CARTESIAN_POINT('Ctrl Pts',(-0.203141708444645,0.00266179522616666,
0.0089270465013639));
#43588=CARTESIAN_POINT('Ctrl Pts',(-0.203158061311166,0.00268588448919631,
0.00892337370530938));
#43589=CARTESIAN_POINT('Ctrl Pts',(-0.203165168467178,0.00269794277366491,
0.00891903258144683));
#43590=CARTESIAN_POINT('Ctrl Pts',(-0.20317380042585,0.00271569204477004,
0.00890841480613177));
#43591=CARTESIAN_POINT('Ctrl Pts',(-0.203176481264999,0.00272221842788613,
0.00890337129535317));
#43592=CARTESIAN_POINT('Ctrl Pts',(-0.203179953610341,0.00273350931465458,
0.00889196533745507));
#43593=CARTESIAN_POINT('Ctrl Pts',(-0.203180871974325,0.00273826982050736,
0.00888590166379555));
#43594=CARTESIAN_POINT('Ctrl Pts',(-0.203180998697126,0.00274230934947549,
0.00887926197739174));
#43595=CARTESIAN_POINT('Ctrl Pts',(-0.203100639709157,0.00753037906826921,
0.0102107450661697));
#43596=CARTESIAN_POINT('Ctrl Pts',(-0.203099090135222,0.00752951923346159,
0.0102203116781152));
#43597=CARTESIAN_POINT('Ctrl Pts',(-0.203096168617054,0.00752883521908611,
0.0102296213721084));
#43598=CARTESIAN_POINT('Ctrl Pts',(-0.203086495197114,0.00752764953261652,
0.0102497511281073));
#43599=CARTESIAN_POINT('Ctrl Pts',(-0.203078942608029,0.00752723754370073,
0.0102600067102118));
#43600=CARTESIAN_POINT('Ctrl Pts',(-0.203060470790915,0.00752760843690622,
0.0102772538922881));
#43601=CARTESIAN_POINT('Ctrl Pts',(-0.203050718764228,0.00752840964011891,
0.0102830934125772));
#43602=CARTESIAN_POINT('Ctrl Pts',(-0.203036937214749,0.00753175678717982,
0.0102893280833497));
#43603=CARTESIAN_POINT('Ctrl Pts',(-0.203031505707383,0.00753367407208893,
0.0102911984979226));
#43604=CARTESIAN_POINT('Ctrl Pts',(-0.203026668027738,0.00753693501435748,
0.0102924850185916));
#43605=CARTESIAN_POINT('Origin',(-0.206700215990262,0.00793489080233831,
0.00270768538981742));
#43606=CARTESIAN_POINT('Ctrl Pts',(-0.203173149129105,0.0122530883762422,
0.00888129643155584));
#43607=CARTESIAN_POINT('Ctrl Pts',(-0.20317297440395,0.0122560948442299,
0.00888629945558956));
#43608=CARTESIAN_POINT('Ctrl Pts',(-0.203172378826803,0.0122595322427759,
0.00889101768852518));
#43609=CARTESIAN_POINT('Ctrl Pts',(-0.203169545170064,0.0122702686487425,
0.00890330463092521));
#43610=CARTESIAN_POINT('Ctrl Pts',(-0.203166444115766,0.0122781780964424,
0.00890980912223253));
#43611=CARTESIAN_POINT('Ctrl Pts',(-0.203157426591178,0.0122970194599052,
0.00892114765645108));
#43612=CARTESIAN_POINT('Ctrl Pts',(-0.203151137454044,0.012308013466242,
0.00892515690985519));
#43613=CARTESIAN_POINT('Ctrl Pts',(-0.203133565785846,0.0123357834919288,
0.00893042776982717));
#43614=CARTESIAN_POINT('Ctrl Pts',(-0.203122403731747,0.0123508441733906,
0.0089287818815233));
#43615=CARTESIAN_POINT('Ctrl Pts',(-0.203109264237317,0.0123696428494649,
0.00892395720889688));
#43616=CARTESIAN_POINT('Ctrl Pts',(-0.20310482039667,0.012376293311655,
0.00892138071276046));
#43617=CARTESIAN_POINT('Ctrl Pts',(-0.203101792285941,0.0123844394819698,
0.00891742855940335));
#43618=CARTESIAN_POINT('Ctrl Pts',(-0.203101356726026,0.0123866121346325,
0.00891626326363771));
#43619=CARTESIAN_POINT('Ctrl Pts',(-0.203101333135073,0.0123892896384871,
0.00891472662097877));
#43620=CARTESIAN_POINT('Ctrl Pts',(-0.203101370574358,0.0123899340365954,
0.00891434790493989));
#43621=CARTESIAN_POINT('Ctrl Pts',(-0.20310145223708,0.0123905738715769,
0.00891396305599815));
#43622=CARTESIAN_POINT('Origin',(-0.20434441778413,0.00265832731369415,
0.00885114693566833));
#43623=CARTESIAN_POINT('Ctrl Pts',(-0.204181316283697,0.00274294303023111,
0.00890078282268103));
#43624=CARTESIAN_POINT('Ctrl Pts',(-0.204181287056828,0.00273881907435617,
0.00890738725852497));
#43625=CARTESIAN_POINT('Ctrl Pts',(-0.204182292259389,0.00273400615712081,
0.00891340235304115));
#43626=CARTESIAN_POINT('Ctrl Pts',(-0.204186507159662,0.00272228467311434,
0.00892516085818481));
#43627=CARTESIAN_POINT('Ctrl Pts',(-0.204190032653031,0.00271535424362842,
0.00893042203587288));
#43628=CARTESIAN_POINT('Ctrl Pts',(-0.204201200298807,0.00269705888163771,
0.00894125171668725));
#43629=CARTESIAN_POINT('Ctrl Pts',(-0.204210471656198,0.00268472038578496,
0.00894569431453476));
#43630=CARTESIAN_POINT('Ctrl Pts',(-0.204231987787325,0.00266013135857193,
0.0089495490570302));
#43631=CARTESIAN_POINT('Ctrl Pts',(-0.204243288857956,0.00264868401162524,
0.00894923152111447));
#43632=CARTESIAN_POINT('Ctrl Pts',(-0.204271708133428,0.00262245426542647,
0.00894440471167718));
#43633=CARTESIAN_POINT('Ctrl Pts',(-0.2042855456873,0.00261180096071676,
0.00893858233952874));
#43634=CARTESIAN_POINT('Ctrl Pts',(-0.204290481497631,0.00260829237482262,
0.00893668044444359));
#43635=CARTESIAN_POINT('Ctrl Pts',(-0.204291369900567,0.00260750940639311,
0.00893623488881915));
#43636=CARTESIAN_POINT('Ctrl Pts',(-0.204292561846107,0.00260646367638606,
0.00893563174137504));
#43637=CARTESIAN_POINT('Ctrl Pts',(-0.20429351437778,0.00260574920645494,
0.00893520949065184));
#43638=CARTESIAN_POINT('Origin',(-0.203018603003138,0.0123389583705484,
0.00882666246850923));
#43639=CARTESIAN_POINT('Ctrl Pts',(-0.204179891859367,0.0122530438601656,
0.00890316754771291));
#43640=CARTESIAN_POINT('Ctrl Pts',(-0.204179863704633,0.0122570464468669,
0.00890958321584623));
#43641=CARTESIAN_POINT('Ctrl Pts',(-0.204180810870288,0.0122617012456198,
0.0089154459307373));
#43642=CARTESIAN_POINT('Ctrl Pts',(-0.204184790811729,0.0122730144205793,
0.00892694531711205));
#43643=CARTESIAN_POINT('Ctrl Pts',(-0.204188120976517,0.0122796964340686,
0.00893213201592682));
#43644=CARTESIAN_POINT('Ctrl Pts',(-0.204198812236045,0.012297539383815,
0.00894301985940397));
#43645=CARTESIAN_POINT('Ctrl Pts',(-0.204207792790586,0.0123096697165854,
0.00894760162878872));
#43646=CARTESIAN_POINT('Ctrl Pts',(-0.20422856390432,0.0123337324139222,
0.00895181197930262));
#43647=CARTESIAN_POINT('Ctrl Pts',(-0.204239392292698,0.0123448692438461,
0.00895175758388408));
#43648=CARTESIAN_POINT('Ctrl Pts',(-0.204264059719803,0.0123680501513342,
0.0089481455679986));
#43649=CARTESIAN_POINT('Ctrl Pts',(-0.204276250240103,0.0123780056183922,
0.00894405172270597));
#43650=CARTESIAN_POINT('Ctrl Pts',(-0.2042855365112,0.0123853730064948,
0.00894033700997319));
#43651=CARTESIAN_POINT('Ctrl Pts',(-0.204288263139933,0.0123874525706704,
0.00893926256526248));
#43652=CARTESIAN_POINT('Ctrl Pts',(-0.204290996832348,0.0123894716281726,
0.00893810788811969));
#43653=CARTESIAN_POINT('Ctrl Pts',(-0.204292042411585,0.0123902568575966,
0.00893764437443986));
#43654=CARTESIAN_POINT('Ctrl Pts',(-0.204265062019709,0.00221964372301113,
0.00856007836605492));
#43655=CARTESIAN_POINT('Ctrl Pts',(-0.204262719720836,0.0021612997731543,
0.00864368340093128));
#43656=CARTESIAN_POINT('Ctrl Pts',(-0.204363887539702,0.00217154023637526,
0.00865137136587931));
#43657=CARTESIAN_POINT('Ctrl Pts',(-0.20412805707869,0.00305073619898106,
0.00913959446919662));
#43658=CARTESIAN_POINT('Ctrl Pts',(-0.20412547082334,0.0030014403681275,
0.00922956938389137));
#43659=CARTESIAN_POINT('Ctrl Pts',(-0.204226293290499,0.00301522546561237,
0.00923757183785008));
#43660=CARTESIAN_POINT('Ctrl Pts',(-0.203844723877951,0.00493114335503218,
0.0100298425834166));
#43661=CARTESIAN_POINT('Ctrl Pts',(-0.203841781000808,0.00490291518671609,
0.0101297327317632));
#43662=CARTESIAN_POINT('Ctrl Pts',(-0.203944568193161,0.00490313323676524,
0.0101279022979083));
#43663=CARTESIAN_POINT('Ctrl Pts',(-0.20405840197198,0.00700620797942271,
0.0102626710355198));
#43664=CARTESIAN_POINT('Ctrl Pts',(-0.204055332333839,0.00700060634176611,
0.0103650944362403));
#43665=CARTESIAN_POINT('Ctrl Pts',(-0.204156747239523,0.00699020166858962,
0.0103656362115123));
#43666=CARTESIAN_POINT('Ctrl Pts',(-0.204143719711716,0.00802360799215748,
0.0102055713602495));
#43667=CARTESIAN_POINT('Ctrl Pts',(-0.204140674006327,0.00802944118873702,
0.0103073413719115));
#43668=CARTESIAN_POINT('Ctrl Pts',(-0.204242315972835,0.00802109309748085,
0.0103088959211302));
#43669=CARTESIAN_POINT('Ctrl Pts',(-0.204098734059757,0.00749980245225468,
0.0102204145824933));
#43670=CARTESIAN_POINT('Ctrl Pts',(-0.204098586165758,0.00749980223570916,
0.0102269586333304));
#43671=CARTESIAN_POINT('Ctrl Pts',(-0.204099083587065,0.00749980221762655,
0.0102335010073826));
#43672=CARTESIAN_POINT('Ctrl Pts',(-0.204101426216882,0.00749980258329951,
0.0102468033715967));
#43673=CARTESIAN_POINT('Ctrl Pts',(-0.204103348425244,0.00749980299171968,
0.0102535135368467));
#43674=CARTESIAN_POINT('Ctrl Pts',(-0.204110773522535,0.00749980474828837,
0.0102719151173418));
#43675=CARTESIAN_POINT('Ctrl Pts',(-0.204117860546261,0.00749980659017663,
0.010282814526926));
#43676=CARTESIAN_POINT('Ctrl Pts',(-0.204135778200342,0.00749981131633409,
0.0103013367558254));
#43677=CARTESIAN_POINT('Ctrl Pts',(-0.204146442862644,0.00749981423845238,
0.0103087851890371));
#43678=CARTESIAN_POINT('Ctrl Pts',(-0.204168352148334,0.0074998193372597,
0.0103185181067941));
#43679=CARTESIAN_POINT('Ctrl Pts',(-0.204179148198187,0.0074998348658371,
0.0103213088532629));
#43680=CARTESIAN_POINT('Ctrl Pts',(-0.204192371349525,0.00749981086548528,
0.0103224861895429));
#43681=CARTESIAN_POINT('Ctrl Pts',(-0.204194612627097,0.00749983027531024,
0.0103226110687671));
#43682=CARTESIAN_POINT('Ctrl Pts',(-0.204196825282634,0.00749983099238885,
0.0103226610749368));
#43683=CARTESIAN_POINT('Ctrl Pts',(-0.204143994057702,0.00697676071699483,
0.0102055666886271));
#43684=CARTESIAN_POINT('Ctrl Pts',(-0.2041408601556,0.00697091981646658,
0.0103074234560016));
#43685=CARTESIAN_POINT('Ctrl Pts',(-0.204242585767289,0.00697933425661569,
0.0103089798359738));
#43686=CARTESIAN_POINT('Ctrl Pts',(-0.204058114946837,0.0079928086477191,
0.0102622888245846));
#43687=CARTESIAN_POINT('Ctrl Pts',(-0.204054957478253,0.00799839543298179,
0.0103647962811805));
#43688=CARTESIAN_POINT('Ctrl Pts',(-0.204156454632279,0.00800888585074875,
0.0103653299370992));
#43689=CARTESIAN_POINT('Ctrl Pts',(-0.203843707641205,0.0100628925980128,
0.0100315736472558));
#43690=CARTESIAN_POINT('Ctrl Pts',(-0.203840675038655,0.0100910782349306,
0.0101315715362989));
#43691=CARTESIAN_POINT('Ctrl Pts',(-0.203943552101339,0.0100908447850691,
0.0101297390895283));
#43692=CARTESIAN_POINT('Ctrl Pts',(-0.204127325890448,0.0119475991503093,
0.00914023055516254));
#43693=CARTESIAN_POINT('Ctrl Pts',(-0.204124652395982,0.0119969311050922,
0.00923028348964983));
#43694=CARTESIAN_POINT('Ctrl Pts',(-0.204225570130192,0.0119831834122565,
0.00923826131726373));
#43695=CARTESIAN_POINT('Ctrl Pts',(-0.204263055354891,0.0127748578564395,
0.00856365183920312));
#43696=CARTESIAN_POINT('Ctrl Pts',(-0.204260624482029,0.0128332000492351,
0.00864736250104337));
#43697=CARTESIAN_POINT('Ctrl Pts',(-0.204361886645732,0.0128229809829309,
0.00865502158265919));
#43698=CARTESIAN_POINT('Ctrl Pts',(-0.205143217748733,0.00801648272260619,
0.0102288513503545));
#43699=CARTESIAN_POINT('Ctrl Pts',(-0.205141397070134,0.00802259035131162,
0.0103355159558339));
#43700=CARTESIAN_POINT('Ctrl Pts',(-0.205035270082177,0.00803097181891989,
0.0103261045172673));
#43701=CARTESIAN_POINT('Ctrl Pts',(-0.205056278613804,0.00699374265691425,
0.0102848962094768));
#43702=CARTESIAN_POINT('Ctrl Pts',(-0.205054440918194,0.0069878185985912,
0.0103922540218368));
#43703=CARTESIAN_POINT('Ctrl Pts',(-0.204948544649311,0.00699911071925452,
0.0103838328287035));
#43704=CARTESIAN_POINT('Ctrl Pts',(-0.204846431243139,0.00493848158252054,
0.0100498578329968));
#43705=CARTESIAN_POINT('Ctrl Pts',(-0.204844691090855,0.00490894474163874,
0.0101545286263539));
#43706=CARTESIAN_POINT('Ctrl Pts',(-0.204737314569065,0.0049109166968098,
0.0101488940353842));
#43707=CARTESIAN_POINT('Ctrl Pts',(-0.205124469597499,0.00307519585421071,
0.00917342141693886));
#43708=CARTESIAN_POINT('Ctrl Pts',(-0.205123141870177,0.00302363744285394,
0.00926778892652763));
#43709=CARTESIAN_POINT('Ctrl Pts',(-0.205017814730547,0.00301308425163072,
0.0092525626970204));
#43710=CARTESIAN_POINT('Ctrl Pts',(-0.205262224641199,0.00223986690673841,
0.00859354485513374));
#43711=CARTESIAN_POINT('Ctrl Pts',(-0.20526114296998,0.00217880555930881,
0.00868121881747347));
#43712=CARTESIAN_POINT('Ctrl Pts',(-0.205155455117607,0.00217252875054394,
0.00866676529248969));
#43713=CARTESIAN_POINT('Ctrl Pts',(-0.205092334702737,0.00260645295233614,
0.00895141938274717));
#43714=CARTESIAN_POINT('Ctrl Pts',(-0.205093133563206,0.0026072343879083,
0.00895191840030636));
#43715=CARTESIAN_POINT('Ctrl Pts',(-0.205095258409959,0.0026092688461218,
0.00895318228735311));
#43716=CARTESIAN_POINT('Ctrl Pts',(-0.205097375225393,0.00261136069190115,
0.00895436288913649));
#43717=CARTESIAN_POINT('Ctrl Pts',(-0.205104532774812,0.00261875781133091,
0.00895843071484043));
#43718=CARTESIAN_POINT('Ctrl Pts',(-0.205114102664032,0.00262887791286909,
0.00896304924228411));
#43719=CARTESIAN_POINT('Ctrl Pts',(-0.205133688318084,0.00265257222454595,
0.00896757768358735));
#43720=CARTESIAN_POINT('Ctrl Pts',(-0.205142252981025,0.00266387538604602,
0.00896793796110294));
#43721=CARTESIAN_POINT('Ctrl Pts',(-0.205158606120922,0.00268796880691882,
0.00896430844256256));
#43722=CARTESIAN_POINT('Ctrl Pts',(-0.20516571311459,0.00270003373063085,
0.00895998919280492));
#43723=CARTESIAN_POINT('Ctrl Pts',(-0.20517434484453,0.00271780094254793,
0.00894940393856633));
#43724=CARTESIAN_POINT('Ctrl Pts',(-0.205177025557873,0.00272433601707078,
0.0089443725583336));
#43725=CARTESIAN_POINT('Ctrl Pts',(-0.205180497843194,0.00273564720144894,
0.00893298795623472));
#43726=CARTESIAN_POINT('Ctrl Pts',(-0.205181416246512,0.00274041875726572,
0.00892693338808831));
#43727=CARTESIAN_POINT('Ctrl Pts',(-0.20518154308962,0.00274447060991368,
0.00892030161323929));
#43728=CARTESIAN_POINT('Ctrl Pts',(-0.205098436543116,0.00749984782009145,
0.010243256758359));
#43729=CARTESIAN_POINT('Ctrl Pts',(-0.205098274430575,0.00749984762351407,
0.0102497175728602));
#43730=CARTESIAN_POINT('Ctrl Pts',(-0.205097483994373,0.00749984725475431,
0.0102561471696715));
#43731=CARTESIAN_POINT('Ctrl Pts',(-0.2050945605171,0.00749984612943716,
0.0102692497779461));
#43732=CARTESIAN_POINT('Ctrl Pts',(-0.205092336917074,0.00749984534854801,
0.0102758663933169));
#43733=CARTESIAN_POINT('Ctrl Pts',(-0.205084087417224,0.00749984256928602,
0.0102939138606672));
#43734=CARTESIAN_POINT('Ctrl Pts',(-0.205076514757121,0.00749984013949185,
0.0103044818481159));
#43735=CARTESIAN_POINT('Ctrl Pts',(-0.20505777758101,0.00749983400823954,
0.0103221754888335));
#43736=CARTESIAN_POINT('Ctrl Pts',(-0.205046786694621,0.00749983051795828,
0.0103291343648038));
#43737=CARTESIAN_POINT('Ctrl Pts',(-0.20502348624436,0.00749982117772525,
0.0103382476987318));
#43738=CARTESIAN_POINT('Ctrl Pts',(-0.205012451916365,0.00749983699066525,
0.0103402134687604));
#43739=CARTESIAN_POINT('Ctrl Pts',(-0.205000337272074,0.00749978528464776,
0.0103407438028927));
#43740=CARTESIAN_POINT('Ctrl Pts',(-0.20499801233247,0.00749981993605052,
0.0103407686501798));
#43741=CARTESIAN_POINT('Ctrl Pts',(-0.204995837238769,0.0074998193282587,
0.0103407196921656));
#43742=CARTESIAN_POINT('Ctrl Pts',(-0.205260925816527,0.0127573393964206,
0.0085954370355821));
#43743=CARTESIAN_POINT('Ctrl Pts',(-0.205259981441613,0.012818177596082,
0.00868288953285713));
#43744=CARTESIAN_POINT('Ctrl Pts',(-0.205154563041824,0.0128246666377038,
0.00866886932633953));
#43745=CARTESIAN_POINT('Ctrl Pts',(-0.20512350504628,0.011918896615286,
0.00917641659755658));
#43746=CARTESIAN_POINT('Ctrl Pts',(-0.205122314353347,0.0119702189154387,
0.00927055622826414));
#43747=CARTESIAN_POINT('Ctrl Pts',(-0.205017252916804,0.0119808957925622,
0.00925580328110713));
#43748=CARTESIAN_POINT('Ctrl Pts',(-0.204846130960769,0.010062506110505,
0.0100487182598789));
#43749=CARTESIAN_POINT('Ctrl Pts',(-0.20484453360047,0.0100919672421221,
0.0101530708413611));
#43750=CARTESIAN_POINT('Ctrl Pts',(-0.204737436020278,0.0100902502137758,
0.010147851443999));
#43751=CARTESIAN_POINT('Ctrl Pts',(-0.205055807234136,0.00800548029823725,
0.0102849382972628));
#43752=CARTESIAN_POINT('Ctrl Pts',(-0.205054110390278,0.00801139161403613,
0.010391986660739));
#43753=CARTESIAN_POINT('Ctrl Pts',(-0.204948492565434,0.00800006338884696,
0.0103840497641343));
#43754=CARTESIAN_POINT('Ctrl Pts',(-0.205143559896196,0.00698344979987348,
0.0102286690008394));
#43755=CARTESIAN_POINT('Ctrl Pts',(-0.205141880339568,0.00697737023664258,
0.0103350246469026));
#43756=CARTESIAN_POINT('Ctrl Pts',(-0.205036031913016,0.00696893486623635,
0.0103260790360151));
#43757=CARTESIAN_POINT('Ctrl Pts',(-0.205180445672117,0.0122517034922546,
0.00892259327448536));
#43758=CARTESIAN_POINT('Ctrl Pts',(-0.205180323054652,0.0122556110563871,
0.00892899712366704));
#43759=CARTESIAN_POINT('Ctrl Pts',(-0.20517946244098,0.0122601909823991,
0.00893486620714245));
#43760=CARTESIAN_POINT('Ctrl Pts',(-0.205176214037774,0.0122710085088525,
0.00894594287415477));
#43761=CARTESIAN_POINT('Ctrl Pts',(-0.205173710804417,0.0122772429515444,
0.00895088031987881));
#43762=CARTESIAN_POINT('Ctrl Pts',(-0.205165499740559,0.0122944821254439,
0.00896156581316046));
#43763=CARTESIAN_POINT('Ctrl Pts',(-0.205158619362418,0.0123063363280765,
0.00896607202978781));
#43764=CARTESIAN_POINT('Ctrl Pts',(-0.205142087193769,0.0123309994366319,
0.00897032808637686));
#43765=CARTESIAN_POINT('Ctrl Pts',(-0.205132977416631,0.0123430619084986,
0.00897004433852129));
#43766=CARTESIAN_POINT('Ctrl Pts',(-0.205109337949273,0.012371579399479,
0.00896456266879536));
#43767=CARTESIAN_POINT('Ctrl Pts',(-0.20509769511444,0.0123831368420804,
0.00895767977417679));
#43768=CARTESIAN_POINT('Ctrl Pts',(-0.205093745802734,0.0123869198976546,
0.00895550568412799));
#43769=CARTESIAN_POINT('Ctrl Pts',(-0.205092545621893,0.0123883647568986,
0.00895462655013412));
#43770=CARTESIAN_POINT('Ctrl Pts',(-0.205091196983166,0.0123896832404942,
0.00895378545522166));
#43771=CARTESIAN_POINT('Origin',(-0.206344955241137,0.00266032655011837,
0.00889192021703303));
#43772=CARTESIAN_POINT('Ctrl Pts',(-0.206181807720331,0.00274488366429473,
0.00894172134960159));
#43773=CARTESIAN_POINT('Ctrl Pts',(-0.206181777333857,0.00274074553468597,
0.00894832213101722));
#43774=CARTESIAN_POINT('Ctrl Pts',(-0.206182782627333,0.00273591857292603,
0.00895433149772863));
#43775=CARTESIAN_POINT('Ctrl Pts',(-0.2061869987975,0.00272417054420443,
0.00896607038342512));
#43776=CARTESIAN_POINT('Ctrl Pts',(-0.206190524634843,0.00271722901686468,
0.0089713181216008));
#43777=CARTESIAN_POINT('Ctrl Pts',(-0.206201693107854,0.00269891001608653,
0.00898211194303197));
#43778=CARTESIAN_POINT('Ctrl Pts',(-0.206210965191943,0.00268656061040968,
0.00898653002283859));
#43779=CARTESIAN_POINT('Ctrl Pts',(-0.206232328954445,0.00266213443912686,
0.00899030799369234));
#43780=CARTESIAN_POINT('Ctrl Pts',(-0.206243446851708,0.00265085165508385,
0.00899000345364994));
#43781=CARTESIAN_POINT('Ctrl Pts',(-0.206271503877879,0.00262488401632038,
0.00898530206088853));
#43782=CARTESIAN_POINT('Ctrl Pts',(-0.20628521595814,0.00261433437329706,
0.00897961320218937));
#43783=CARTESIAN_POINT('Ctrl Pts',(-0.206290127794076,0.0026107230526453,
0.00897768264932748));
#43784=CARTESIAN_POINT('Ctrl Pts',(-0.206291273089138,0.00260976640865154,
0.00897714670056697));
#43785=CARTESIAN_POINT('Ctrl Pts',(-0.206292808630783,0.0026084913937421,
0.00897641700608666));
#43786=CARTESIAN_POINT('Ctrl Pts',(-0.206294003176714,0.00260759611925214,
0.00897588559731814));
#43787=CARTESIAN_POINT('Origin',(-0.205019744048073,0.0123372008288139,
0.00886724630700698));
#43788=CARTESIAN_POINT('Ctrl Pts',(-0.206181037530589,0.0122515254343705,
0.00894387539800756));
#43789=CARTESIAN_POINT('Ctrl Pts',(-0.206181008360377,0.0122555416227814,
0.00895028645839285));
#43790=CARTESIAN_POINT('Ctrl Pts',(-0.206181955433058,0.0122602096263031,
0.00895614280721616));
#43791=CARTESIAN_POINT('Ctrl Pts',(-0.206185935826737,0.0122715473608068,
0.00896762203649176));
#43792=CARTESIAN_POINT('Ctrl Pts',(-0.206189265738046,0.0122782394074966,
0.00897279547154573));
#43793=CARTESIAN_POINT('Ctrl Pts',(-0.206199956453773,0.0122961040213282,
0.00898364839558845));
#43794=CARTESIAN_POINT('Ctrl Pts',(-0.206208936856501,0.0123082440318456,
0.0089882064826025));
#43795=CARTESIAN_POINT('Ctrl Pts',(-0.206229707690682,0.0123323170437131,
0.00899236976530477));
#43796=CARTESIAN_POINT('Ctrl Pts',(-0.20624053610774,0.0123434551022436,
0.00899229343561907));
#43797=CARTESIAN_POINT('Ctrl Pts',(-0.206265161532738,0.012366592468694,
0.00898864163563936));
#43798=CARTESIAN_POINT('Ctrl Pts',(-0.206277327979804,0.0123765295081089,
0.00898454730676776));
#43799=CARTESIAN_POINT('Ctrl Pts',(-0.206286691450758,0.0123839492220929,
0.0089807883441402));
#43800=CARTESIAN_POINT('Ctrl Pts',(-0.206289406067974,0.012386018586932,
0.00897971337216977));
#43801=CARTESIAN_POINT('Ctrl Pts',(-0.20629212794999,0.0123880284654335,
0.00897855924406012));
#43802=CARTESIAN_POINT('Ctrl Pts',(-0.206293185535286,0.0123888219494838,
0.00897808876183893));
#43803=CARTESIAN_POINT('Ctrl Pts',(-0.206265361080271,0.00222221827535806,
0.00859997798124637));
#43804=CARTESIAN_POINT('Ctrl Pts',(-0.206263035706064,0.00216379824786295,
0.00868332185176802));
#43805=CARTESIAN_POINT('Ctrl Pts',(-0.206364035202085,0.00217391790280425,
0.00869114406698921));
#43806=CARTESIAN_POINT('Ctrl Pts',(-0.206129039916538,0.00305219375783605,
0.00918130268389152));
#43807=CARTESIAN_POINT('Ctrl Pts',(-0.206126471811688,0.00300282276552956,
0.00927104603765872));
#43808=CARTESIAN_POINT('Ctrl Pts',(-0.206227126009343,0.00301644299843148,
0.00927918109642607));
#43809=CARTESIAN_POINT('Ctrl Pts',(-0.205843114295396,0.00493078093842745,
0.0100742895591365));
#43810=CARTESIAN_POINT('Ctrl Pts',(-0.20584019217099,0.00490250351805925,
0.0101739988347731));
#43811=CARTESIAN_POINT('Ctrl Pts',(-0.205942808907154,0.0049029244902082,
0.010172369914728));
#43812=CARTESIAN_POINT('Ctrl Pts',(-0.206056905126677,0.00700670674502859,
0.010308041670639));
#43813=CARTESIAN_POINT('Ctrl Pts',(-0.206053855846052,0.00700109571471318,
0.0104102978886477));
#43814=CARTESIAN_POINT('Ctrl Pts',(-0.206155087564965,0.00699052260417267,
0.0104109705696189));
#43815=CARTESIAN_POINT('Ctrl Pts',(-0.206143835444834,0.00802364330158489,
0.010250719836519));
#43816=CARTESIAN_POINT('Ctrl Pts',(-0.206140810023571,0.0080294871033969,
0.0103523190431676));
#43817=CARTESIAN_POINT('Ctrl Pts',(-0.206242270945703,0.00802106546893099,
0.0103540384991376));
#43818=CARTESIAN_POINT('Ctrl Pts',(-0.206098144959998,0.00749989479917323,
0.0102656028080008));
#43819=CARTESIAN_POINT('Ctrl Pts',(-0.206097997059586,0.00749989463897083,
0.0102721471703159));
#43820=CARTESIAN_POINT('Ctrl Pts',(-0.206098494595543,0.00749989465445635,
0.0102786898446544));
#43821=CARTESIAN_POINT('Ctrl Pts',(-0.206100837702042,0.00749989504069795,
0.0102919928424395));
#43822=CARTESIAN_POINT('Ctrl Pts',(-0.206102760293655,0.00749989543298072,
0.0102987033059631));
#43823=CARTESIAN_POINT('Ctrl Pts',(-0.206110186665226,0.00749989706680563,
0.0103171052918464));
#43824=CARTESIAN_POINT('Ctrl Pts',(-0.206117274672292,0.00749989873859384,
0.0103280045983479));
#43825=CARTESIAN_POINT('Ctrl Pts',(-0.206135194433958,0.0074999029495758,
0.010346526573871));
#43826=CARTESIAN_POINT('Ctrl Pts',(-0.206145860283699,0.00749990553928964,
0.0103539747648798));
#43827=CARTESIAN_POINT('Ctrl Pts',(-0.206167772870826,0.00749990981405412,
0.0103637077806601));
#43828=CARTESIAN_POINT('Ctrl Pts',(-0.206178569199203,0.00749992615583955,
0.0103664975019689));
#43829=CARTESIAN_POINT('Ctrl Pts',(-0.206191787570224,0.00749989903157803,
0.0103676744623668));
#43830=CARTESIAN_POINT('Ctrl Pts',(-0.206194034750604,0.00749992015594775,
0.0103677996707739));
#43831=CARTESIAN_POINT('Ctrl Pts',(-0.206196245004281,0.00749992079740314,
0.0103678496339236));
#43832=CARTESIAN_POINT('Ctrl Pts',(-0.206144104594209,0.00697680057252784,
0.0102506660646432));
#43833=CARTESIAN_POINT('Ctrl Pts',(-0.206140934104293,0.00697094762846495,
0.0103523029798102));
#43834=CARTESIAN_POINT('Ctrl Pts',(-0.206242430803,0.00697941470148986,
0.0103541300309738));
#43835=CARTESIAN_POINT('Ctrl Pts',(-0.206056577677555,0.00799264761430986,
0.0103075953740775));
#43836=CARTESIAN_POINT('Ctrl Pts',(-0.206053383823223,0.0079982387982383,
0.0104098867566766));
#43837=CARTESIAN_POINT('Ctrl Pts',(-0.206154650474734,0.008008907775399,
0.0104106527590022));
#43838=CARTESIAN_POINT('Ctrl Pts',(-0.205842604186409,0.0100635095616092,
0.0100759104351038));
#43839=CARTESIAN_POINT('Ctrl Pts',(-0.205839534753177,0.0100917343277227,
0.0101756804741991));
#43840=CARTESIAN_POINT('Ctrl Pts',(-0.205942191076445,0.0100912285879667,
0.0101741825465384));
#43841=CARTESIAN_POINT('Ctrl Pts',(-0.206128983923121,0.0119465421786305,
0.00918167990255796));
#43842=CARTESIAN_POINT('Ctrl Pts',(-0.206126272027682,0.0119959385645935,
0.0092714515540072));
#43843=CARTESIAN_POINT('Ctrl Pts',(-0.206226974205861,0.011982429450636,
0.00927964772645204));
#43844=CARTESIAN_POINT('Ctrl Pts',(-0.206264007846902,0.0127726530819234,
0.00860324800585114));
#43845=CARTESIAN_POINT('Ctrl Pts',(-0.206261537061061,0.0128310540613221,
0.00868665044708584));
#43846=CARTESIAN_POINT('Ctrl Pts',(-0.206362583389019,0.0128210156501638,
0.00869452929791549));
#43847=CARTESIAN_POINT('Ctrl Pts',(-0.207142444673933,0.00800781553972708,
0.010275022722237));
#43848=CARTESIAN_POINT('Ctrl Pts',(-0.207140064658573,0.0080138362133013,
0.0103806849379504));
#43849=CARTESIAN_POINT('Ctrl Pts',(-0.207034903442016,0.00802228009373349,
0.0103717639889522));
#43850=CARTESIAN_POINT('Ctrl Pts',(-0.207054099445209,0.00698801037561799,
0.0103300780697022));
#43851=CARTESIAN_POINT('Ctrl Pts',(-0.2070517042754,0.00698211378551127,
0.0104364239726335));
#43852=CARTESIAN_POINT('Ctrl Pts',(-0.206946767716351,0.00699343558996355,
0.0104285245883844));
#43853=CARTESIAN_POINT('Ctrl Pts',(-0.206845339015377,0.0049362023550447,
0.0100937709797338));
#43854=CARTESIAN_POINT('Ctrl Pts',(-0.206843032419443,0.00490681719228294,
0.0101974457807158));
#43855=CARTESIAN_POINT('Ctrl Pts',(-0.206736622083599,0.00490835191115651,
0.010192192130957));
#43856=CARTESIAN_POINT('Ctrl Pts',(-0.207125456189955,0.00307642210849726,
0.00921573551924576));
#43857=CARTESIAN_POINT('Ctrl Pts',(-0.207123567613966,0.0030251050994184,
0.0093090903467788));
#43858=CARTESIAN_POINT('Ctrl Pts',(-0.207019188297482,0.0030145359074727,
0.00929436328058973));
#43859=CARTESIAN_POINT('Ctrl Pts',(-0.207262560200634,0.00224233294950047,
0.00863411935968771));
#43860=CARTESIAN_POINT('Ctrl Pts',(-0.207260912515351,0.00218160679793509,
0.00872080422753244));
#43861=CARTESIAN_POINT('Ctrl Pts',(-0.207156176888109,0.00217517650829302,
0.00870680543946287));
#43862=CARTESIAN_POINT('Ctrl Pts',(-0.207092854540501,0.00260851289160005,
0.00899226593441351));
#43863=CARTESIAN_POINT('Ctrl Pts',(-0.207093661671656,0.00260930138402402,
0.00899277156336772));
#43864=CARTESIAN_POINT('Ctrl Pts',(-0.207095778208369,0.00261132664878968,
0.00899403454397879));
#43865=CARTESIAN_POINT('Ctrl Pts',(-0.207097886856061,0.00261340871206773,
0.00899521536690078));
#43866=CARTESIAN_POINT('Ctrl Pts',(-0.20710509653825,0.00262084830596442,
0.00899932471837138));
#43867=CARTESIAN_POINT('Ctrl Pts',(-0.207114650508154,0.00263094785655132,
0.00900394444985275));
#43868=CARTESIAN_POINT('Ctrl Pts',(-0.207134211351354,0.00265460158472104,
0.00900851090477576));
#43869=CARTESIAN_POINT('Ctrl Pts',(-0.207142776523973,0.00266590395548275,
0.00900889219077089));
#43870=CARTESIAN_POINT('Ctrl Pts',(-0.207159130351548,0.00269000365493396,
0.00900530727549867));
#43871=CARTESIAN_POINT('Ctrl Pts',(-0.20716623750744,0.00270207623203594,
0.00900101040587168));
#43872=CARTESIAN_POINT('Ctrl Pts',(-0.207174869590674,0.00271986271764353,
0.0089904581290781));
#43873=CARTESIAN_POINT('Ctrl Pts',(-0.20717755046045,0.00272640706578969,
0.00898543882878451));
#43874=CARTESIAN_POINT('Ctrl Pts',(-0.207181023031312,0.00273773927407138,
0.00897407515034856));
#43875=CARTESIAN_POINT('Ctrl Pts',(-0.207181941566556,0.00274252203293754,
0.00896802941304953));
#43876=CARTESIAN_POINT('Ctrl Pts',(-0.207182068536114,0.00274658618351931,
0.0089614051446851));
#43877=CARTESIAN_POINT('Ctrl Pts',(-0.207097776915989,0.00750000158973935,
0.010288431808782));
#43878=CARTESIAN_POINT('Ctrl Pts',(-0.207097615449255,0.00750000150078048,
0.010294896926047));
#43879=CARTESIAN_POINT('Ctrl Pts',(-0.207096824768248,0.00750000127095302,
0.0103013308258036));
#43880=CARTESIAN_POINT('Ctrl Pts',(-0.207093899892511,0.00750000049420602,
0.0103144379848226));
#43881=CARTESIAN_POINT('Ctrl Pts',(-0.207091675856147,0.00749999992679673,
0.010321054956798));
#43882=CARTESIAN_POINT('Ctrl Pts',(-0.207083424988614,0.00749999783641234,
0.0103391027987811));
#43883=CARTESIAN_POINT('Ctrl Pts',(-0.207075851344921,0.00749999594507674,
0.0103496706025116));
#43884=CARTESIAN_POINT('Ctrl Pts',(-0.207057112101686,0.00749999098558329,
0.010367363790383));
#43885=CARTESIAN_POINT('Ctrl Pts',(-0.207046120079705,0.00749998813306785,
0.0103743223145231));
#43886=CARTESIAN_POINT('Ctrl Pts',(-0.207022666561015,0.00749997979926175,
0.0103834940223032));
#43887=CARTESIAN_POINT('Ctrl Pts',(-0.207011609070574,0.00749999733979672,
0.010385407894664));
#43888=CARTESIAN_POINT('Ctrl Pts',(-0.206999678146928,0.00749994229578302,
0.0103859299553424));
#43889=CARTESIAN_POINT('Ctrl Pts',(-0.206997332525893,0.00749998053119276,
0.0103859550031861));
#43890=CARTESIAN_POINT('Ctrl Pts',(-0.206995167637369,0.00749998003531992,
0.0103859062510846));
#43891=CARTESIAN_POINT('Ctrl Pts',(-0.207261886265387,0.0127551146813286,
0.00863509390574996));
#43892=CARTESIAN_POINT('Ctrl Pts',(-0.207261035868668,0.0128159573149126,
0.00872217657099504));
#43893=CARTESIAN_POINT('Ctrl Pts',(-0.207155887419512,0.0128226349039402,
0.0087085012780755));
#43894=CARTESIAN_POINT('Ctrl Pts',(-0.207125087189744,0.0119178974994294,
0.00921790212244517));
#43895=CARTESIAN_POINT('Ctrl Pts',(-0.207123991865616,0.011969232742892,
0.00931169547144037));
#43896=CARTESIAN_POINT('Ctrl Pts',(-0.20701919820191,0.0119799828515178,
0.00929732829977912));
#43897=CARTESIAN_POINT('Ctrl Pts',(-0.206845110243081,0.0100626154563815,
0.0100931300888338));
#43898=CARTESIAN_POINT('Ctrl Pts',(-0.206843612318736,0.0100920921441639,
0.010197172067879));
#43899=CARTESIAN_POINT('Ctrl Pts',(-0.206736785445693,0.0100908119228757,
0.0101922846257381));
#43900=CARTESIAN_POINT('Ctrl Pts',(-0.207054259433642,0.00800547639790048,
0.0103301544768812));
#43901=CARTESIAN_POINT('Ctrl Pts',(-0.207052661366926,0.00801140287506987,
0.0104369044212851));
#43902=CARTESIAN_POINT('Ctrl Pts',(-0.206947322354661,0.00799994996548187,
0.010429412007676));
#43903=CARTESIAN_POINT('Ctrl Pts',(-0.207143516918877,0.00698371431586357,
0.0102737402097756));
#43904=CARTESIAN_POINT('Ctrl Pts',(-0.207141936092252,0.00697763980344933,
0.0103797958532295));
#43905=CARTESIAN_POINT('Ctrl Pts',(-0.207036365342542,0.00696912440198335,
0.0103712553903634));
#43906=CARTESIAN_POINT('Ctrl Pts',(-0.207181566227228,0.0122501673758382,
0.00896336754694151));
#43907=CARTESIAN_POINT('Ctrl Pts',(-0.207181443529624,0.0122540864740861,
0.00896976251367002));
#43908=CARTESIAN_POINT('Ctrl Pts',(-0.20718058317538,0.012258676661758,
0.00897562162657197));
#43909=CARTESIAN_POINT('Ctrl Pts',(-0.207177335976054,0.0122695128914114,
0.00898667546788692));
#43910=CARTESIAN_POINT('Ctrl Pts',(-0.207174833751635,0.0122757552730441,
0.00899160021002775));
#43911=CARTESIAN_POINT('Ctrl Pts',(-0.207166625261092,0.012293012287366,
0.0090022524895017));
#43912=CARTESIAN_POINT('Ctrl Pts',(-0.207159746438497,0.0123048741518531,
0.00900673653866809));
#43913=CARTESIAN_POINT('Ctrl Pts',(-0.207143242800486,0.0123295060202738,
0.00901094050830801));
#43914=CARTESIAN_POINT('Ctrl Pts',(-0.207134165724431,0.0123415303218528,
0.00901064297181319));
#43915=CARTESIAN_POINT('Ctrl Pts',(-0.207115612578345,0.0123639197185274,
0.00900632226716967));
#43916=CARTESIAN_POINT('Ctrl Pts',(-0.207106180654793,0.0123745726871226,
0.00900226869215929));
#43917=CARTESIAN_POINT('Ctrl Pts',(-0.207094994078381,0.0123853378653371,
0.00899608376006582));
#43918=CARTESIAN_POINT('Ctrl Pts',(-0.20709372520993,0.0123868362173346,
0.00899517010746788));
#43919=CARTESIAN_POINT('Ctrl Pts',(-0.207092315986968,0.012388212238266,
0.00899428849862686));
#43920=CARTESIAN_POINT('Origin',(-0.208345484142396,0.00266244643750944,
0.0089328629507606));
#43921=CARTESIAN_POINT('Ctrl Pts',(-0.208182309222901,0.00274692227615215,
0.00898281378318786));
#43922=CARTESIAN_POINT('Ctrl Pts',(-0.208182277952001,0.00274277083451149,
0.0089894098019654));
#43923=CARTESIAN_POINT('Ctrl Pts',(-0.208183283209678,0.00273793104540203,
0.00899541268676956));
#43924=CARTESIAN_POINT('Ctrl Pts',(-0.208187499969814,0.00272615894310283,
0.00900713179321195));
#43925=CARTESIAN_POINT('Ctrl Pts',(-0.208191025783579,0.00271920742887892,
0.00901236665814065));
#43926=CARTESIAN_POINT('Ctrl Pts',(-0.208202194255079,0.00270086747218974,
0.00902312656656882));
#43927=CARTESIAN_POINT('Ctrl Pts',(-0.20821146643949,0.00268850905365718,
0.00902752167695764));
#43928=CARTESIAN_POINT('Ctrl Pts',(-0.208232757864608,0.00266415672876088,
0.00903124128829879));
#43929=CARTESIAN_POINT('Ctrl Pts',(-0.208243789470648,0.00265295194952518,
0.00903093244186576));
#43930=CARTESIAN_POINT('Ctrl Pts',(-0.208266197965404,0.0026321884360446,
0.00902718224347479));
#43931=CARTESIAN_POINT('Ctrl Pts',(-0.208277625842864,0.00262232779038878,
0.00902366625820533));
#43932=CARTESIAN_POINT('Ctrl Pts',(-0.208291122506059,0.00261230317031573,
0.00901833264904263));
#43933=CARTESIAN_POINT('Ctrl Pts',(-0.208292752737439,0.00261086851622097,
0.00901750864256678));
#43934=CARTESIAN_POINT('Ctrl Pts',(-0.208294498840167,0.00260956111026396,
0.00901672932862339));
#43935=CARTESIAN_POINT('Origin',(-0.207020842672714,0.0123355638655574,
0.00890784819837363));
#43936=CARTESIAN_POINT('Ctrl Pts',(-0.208182119617078,0.0122499879746583,
0.00898468528329885));
#43937=CARTESIAN_POINT('Ctrl Pts',(-0.208182089694991,0.0122540172315659,
0.0089910909843969));
#43938=CARTESIAN_POINT('Ctrl Pts',(-0.208183036687498,0.0122586976544962,
0.00899694045039098));
#43939=CARTESIAN_POINT('Ctrl Pts',(-0.208187017406401,0.0122700585909288,
0.00900839967133868));
#43940=CARTESIAN_POINT('Ctrl Pts',(-0.208190347149437,0.0122767602329116,
0.0090135603977819));
#43941=CARTESIAN_POINT('Ctrl Pts',(-0.208201037604085,0.0122946451894827,
0.00902437981604124));
#43942=CARTESIAN_POINT('Ctrl Pts',(-0.208210017974045,0.0123067937546356,
0.00902891519986445));
#43943=CARTESIAN_POINT('Ctrl Pts',(-0.208230788381485,0.0123308742080499,
0.00903303342014732));
#43944=CARTESIAN_POINT('Ctrl Pts',(-0.208241616538774,0.0123420119266663,
0.00903293626524176));
#43945=CARTESIAN_POINT('Ctrl Pts',(-0.208265385785225,0.0123643383350005,
0.00902936943810583));
#43946=CARTESIAN_POINT('Ctrl Pts',(-0.208277296931519,0.0123741925119681,
0.00902557501439544));
#43947=CARTESIAN_POINT('Ctrl Pts',(-0.208287775341226,0.0123824863977806,
0.00902135349364886));
#43948=CARTESIAN_POINT('Ctrl Pts',(-0.208290484416003,0.0123845498665015,
0.00902027628333439));
#43949=CARTESIAN_POINT('Ctrl Pts',(-0.208293200976528,0.0123865543346131,
0.00901912040146179));
#43950=CARTESIAN_POINT('Ctrl Pts',(-0.208294263946347,0.0123873509824498,
0.0090186459804785));
#43951=CARTESIAN_POINT('Ctrl Pts',(-0.208254768538843,0.00229164450644493,
0.00868658687555039));
#43952=CARTESIAN_POINT('Ctrl Pts',(-0.20825245751503,0.00223391860146863,
0.00877013646409537));
#43953=CARTESIAN_POINT('Ctrl Pts',(-0.208353202742803,0.00224414377019507,
0.00877813922762492));
#43954=CARTESIAN_POINT('Ctrl Pts',(-0.208122384277123,0.00310399998892067,
0.00924699455230831));
#43955=CARTESIAN_POINT('Ctrl Pts',(-0.208119840484776,0.00305516247643459,
0.00933672629287622));
#43956=CARTESIAN_POINT('Ctrl Pts',(-0.208220318667977,0.00306823181203351,
0.00934476558783898));
#43957=CARTESIAN_POINT('Ctrl Pts',(-0.207848303618453,0.00493309708019399,
0.0101100452809943));
#43958=CARTESIAN_POINT('Ctrl Pts',(-0.207845421398244,0.0049048112167105,
0.0102094175693445));
#43959=CARTESIAN_POINT('Ctrl Pts',(-0.207947761301341,0.00490547979792474,
0.010208203470148));
#43960=CARTESIAN_POINT('Ctrl Pts',(-0.208049730569645,0.006951724782394,
0.0103470289032258));
#43961=CARTESIAN_POINT('Ctrl Pts',(-0.208046721415412,0.00694549324445781,
0.0104489865111578));
#43962=CARTESIAN_POINT('Ctrl Pts',(-0.208147746503408,0.00693506629254703,
0.0104497771185207));
#43963=CARTESIAN_POINT('Ctrl Pts',(-0.20813673385937,0.00794205725535903,
0.0103001245699642));
#43964=CARTESIAN_POINT('Ctrl Pts',(-0.208133744121088,0.00794698726026996,
0.0104015414775745));
#43965=CARTESIAN_POINT('Ctrl Pts',(-0.208234946083908,0.00793834125015301,
0.0104033834628677));
#43966=CARTESIAN_POINT('Ctrl Pts',(-0.208097498904532,0.00750000157090282,
0.0103107897516593));
#43967=CARTESIAN_POINT('Ctrl Pts',(-0.208097350998533,0.00750000147467617,
0.0103173344020294));
#43968=CARTESIAN_POINT('Ctrl Pts',(-0.208097848642823,0.00750000152421671,
0.0103238773537081));
#43969=CARTESIAN_POINT('Ctrl Pts',(-0.208100192198594,0.00750000191733527,
0.0103371809375536));
#43970=CARTESIAN_POINT('Ctrl Pts',(-0.208102115151153,0.00750000227840782,
0.0103438916765363));
#43971=CARTESIAN_POINT('Ctrl Pts',(-0.208109542727457,0.00750000372441253,
0.0103622940444594));
#43972=CARTESIAN_POINT('Ctrl Pts',(-0.208116631669298,0.00750000515796395,
0.0103731932565404));
#43973=CARTESIAN_POINT('Ctrl Pts',(-0.208134553438137,0.00750000867236801,
0.0103917150014214));
#43974=CARTESIAN_POINT('Ctrl Pts',(-0.20814522042124,0.00750001081833758,
0.0103991629677472));
#43975=CARTESIAN_POINT('Ctrl Pts',(-0.208167136522622,0.00750001403039175,
0.0104088962499627));
#43976=CARTESIAN_POINT('Ctrl Pts',(-0.208177933155013,0.00750003110817561,
0.0104116848717577));
#43977=CARTESIAN_POINT('Ctrl Pts',(-0.208191146075881,0.00750000062131712,
0.0104128614042931));
#43978=CARTESIAN_POINT('Ctrl Pts',(-0.208193399877725,0.00750002349787222,
0.0104129869823138));
#43979=CARTESIAN_POINT('Ctrl Pts',(-0.208195607365359,0.00750002403881075,
0.0104130368945439));
#43980=CARTESIAN_POINT('Ctrl Pts',(-0.208129717403001,0.00713943526630543,
0.0103043208883982));
#43981=CARTESIAN_POINT('Ctrl Pts',(-0.208127433729327,0.00713551312926382,
0.0104050179882739));
#43982=CARTESIAN_POINT('Ctrl Pts',(-0.208227838903267,0.00714426099060607,
0.0104068541862071));
#43983=CARTESIAN_POINT('Ctrl Pts',(-0.208043973659639,0.00810286960191034,
0.0103409197394026));
#43984=CARTESIAN_POINT('Ctrl Pts',(-0.208041674140705,0.00810972080058238,
0.0104420318495822));
#43985=CARTESIAN_POINT('Ctrl Pts',(-0.208141951845999,0.0081198345803917,
0.0104428483686937));
#43986=CARTESIAN_POINT('Ctrl Pts',(-0.207854652784077,0.0100593757296637,
0.010103906718878));
#43987=CARTESIAN_POINT('Ctrl Pts',(-0.207852485956685,0.01008736209812,
0.010202440838558));
#43988=CARTESIAN_POINT('Ctrl Pts',(-0.207953993445674,0.0100865744749508,
0.0102015120896318));
#43989=CARTESIAN_POINT('Ctrl Pts',(-0.208115460371667,0.0118454327588012,
0.00927136703343939));
#43990=CARTESIAN_POINT('Ctrl Pts',(-0.208113606081108,0.0118932388858219,
0.0093607345340023));
#43991=CARTESIAN_POINT('Ctrl Pts',(-0.20821336750236,0.011880714719645,
0.00936851289219113));
#43992=CARTESIAN_POINT('Ctrl Pts',(-0.208243338997617,0.0126380043079271,
0.00873539247773069));
#43993=CARTESIAN_POINT('Ctrl Pts',(-0.208241707494196,0.0126944515532892,
0.00881888793575907));
#43994=CARTESIAN_POINT('Ctrl Pts',(-0.20834166317492,0.0126841741346925,
0.00882686968717256));
#43995=CARTESIAN_POINT('Ctrl Pts',(-0.20914253069387,0.00800768546079551,
0.0103201868919279));
#43996=CARTESIAN_POINT('Ctrl Pts',(-0.209140158727521,0.00801370758595218,
0.0104254987444665));
#43997=CARTESIAN_POINT('Ctrl Pts',(-0.209035328314277,0.00802224413564764,
0.0104169409854339));
#43998=CARTESIAN_POINT('Ctrl Pts',(-0.209052502335453,0.00698800171825145,
0.0103753680037525));
#43999=CARTESIAN_POINT('Ctrl Pts',(-0.209050115505252,0.00698210423024609,
0.0104813658057015));
#44000=CARTESIAN_POINT('Ctrl Pts',(-0.20894551118575,0.00699356179921356,
0.0104738686489309));
#44001=CARTESIAN_POINT('Ctrl Pts',(-0.20884391279819,0.00493657161352178,
0.010138368073117));
#44002=CARTESIAN_POINT('Ctrl Pts',(-0.208841613705275,0.00490719070191681,
0.0102416870201151));
#44003=CARTESIAN_POINT('Ctrl Pts',(-0.208735525137882,0.0049083303013487,
0.0102367321435203));
#44004=CARTESIAN_POINT('Ctrl Pts',(-0.209126397964456,0.00307771249090385,
0.00925753373586065));
#44005=CARTESIAN_POINT('Ctrl Pts',(-0.209124514363621,0.00302640308937374,
0.00935049596620794));
#44006=CARTESIAN_POINT('Ctrl Pts',(-0.209020453031246,0.00301578732888502,
0.0093361236084367));
#44007=CARTESIAN_POINT('Ctrl Pts',(-0.209262833615147,0.00224487032025302,
0.00867419277172518));
#44008=CARTESIAN_POINT('Ctrl Pts',(-0.209261189107054,0.00218416846403701,
0.00876046668203946));
#44009=CARTESIAN_POINT('Ctrl Pts',(-0.209156773635649,0.00217758333808884,
0.00874678629964514));
#44010=CARTESIAN_POINT('Ctrl Pts',(-0.209093315567622,0.00261035486184449,
0.0090330700905398));
#44011=CARTESIAN_POINT('Ctrl Pts',(-0.209094120821064,0.00261114070661801,
0.00903357611206334));
#44012=CARTESIAN_POINT('Ctrl Pts',(-0.209096239518301,0.00261316568678703,
0.00903484434778787));
#44013=CARTESIAN_POINT('Ctrl Pts',(-0.209098350289981,0.00261524780172148,
0.00903603028854842));
#44014=CARTESIAN_POINT('Ctrl Pts',(-0.209105547676708,0.00262266893378366,
0.00904014786330693));
#44015=CARTESIAN_POINT('Ctrl Pts',(-0.209115105486559,0.00263276396907685,
0.00904479212974383));
#44016=CARTESIAN_POINT('Ctrl Pts',(-0.209134673402525,0.00265642100159974,
0.00904940747341608));
#44017=CARTESIAN_POINT('Ctrl Pts',(-0.209143238710959,0.00266772421138318,
0.00904981136009591));
#44018=CARTESIAN_POINT('Ctrl Pts',(-0.209159593323108,0.0026918341576449,
0.00904627431702745));
#44019=CARTESIAN_POINT('Ctrl Pts',(-0.209166700895917,0.00270391634463159,
0.0090420012009457));
#44020=CARTESIAN_POINT('Ctrl Pts',(-0.209175333936052,0.00272172484600436,
0.00903148343667792));
#44021=CARTESIAN_POINT('Ctrl Pts',(-0.209178015309464,0.00272827965420737,
0.00902647642775316));
#44022=CARTESIAN_POINT('Ctrl Pts',(-0.209181488583474,0.00273963457004301,
0.00901513347071432));
#44023=CARTESIAN_POINT('Ctrl Pts',(-0.209182407362429,0.00274442903389408,
0.00900909632180704));
#44024=CARTESIAN_POINT('Ctrl Pts',(-0.209182534463097,0.0027485057034167,
0.00900247906972172));
#44025=CARTESIAN_POINT('Ctrl Pts',(-0.209097174476702,0.00750003461914674,
0.0103336083237276));
#44026=CARTESIAN_POINT('Ctrl Pts',(-0.209097013644898,0.00750003454899016,
0.0103400777327138));
#44027=CARTESIAN_POINT('Ctrl Pts',(-0.209096222702432,0.00750003434545369,
0.010346515921967));
#44028=CARTESIAN_POINT('Ctrl Pts',(-0.20909329636813,0.00750003363702495,
0.0103596276713648));
#44029=CARTESIAN_POINT('Ctrl Pts',(-0.209091071837928,0.00750003311269133,
0.0103662450459666));
#44030=CARTESIAN_POINT('Ctrl Pts',(-0.209082819421827,0.00750003116198735,
0.0103842933115514));
#44031=CARTESIAN_POINT('Ctrl Pts',(-0.209075244663783,0.00750002938167454,
0.0103948609074878));
#44032=CARTESIAN_POINT('Ctrl Pts',(-0.209056503078323,0.00750002464315622,
0.0104125535831743));
#44033=CARTESIAN_POINT('Ctrl Pts',(-0.209045509769346,0.00750002191516809,
0.0104195117091797));
#44034=CARTESIAN_POINT('Ctrl Pts',(-0.209021617401814,0.00750001345630346,
0.0104288533084413));
#44035=CARTESIAN_POINT('Ctrl Pts',(-0.209010431787089,0.00750003042004547,
0.0104306206808396));
#44036=CARTESIAN_POINT('Ctrl Pts',(-0.208999076913879,0.00749997330983711,
0.0104311172901319));
#44037=CARTESIAN_POINT('Ctrl Pts',(-0.208996706739788,0.00750001530311512,
0.0104311425771752));
#44038=CARTESIAN_POINT('Ctrl Pts',(-0.208994553969907,0.00750001483683845,
0.0104310940718314));
#44039=CARTESIAN_POINT('Ctrl Pts',(-0.209262779834381,0.0127530221952519,
0.00867490352571389));
#44040=CARTESIAN_POINT('Ctrl Pts',(-0.209261907724246,0.0128139114200784,
0.00876165882827295));
#44041=CARTESIAN_POINT('Ctrl Pts',(-0.209156981788614,0.012820678596178,
0.00874817825753072));
#44042=CARTESIAN_POINT('Ctrl Pts',(-0.209126646748533,0.0119169803293661,
0.00925954195823561));
#44043=CARTESIAN_POINT('Ctrl Pts',(-0.209125531306061,0.0119683694124045,
0.00935303445838102));
#44044=CARTESIAN_POINT('Ctrl Pts',(-0.209020958517736,0.0119791049845719,
0.0093388928112537));
#44045=CARTESIAN_POINT('Ctrl Pts',(-0.208844099307297,0.0100626751446717,
0.0101376946082389));
#44046=CARTESIAN_POINT('Ctrl Pts',(-0.208842582846295,0.0100921812902052,
0.0102414874601498));
#44047=CARTESIAN_POINT('Ctrl Pts',(-0.208735979740018,0.0100913135780991,
0.0102367496736839));
#44048=CARTESIAN_POINT('Ctrl Pts',(-0.209052615735226,0.00800535755099375,
0.0103754827269987));
#44049=CARTESIAN_POINT('Ctrl Pts',(-0.20905100004752,0.00801128846267801,
0.0104819939673908));
#44050=CARTESIAN_POINT('Ctrl Pts',(-0.208945895941917,0.00799967234605693,
0.0104747668175588));
#44051=CARTESIAN_POINT('Ctrl Pts',(-0.209143634222637,0.00698384875614079,
0.0103189178445225));
#44052=CARTESIAN_POINT('Ctrl Pts',(-0.20914203548401,0.00697776519261641,
0.0104247315141036));
#44053=CARTESIAN_POINT('Ctrl Pts',(-0.209036698006323,0.00696916149533664,
0.0104164133964875));
#44054=CARTESIAN_POINT('Ctrl Pts',(-0.209182644409035,0.0122486795278824,
0.00900419949295514));
#44055=CARTESIAN_POINT('Ctrl Pts',(-0.209182521643671,0.0122526095831882,
0.00901058504921382));
#44056=CARTESIAN_POINT('Ctrl Pts',(-0.209181661669861,0.0122572093094837,
0.0090164338194715));
#44057=CARTESIAN_POINT('Ctrl Pts',(-0.209178416135399,0.0122680624431654,
0.00902746434418135));
#44058=CARTESIAN_POINT('Ctrl Pts',(-0.209175915285084,0.012274311695359,
0.00903237634726934));
#44059=CARTESIAN_POINT('Ctrl Pts',(-0.209167710129561,0.0122915844470447,
0.00904299633559153));
#44060=CARTESIAN_POINT('Ctrl Pts',(-0.209160833161763,0.0123034529544618,
0.00904745920985657));
#44061=CARTESIAN_POINT('Ctrl Pts',(-0.209144368242992,0.0123280371679506,
0.00905161116321708));
#44062=CARTESIAN_POINT('Ctrl Pts',(-0.209135335915253,0.0123400083561572,
0.00905130441416833));
#44063=CARTESIAN_POINT('Ctrl Pts',(-0.209112342658012,0.0123677708343673,
0.00904594077689228));
#44064=CARTESIAN_POINT('Ctrl Pts',(-0.209101177031499,0.0123789797724797,
0.00903949015665347));
#44065=CARTESIAN_POINT('Ctrl Pts',(-0.209096245091944,0.0123837538311807,
0.0090367533421206));
#44066=CARTESIAN_POINT('Ctrl Pts',(-0.209094881900175,0.0123853276342592,
0.00903579255933166));
#44067=CARTESIAN_POINT('Ctrl Pts',(-0.209093388609595,0.0123867838297658,
0.00903485559890448));
#44068=CARTESIAN_POINT('Origin',(-0.210345958636625,0.00266466447152654,
0.00897396025668633));
#44069=CARTESIAN_POINT('Ctrl Pts',(-0.210183018258064,0.00274902051429104,
0.00902403655092187));
#44070=CARTESIAN_POINT('Ctrl Pts',(-0.210182986078409,0.00274485631500351,
0.00903062764218945));
#44071=CARTESIAN_POINT('Ctrl Pts',(-0.210183991131823,0.00274000451982491,
0.00903662419786442));
#44072=CARTESIAN_POINT('Ctrl Pts',(-0.210188207874478,0.00272821082078781,
0.00904832417145669));
#44073=CARTESIAN_POINT('Ctrl Pts',(-0.210191733117001,0.00272125100204574,
0.00905354691312546));
#44074=CARTESIAN_POINT('Ctrl Pts',(-0.210202900403688,0.00270289424632346,
0.0090642756442902));
#44075=CARTESIAN_POINT('Ctrl Pts',(-0.210212171803793,0.00269052988924587,
0.0090686500280575));
#44076=CARTESIAN_POINT('Ctrl Pts',(-0.210233488109546,0.00266614464063956,
0.00907233386721743));
#44077=CARTESIAN_POINT('Ctrl Pts',(-0.210244550889318,0.00265491334574057,
0.00907200029364349));
#44078=CARTESIAN_POINT('Ctrl Pts',(-0.210273032995874,0.00262854735965918,
0.00906716900269468));
#44079=CARTESIAN_POINT('Ctrl Pts',(-0.210287082514763,0.00261786366084564,
0.00906121416973908));
#44080=CARTESIAN_POINT('Ctrl Pts',(-0.210291941494424,0.00261427253208097,
0.00905928867009177));
#44081=CARTESIAN_POINT('Ctrl Pts',(-0.210293509512885,0.00261287915022715,
0.00905848296687824));
#44082=CARTESIAN_POINT('Ctrl Pts',(-0.210295198244815,0.0026116162614646,
0.00905772710662984));
#44083=CARTESIAN_POINT('Origin',(-0.209022184336501,0.0123339684657499,
0.00894852096435255));
#44084=CARTESIAN_POINT('Ctrl Pts',(-0.210183435338165,0.0122485460076652,
0.00902552908127326));
#44085=CARTESIAN_POINT('Ctrl Pts',(-0.210183404672864,0.0122525882063418,
0.00903192950713903));
#44086=CARTESIAN_POINT('Ctrl Pts',(-0.210184351646517,0.0122572809704391,
0.00903777213926606));
#44087=CARTESIAN_POINT('Ctrl Pts',(-0.21018833291572,0.0122686650660501,
0.00904921147354004));
#44088=CARTESIAN_POINT('Ctrl Pts',(-0.21019166268256,0.0122753763527015,
0.00905435951685488));
#44089=CARTESIAN_POINT('Ctrl Pts',(-0.210202353382174,0.0122932818182202,
0.00906514542427994));
#44090=CARTESIAN_POINT('Ctrl Pts',(-0.210211334152892,0.0123054392161153,
0.00906965808582159));
#44091=CARTESIAN_POINT('Ctrl Pts',(-0.210232105195764,0.0123295279541306,
0.00907373115597808));
#44092=CARTESIAN_POINT('Ctrl Pts',(-0.210242933631105,0.0123406657908483,
0.0090736130899169));
#44093=CARTESIAN_POINT('Ctrl Pts',(-0.210266698853524,0.0123629818522671,
0.00907000489842172));
#44094=CARTESIAN_POINT('Ctrl Pts',(-0.21027859935186,0.0123728221870957,
0.00906619671479487));
#44095=CARTESIAN_POINT('Ctrl Pts',(-0.21028910046586,0.0123811241479557,
0.00906195160088883));
#44096=CARTESIAN_POINT('Ctrl Pts',(-0.210291801841148,0.0123831802714617,
0.00906087284311615));
#44097=CARTESIAN_POINT('Ctrl Pts',(-0.210294510886685,0.0123851780658678,
0.0090597161082102));
#44098=CARTESIAN_POINT('Ctrl Pts',(-0.210295581644675,0.0123859796838815,
0.00905923666941981));
#44099=CARTESIAN_POINT('Ctrl Pts',(-0.210235728831914,0.00241507780074195,
0.00880998116420352));
#44100=CARTESIAN_POINT('Ctrl Pts',(-0.210234071406577,0.00235904669073682,
0.00889370041917784));
#44101=CARTESIAN_POINT('Ctrl Pts',(-0.210333962911911,0.00236943696297074,
0.00890175177268792));
#44102=CARTESIAN_POINT('Ctrl Pts',(-0.210110088197621,0.00319578551215262,
0.00933201998592346));
#44103=CARTESIAN_POINT('Ctrl Pts',(-0.210108215185178,0.00314830174918374,
0.00942147779615604));
#44104=CARTESIAN_POINT('Ctrl Pts',(-0.210207963690016,0.00316052625529352,
0.00942914090505225));
#44105=CARTESIAN_POINT('Ctrl Pts',(-0.209858705116303,0.00493729344559936,
0.0101400029770193));
#44106=CARTESIAN_POINT('Ctrl Pts',(-0.209856530969995,0.00490918845389919,
0.010238384157586));
#44107=CARTESIAN_POINT('Ctrl Pts',(-0.209957959507333,0.0049101000603546,
0.0102376501196028));
#44108=CARTESIAN_POINT('Ctrl Pts',(-0.210038519626352,0.00685239975317306,
0.0103808740076419));
#44109=CARTESIAN_POINT('Ctrl Pts',(-0.21003621314574,0.00684503735312283,
0.0104818812876138));
#44110=CARTESIAN_POINT('Ctrl Pts',(-0.210136464709093,0.00683510449030559,
0.0104827068374165));
#44111=CARTESIAN_POINT('Ctrl Pts',(-0.210123396348251,0.00779507013823767,
0.0103517138661237));
#44112=CARTESIAN_POINT('Ctrl Pts',(-0.210121102243751,0.00779827092525759,
0.0104523876710869));
#44113=CARTESIAN_POINT('Ctrl Pts',(-0.210221446144753,0.00778939338474545,
0.0104542160251016));
#44114=CARTESIAN_POINT('Ctrl Pts',(-0.210096835005399,0.00750005701517807,
0.0103559762949856));
#44115=CARTESIAN_POINT('Ctrl Pts',(-0.210096687094351,0.00750005694619478,
0.0103625212097521));
#44116=CARTESIAN_POINT('Ctrl Pts',(-0.2100971848396,0.00750005699373978,
0.0103690644157446));
#44117=CARTESIAN_POINT('Ctrl Pts',(-0.21009952881361,0.00750005732184499,
0.0103823685377432));
#44118=CARTESIAN_POINT('Ctrl Pts',(-0.210101452102109,0.00750005761622642,
0.0103890795293896));
#44119=CARTESIAN_POINT('Ctrl Pts',(-0.210108880803097,0.00750005877942611,
0.0104074822535115));
#44120=CARTESIAN_POINT('Ctrl Pts',(-0.210115970621333,0.00750005992136825,
0.0104183813798077));
#44121=CARTESIAN_POINT('Ctrl Pts',(-0.210133894274973,0.00750006265497224,
0.0104369029164948));
#44122=CARTESIAN_POINT('Ctrl Pts',(-0.210144562324342,0.00750006432698296,
0.0104443506765333));
#44123=CARTESIAN_POINT('Ctrl Pts',(-0.210166482013843,0.0075000664469057,
0.0104540843436323));
#44124=CARTESIAN_POINT('Ctrl Pts',(-0.210177278956079,0.00750008423230304,
0.0104568718346631));
#44125=CARTESIAN_POINT('Ctrl Pts',(-0.210190486034838,0.00750005044434054,
0.0104580479112367));
#44126=CARTESIAN_POINT('Ctrl Pts',(-0.210192746853844,0.0075000750390866,
0.0104581738820239));
#44127=CARTESIAN_POINT('Ctrl Pts',(-0.210194951359283,0.00750007548126885,
0.0104582237389144));
#44128=CARTESIAN_POINT('Ctrl Pts',(-0.210122793732566,0.0072130985215446,
0.0103519917672711));
#44129=CARTESIAN_POINT('Ctrl Pts',(-0.210120511886917,0.00720999322852045,
0.0104525810605786));
#44130=CARTESIAN_POINT('Ctrl Pts',(-0.210220762860161,0.00721890481119139,
0.0104544782767662));
#44131=CARTESIAN_POINT('Ctrl Pts',(-0.210037720781374,0.00815258917703958,
0.0103800527152135));
#44132=CARTESIAN_POINT('Ctrl Pts',(-0.210035427035482,0.00816000131863083,
0.0104809628804394));
#44133=CARTESIAN_POINT('Ctrl Pts',(-0.210135589792883,0.00816995626869976,
0.0104818539938396));
#44134=CARTESIAN_POINT('Ctrl Pts',(-0.209859677707026,0.0100577432524158,
0.0101407613056068));
#44135=CARTESIAN_POINT('Ctrl Pts',(-0.209857515480827,0.0100857673151341,
0.0102390654985703));
#44136=CARTESIAN_POINT('Ctrl Pts',(-0.209958847930015,0.01008472544421,
0.0102384646295444));
#44137=CARTESIAN_POINT('Ctrl Pts',(-0.210110429917104,0.0117990274139096,
0.00933430221347137));
#44138=CARTESIAN_POINT('Ctrl Pts',(-0.210108568093871,0.0118464108462543,
0.00942370750730259));
#44139=CARTESIAN_POINT('Ctrl Pts',(-0.210208238820813,0.0118343155306104,
0.00943138597517952));
#44140=CARTESIAN_POINT('Ctrl Pts',(-0.210234836619464,0.0125753775929816,
0.00881634681983917));
#44141=CARTESIAN_POINT('Ctrl Pts',(-0.210233188506976,0.012631254401039,
0.00890006330818432));
#44142=CARTESIAN_POINT('Ctrl Pts',(-0.210332995760394,0.0126209274539493,
0.00890814505908907));
#44143=CARTESIAN_POINT('Ctrl Pts',(-0.193150248578096,0.002155718567371,
0.00842869397060042));
#44144=CARTESIAN_POINT('Ctrl Pts',(-0.193256283550229,0.00216190824138389,
0.00844307130174834));
#44145=CARTESIAN_POINT('Ctrl Pts',(-0.193257164103685,0.00222199064266424,
0.00835431756888208));
#44146=CARTESIAN_POINT('Ctrl Pts',(-0.193012984040365,0.00300714201445438,
0.00900503485649586));
#44147=CARTESIAN_POINT('Ctrl Pts',(-0.193118665659607,0.00301772975659131,
0.0090202174587487));
#44148=CARTESIAN_POINT('Ctrl Pts',(-0.193119801031167,0.0030683347568226,
0.00892498937300423));
#44149=CARTESIAN_POINT('Ctrl Pts',(-0.192745011683614,0.00490686685772646,
0.0098801636284191));
#44150=CARTESIAN_POINT('Ctrl Pts',(-0.192852683475637,0.00490403518209803,
0.00988585649881339));
#44151=CARTESIAN_POINT('Ctrl Pts',(-0.192854234568138,0.00493309436623873,
0.00978079682132178));
#44152=CARTESIAN_POINT('Ctrl Pts',(-0.192955683255973,0.00699520299814787,
0.010111749605735));
#44153=CARTESIAN_POINT('Ctrl Pts',(-0.193061924225102,0.00698430847540474,
0.0101203996272913));
#44154=CARTESIAN_POINT('Ctrl Pts',(-0.193063578454204,0.00699016812253032,
0.0100127282934439));
#44155=CARTESIAN_POINT('Ctrl Pts',(-0.193039146112862,0.00802792285482773,
0.0100554658624458));
#44156=CARTESIAN_POINT('Ctrl Pts',(-0.193145610777312,0.00801970468892787,
0.0100650060203432));
#44157=CARTESIAN_POINT('Ctrl Pts',(-0.193147246517876,0.00801377089926689,
0.00995799710993926));
#44158=CARTESIAN_POINT('Ctrl Pts',(-0.193087906597634,0.00259433621160271,
0.00870850400383643));
#44159=CARTESIAN_POINT('Ctrl Pts',(-0.193088660379233,0.00259507710819496,
0.00870896461926417));
#44160=CARTESIAN_POINT('Ctrl Pts',(-0.193090838197641,0.00259716508697917,
0.00871022994405992));
#44161=CARTESIAN_POINT('Ctrl Pts',(-0.193093007507657,0.00259931370221831,
0.00871140548417046));
#44162=CARTESIAN_POINT('Ctrl Pts',(-0.193099786390759,0.00260636033187971,
0.00871517111274946));
#44163=CARTESIAN_POINT('Ctrl Pts',(-0.193109374534362,0.00261646326772918,
0.00871977795304027));
#44164=CARTESIAN_POINT('Ctrl Pts',(-0.193129347090727,0.00264061390658031,
0.0087240933815241));
#44165=CARTESIAN_POINT('Ctrl Pts',(-0.193137930238211,0.00265191377293256,
0.00872431831244535));
#44166=CARTESIAN_POINT('Ctrl Pts',(-0.193154323635676,0.00267595556989629,
0.00872040298226909));
#44167=CARTESIAN_POINT('Ctrl Pts',(-0.19316144921592,0.00268796736359503,
0.00871594058854767));
#44168=CARTESIAN_POINT('Ctrl Pts',(-0.193170103619306,0.00270560796812055,
0.00870514470897271));
#44169=CARTESIAN_POINT('Ctrl Pts',(-0.193172791808667,0.00271208445690734,
0.00870003504614985));
#44170=CARTESIAN_POINT('Ctrl Pts',(-0.193176272919966,0.00272326292681188,
0.00868851352183221));
#44171=CARTESIAN_POINT('Ctrl Pts',(-0.193177193207206,0.00272796362356798,
0.0086824011184089));
#44172=CARTESIAN_POINT('Ctrl Pts',(-0.193177319394213,0.00273193776376147,
0.00867571960454275));
#44173=CARTESIAN_POINT('Ctrl Pts',(-0.193103854794884,0.00749669679535383,
0.00997223701970883));
#44174=CARTESIAN_POINT('Ctrl Pts',(-0.193103688879779,0.00749669454298784,
0.00997867376305629));
#44175=CARTESIAN_POINT('Ctrl Pts',(-0.193102899462808,0.00749669250460742,
0.00998507923961693));
#44176=CARTESIAN_POINT('Ctrl Pts',(-0.193099982508425,0.00749668876680328,
0.00999815748298232));
#44177=CARTESIAN_POINT('Ctrl Pts',(-0.193097760138914,0.00749668711867432,
0.0100047731041968));
#44178=CARTESIAN_POINT('Ctrl Pts',(-0.193089514503717,0.00749668333127773,
0.0100228195151261));
#44179=CARTESIAN_POINT('Ctrl Pts',(-0.193081944631272,0.00749668200346064,
0.01003338801341));
#44180=CARTESIAN_POINT('Ctrl Pts',(-0.193063213341713,0.00749668173385395,
0.0100510828898264));
#44181=CARTESIAN_POINT('Ctrl Pts',(-0.193052225711713,0.00749668280519559,
0.0100580427360768));
#44182=CARTESIAN_POINT('Ctrl Pts',(-0.19302027734347,0.00749668852449542,
0.010070544244531));
#44183=CARTESIAN_POINT('Ctrl Pts',(-0.193003720397325,0.00749672313589827,
0.0100696729208636));
#44184=CARTESIAN_POINT('Ctrl Pts',(-0.193001721429014,0.00749667300664829,
0.0100696409746475));
#44185=CARTESIAN_POINT('Ctrl Pts',(-0.193001278631462,0.00749669549250376,
0.0100696317309843));
#44186=CARTESIAN_POINT('Ctrl Pts',(-0.193258116673284,0.0127748021146355,
0.00835637632548243));
#44187=CARTESIAN_POINT('Ctrl Pts',(-0.19325734733193,0.0128347753589733,
0.0084450700687607));
#44188=CARTESIAN_POINT('Ctrl Pts',(-0.1931513946487,0.0128410248114817,
0.00843094236671849));
#44189=CARTESIAN_POINT('Ctrl Pts',(-0.193121943698077,0.0119278082044051,
0.00892703216180217));
#44190=CARTESIAN_POINT('Ctrl Pts',(-0.193120919356265,0.011978301925409,
0.00902219357317199));
#44191=CARTESIAN_POINT('Ctrl Pts',(-0.193015313553372,0.0119888536363698,
0.00900729145699337));
#44192=CARTESIAN_POINT('Ctrl Pts',(-0.192856751458538,0.0100615008924823,
0.00978240230173624));
#44193=CARTESIAN_POINT('Ctrl Pts',(-0.192855314176916,0.0100904700801754,
0.00988737015200106));
#44194=CARTESIAN_POINT('Ctrl Pts',(-0.192747750734788,0.0100879112589918,
0.0098818218088034));
#44195=CARTESIAN_POINT('Ctrl Pts',(-0.193063722049803,0.00800347256964883,
0.010013024834604));
#44196=CARTESIAN_POINT('Ctrl Pts',(-0.193062180924944,0.00800926363390783,
0.0101205895545703));
#44197=CARTESIAN_POINT('Ctrl Pts',(-0.192956023165166,0.00799844202683973,
0.0101121707024309));
#44198=CARTESIAN_POINT('Ctrl Pts',(-0.193146983637435,0.00697937055318562,
0.00995750654052233));
#44199=CARTESIAN_POINT('Ctrl Pts',(-0.193145461549892,0.00697337420362424,
0.0100644016451243));
#44200=CARTESIAN_POINT('Ctrl Pts',(-0.193039084458002,0.00696523223500842,
0.0100550890613376));
#44201=CARTESIAN_POINT('Ctrl Pts',(-0.193178854938834,0.0122644745065787,
0.00867785711110863));
#44202=CARTESIAN_POINT('Ctrl Pts',(-0.193178732684009,0.0122683134690069,
0.00868431988905915));
#44203=CARTESIAN_POINT('Ctrl Pts',(-0.193177867248174,0.0122728334582095,
0.00869025340848932));
#44204=CARTESIAN_POINT('Ctrl Pts',(-0.193174598785043,0.0122835448345936,
0.0087014760988186));
#44205=CARTESIAN_POINT('Ctrl Pts',(-0.193172079221637,0.0122897359511657,
0.00870649292851449));
#44206=CARTESIAN_POINT('Ctrl Pts',(-0.193163823813424,0.0123068720960452,
0.00871737792668749));
#44207=CARTESIAN_POINT('Ctrl Pts',(-0.193156912387403,0.0123186810332227,
0.0087220158449302));
#44208=CARTESIAN_POINT('Ctrl Pts',(-0.193140066915631,0.0123436664345626,
0.00872660846703081));
#44209=CARTESIAN_POINT('Ctrl Pts',(-0.193130622805463,0.0123560881528755,
0.00872637846084337));
#44210=CARTESIAN_POINT('Ctrl Pts',(-0.193106574731809,0.0123848966283851,
0.00872085579898184));
#44211=CARTESIAN_POINT('Ctrl Pts',(-0.193094959201527,0.0123966062123334,
0.00871393611643193));
#44212=CARTESIAN_POINT('Ctrl Pts',(-0.193091121761129,0.0123999085096778,
0.00871200439517824));
#44213=CARTESIAN_POINT('Ctrl Pts',(-0.193090627838197,0.0124005744669603,
0.00871160617095989));
#44214=CARTESIAN_POINT('Ctrl Pts',(-0.19308996299534,0.0124014666379723,
0.00871106882775808));
#44215=CARTESIAN_POINT('Ctrl Pts',(-0.193089364511003,0.0124020544162197,
0.00871070376520487));
#44216=CARTESIAN_POINT('Origin',(-0.194340687084312,0.00264715365052573,
0.00864799567634145));
#44217=CARTESIAN_POINT('Ctrl Pts',(-0.194177759801894,0.00273230901719225,
0.00869689124250935));
#44218=CARTESIAN_POINT('Ctrl Pts',(-0.194177734563329,0.00272825679049417,
0.0087035201702409));
#44219=CARTESIAN_POINT('Ctrl Pts',(-0.194178737007743,0.00272351230975779,
0.0087095688792266));
#44220=CARTESIAN_POINT('Ctrl Pts',(-0.194182937678093,0.00271191998453251,
0.00872142829908946));
#44221=CARTESIAN_POINT('Ctrl Pts',(-0.194186453742996,0.00270504337667792,
0.00872675563944484));
#44222=CARTESIAN_POINT('Ctrl Pts',(-0.194197594088965,0.00268685648376357,
0.00873776163623637));
#44223=CARTESIAN_POINT('Ctrl Pts',(-0.194206842940504,0.00267456231482886,
0.00874232351067159));
#44224=CARTESIAN_POINT('Ctrl Pts',(-0.19422845325808,0.00264984454257071,
0.00874644507296066));
#44225=CARTESIAN_POINT('Ctrl Pts',(-0.194239902406931,0.00263823421510073,
0.00874620622855402));
#44226=CARTESIAN_POINT('Ctrl Pts',(-0.194268856357757,0.00261146863134927,
0.00874142573297465));
#44227=CARTESIAN_POINT('Ctrl Pts',(-0.194282924857919,0.00260056732491295,
0.00873542278756813));
#44228=CARTESIAN_POINT('Ctrl Pts',(-0.194287483390899,0.0025974904442716,
0.00873376963576102));
#44229=CARTESIAN_POINT('Ctrl Pts',(-0.194288131908502,0.00259685179335783,
0.00873340705306226));
#44230=CARTESIAN_POINT('Ctrl Pts',(-0.194289003765303,0.00259599649080464,
0.00873291853305801));
#44231=CARTESIAN_POINT('Ctrl Pts',(-0.194289738575767,0.00259544077467718,
0.00873259744100971));
#44232=CARTESIAN_POINT('Origin',(-0.193016773520565,0.0123506084835679,
0.00862353297935073));
#44233=CARTESIAN_POINT('Ctrl Pts',(-0.194178213525151,0.0122641753917418,
0.00869897007119024));
#44234=CARTESIAN_POINT('Ctrl Pts',(-0.19417818900797,0.0122681099513547,
0.00870541070607376));
#44235=CARTESIAN_POINT('Ctrl Pts',(-0.194179133897106,0.0122726998135444,
0.00871130683949189));
#44236=CARTESIAN_POINT('Ctrl Pts',(-0.194183101697783,0.0122838897135974,
0.00872290434119992));
#44237=CARTESIAN_POINT('Ctrl Pts',(-0.194186423814274,0.0122905196648154,
0.00872815483354177));
#44238=CARTESIAN_POINT('Ctrl Pts',(-0.194197091348588,0.0123082547642953,
0.00873921387701456));
#44239=CARTESIAN_POINT('Ctrl Pts',(-0.194206051681268,0.012320338923391,
0.00874391202827635));
#44240=CARTESIAN_POINT('Ctrl Pts',(-0.194226779022762,0.0123443606653273,
0.00874835472895947));
#44241=CARTESIAN_POINT('Ctrl Pts',(-0.194237586866862,0.0123555001763983,
0.00874840789326625));
#44242=CARTESIAN_POINT('Ctrl Pts',(-0.194262383165019,0.012378886469752,
0.00874499443907016));
#44243=CARTESIAN_POINT('Ctrl Pts',(-0.19427464652378,0.012388931904822,
0.00874091634599449));
#44244=CARTESIAN_POINT('Ctrl Pts',(-0.19428359687381,0.012396093564287,
0.00873739094093589));
#44245=CARTESIAN_POINT('Ctrl Pts',(-0.194286369122631,0.0123982203159595,
0.00873632096909965));
#44246=CARTESIAN_POINT('Ctrl Pts',(-0.194289147403157,0.0124002824398107,
0.0087351659660157));
#44247=CARTESIAN_POINT('Ctrl Pts',(-0.194290139287956,0.0124010331447966,
0.00873473267146801));
#44248=CARTESIAN_POINT('Ctrl Pts',(-0.194260506267582,0.00220572340070951,
0.00836167384219302));
#44249=CARTESIAN_POINT('Ctrl Pts',(-0.194258100970628,0.00214777522781843,
0.00844667263238102));
#44250=CARTESIAN_POINT('Ctrl Pts',(-0.194360207871775,0.00215850129660316,
0.00845346577350011));
#44251=CARTESIAN_POINT('Ctrl Pts',(-0.194124326267857,0.00304288389765983,
0.00893183123041262));
#44252=CARTESIAN_POINT('Ctrl Pts',(-0.19412167047553,0.00299397998963251,
0.00902304578615173));
#44253=CARTESIAN_POINT('Ctrl Pts',(-0.194223439496858,0.0030082858629339,
0.00903013800120372));
#44254=CARTESIAN_POINT('Ctrl Pts',(-0.193851172469893,0.00493055345358367,
0.00980700548405018));
#44255=CARTESIAN_POINT('Ctrl Pts',(-0.193848146793342,0.00490256758354324,
0.00990786728226616));
#44256=CARTESIAN_POINT('Ctrl Pts',(-0.193951850968722,0.00490228471229653,
0.00990506238773098));
#44257=CARTESIAN_POINT('Ctrl Pts',(-0.19406447559344,0.007002084092692,
0.0100356201917367));
#44258=CARTESIAN_POINT('Ctrl Pts',(-0.194061323729412,0.00699650921242796,
0.0101389487716742));
#44259=CARTESIAN_POINT('Ctrl Pts',(-0.194163683898811,0.00698641223011458,
0.0101386734868917));
#44260=CARTESIAN_POINT('Ctrl Pts',(-0.194147067815913,0.00802012051698481,
0.00998010568044098));
#44261=CARTESIAN_POINT('Ctrl Pts',(-0.194143940209193,0.00802585838081097,
0.0100828035425696));
#44262=CARTESIAN_POINT('Ctrl Pts',(-0.194246522734699,0.00801753202529335,
0.0100834664650456));
#44263=CARTESIAN_POINT('Ctrl Pts',(-0.194103277573009,0.00749642324651037,
0.00999450835808371));
#44264=CARTESIAN_POINT('Ctrl Pts',(-0.194103129691022,0.00749642071073177,
0.0100010516868068));
#44265=CARTESIAN_POINT('Ctrl Pts',(-0.19410362684754,0.00749641796588605,
0.0100075933642326));
#44266=CARTESIAN_POINT('Ctrl Pts',(-0.194105968382486,0.00749641195276905,
0.0100208942631091));
#44267=CARTESIAN_POINT('Ctrl Pts',(-0.194107889712825,0.00749640867914678,
0.0100276037389201));
#44268=CARTESIAN_POINT('Ctrl Pts',(-0.194115311897938,0.00749639900304797,
0.0100460043878287));
#44269=CARTESIAN_POINT('Ctrl Pts',(-0.194122396681178,0.00749639239915879,
0.0100569040309536));
#44270=CARTESIAN_POINT('Ctrl Pts',(-0.194140309556159,0.00749637928051436,
0.0100754268638114));
#44271=CARTESIAN_POINT('Ctrl Pts',(-0.19415097154416,0.00749637288296616,
0.0100828758665553));
#44272=CARTESIAN_POINT('Ctrl Pts',(-0.1941746012313,0.0074963611503292,
0.0100933764134099));
#44273=CARTESIAN_POINT('Ctrl Pts',(-0.194187727972084,0.00749618054610755,
0.0100963596764324));
#44274=CARTESIAN_POINT('Ctrl Pts',(-0.194200910015988,0.00749636354091595,
0.0100967435529685));
#44275=CARTESIAN_POINT('Ctrl Pts',(-0.194201347570367,0.00749635091189165,
0.0100967541477686));
#44276=CARTESIAN_POINT('Ctrl Pts',(-0.194360528299949,0.0128383615463125,
0.00845560308938517));
#44277=CARTESIAN_POINT('Ctrl Pts',(-0.194258272737925,0.0128491304722729,
0.00844891950105934));
#44278=CARTESIAN_POINT('Ctrl Pts',(-0.194260717158237,0.0127911313733274,
0.00836378093723286));
#44279=CARTESIAN_POINT('Ctrl Pts',(-0.194224114589826,0.0119877834030537,
0.00903232837929657));
#44280=CARTESIAN_POINT('Ctrl Pts',(-0.194122194143984,0.012002116243167,
0.00902535590699909));
#44281=CARTESIAN_POINT('Ctrl Pts',(-0.194124889316599,0.01195318233319,
0.00893399239655918));
#44282=CARTESIAN_POINT('Ctrl Pts',(-0.193953516481441,0.0100921752283048,
0.00990683661153991));
#44283=CARTESIAN_POINT('Ctrl Pts',(-0.193849673625334,0.0100919068339616,
0.0099097432667668));
#44284=CARTESIAN_POINT('Ctrl Pts',(-0.19385274022071,0.0100639398252907,
0.00980872003459304));
#44285=CARTESIAN_POINT('Ctrl Pts',(-0.194164107388867,0.0080066176885033,
0.0101391372864121));
#44286=CARTESIAN_POINT('Ctrl Pts',(-0.194061595152703,0.00799659454517679,
0.0101395100125378));
#44287=CARTESIAN_POINT('Ctrl Pts',(-0.19406478636751,0.00799109269338365,
0.0100360321855207));
#44288=CARTESIAN_POINT('Ctrl Pts',(-0.194246313132581,0.00697484113490648,
0.0100830349322283));
#44289=CARTESIAN_POINT('Ctrl Pts',(-0.194143580799908,0.00696655979783964,
0.0100824785919351));
#44290=CARTESIAN_POINT('Ctrl Pts',(-0.194146747597959,0.00697239106197278,
0.00997964182851975));
#44291=CARTESIAN_POINT('Ctrl Pts',(-0.21314244217965,0.00800704485816821,
0.0104100735882361));
#44292=CARTESIAN_POINT('Ctrl Pts',(-0.213140557332318,0.00801304626172808,
0.010515107812128));
#44293=CARTESIAN_POINT('Ctrl Pts',(-0.213035975570542,0.00802176781725835,
0.0105073159363579));
#44294=CARTESIAN_POINT('Ctrl Pts',(-0.213049378421211,0.00698785896905304,
0.0104654522252342));
#44295=CARTESIAN_POINT('Ctrl Pts',(-0.213047478135136,0.00698188315917987,
0.0105711732503626));
#44296=CARTESIAN_POINT('Ctrl Pts',(-0.212943125098063,0.00699360586976436,
0.0105645191388941));
#44297=CARTESIAN_POINT('Ctrl Pts',(-0.21284235286589,0.00493765989046783,
0.0102271645351171));
#44298=CARTESIAN_POINT('Ctrl Pts',(-0.212840545854496,0.00490818586219254,
0.0103301719884767));
#44299=CARTESIAN_POINT('Ctrl Pts',(-0.212734689125797,0.00490851668823669,
0.0103258556199139));
#44300=CARTESIAN_POINT('Ctrl Pts',(-0.213128996239289,0.00308108542687099,
0.00934123157192873));
#44301=CARTESIAN_POINT('Ctrl Pts',(-0.213127591971784,0.00302966984888558,
0.00943382096925474));
#44302=CARTESIAN_POINT('Ctrl Pts',(-0.213023759867318,0.0030188772658784,
0.00942016390252589));
#44303=CARTESIAN_POINT('Ctrl Pts',(-0.213264189117079,0.00225085884863554,
0.00875478600723178));
#44304=CARTESIAN_POINT('Ctrl Pts',(-0.213263022759027,0.00219003479095467,
0.00884062777732394));
#44305=CARTESIAN_POINT('Ctrl Pts',(-0.21315884015455,0.00218306511806226,
0.00882758561253449));
#44306=CARTESIAN_POINT('Ctrl Pts',(-0.21309502125729,0.00261465160980138,
0.00911535617230443));
#44307=CARTESIAN_POINT('Ctrl Pts',(-0.213095852147055,0.00261546012528567,
0.00911588091549215));
#44308=CARTESIAN_POINT('Ctrl Pts',(-0.213097944988729,0.00261745919854445,
0.00911714133440077));
#44309=CARTESIAN_POINT('Ctrl Pts',(-0.213100030401507,0.00261951332673603,
0.00911832279138069));
#44310=CARTESIAN_POINT('Ctrl Pts',(-0.213107399960229,0.00262708280290663,
0.00912255754016195));
#44311=CARTESIAN_POINT('Ctrl Pts',(-0.213116909534435,0.00263712569580249,
0.00912717772590095));
#44312=CARTESIAN_POINT('Ctrl Pts',(-0.213136390591303,0.00266064930220927,
0.00913185073406218));
#44313=CARTESIAN_POINT('Ctrl Pts',(-0.213144957944981,0.00267194878783946,
0.00913229266932233));
#44314=CARTESIAN_POINT('Ctrl Pts',(-0.213161315291064,0.00269606564430115,
0.00912883668359065));
#44315=CARTESIAN_POINT('Ctrl Pts',(-0.213168423636603,0.00270815996238018,
0.00912460454553612));
#44316=CARTESIAN_POINT('Ctrl Pts',(-0.213177057657863,0.00272600171322136,
0.00911414773088799));
#44317=CARTESIAN_POINT('Ctrl Pts',(-0.213179739287994,0.00273257276596848,
0.0091091633924076));
#44318=CARTESIAN_POINT('Ctrl Pts',(-0.213183213079011,0.00274396560695684,
0.0090978602830844));
#44319=CARTESIAN_POINT('Ctrl Pts',(-0.213184132100665,0.00274878070299104,
0.00909184013117857));
#44320=CARTESIAN_POINT('Ctrl Pts',(-0.213184259448588,0.00275288038367511,
0.00908523762214338));
#44321=CARTESIAN_POINT('Ctrl Pts',(-0.213095881749409,0.00749981308898754,
0.0104239596527637));
#44322=CARTESIAN_POINT('Ctrl Pts',(-0.213095722179992,0.00749981285121825,
0.010430437431427));
#44323=CARTESIAN_POINT('Ctrl Pts',(-0.213094930767734,0.00749981251703481,
0.0104368839919119));
#44324=CARTESIAN_POINT('Ctrl Pts',(-0.213092001729469,0.00749981161579216,
0.0104500045880059));
#44325=CARTESIAN_POINT('Ctrl Pts',(-0.213089776365308,0.00749981103605203,
0.0104566226524584));
#44326=CARTESIAN_POINT('Ctrl Pts',(-0.213081521344629,0.00749980905034941,
0.010474671634648));
#44327=CARTESIAN_POINT('Ctrl Pts',(-0.213073944722568,0.00749980739807012,
0.0104852388781492));
#44328=CARTESIAN_POINT('Ctrl Pts',(-0.213055199228367,0.00749980314047178,
0.0105029306783858));
#44329=CARTESIAN_POINT('Ctrl Pts',(-0.213044203777357,0.00749980079481611,
0.0105098881281539));
#44330=CARTESIAN_POINT('Ctrl Pts',(-0.213021129873168,0.00749979313590021,
0.0105189069191168));
#44331=CARTESIAN_POINT('Ctrl Pts',(-0.213010238547216,0.00749982047260193,
0.0105209461160442));
#44332=CARTESIAN_POINT('Ctrl Pts',(-0.212998855188053,0.0074997539260879,
0.0105214434901032));
#44333=CARTESIAN_POINT('Ctrl Pts',(-0.21299658018429,0.00749977253963051,
0.0105215078747055));
#44334=CARTESIAN_POINT('Ctrl Pts',(-0.212994304312368,0.00749979722059817,
0.0105214917573229));
#44335=CARTESIAN_POINT('Ctrl Pts',(-0.212993242078276,0.00749979705225721,
0.0105214677966727));
#44336=CARTESIAN_POINT('Ctrl Pts',(-0.213265643152316,0.0127494169330871,
0.0087544692044563));
#44337=CARTESIAN_POINT('Ctrl Pts',(-0.21326473253461,0.0128101841803463,
0.00884027806311097));
#44338=CARTESIAN_POINT('Ctrl Pts',(-0.213160591305935,0.0128173325297111,
0.00882751233582958));
#44339=CARTESIAN_POINT('Ctrl Pts',(-0.213130471882447,0.0119156035997271,
0.00934279777846922));
#44340=CARTESIAN_POINT('Ctrl Pts',(-0.213129321865349,0.0119669179384452,
0.0094353728123257));
#44341=CARTESIAN_POINT('Ctrl Pts',(-0.213025528705725,0.0119777956790885,
0.00942203256996151));
#44342=CARTESIAN_POINT('Ctrl Pts',(-0.212843201419264,0.010063046280529,
0.010226865697998));
#44343=CARTESIAN_POINT('Ctrl Pts',(-0.212841654709403,0.0100925082785676,
0.0103298072401898));
#44344=CARTESIAN_POINT('Ctrl Pts',(-0.212735841572136,0.0100925267904534,
0.0103257419102505));
#44345=CARTESIAN_POINT('Ctrl Pts',(-0.21304944510932,0.00800490895468439,
0.0104661698013438));
#44346=CARTESIAN_POINT('Ctrl Pts',(-0.213047801242471,0.00801082470959272,
0.0105718409234886));
#44347=CARTESIAN_POINT('Ctrl Pts',(-0.212943497366402,0.0079990046369987,
0.0105655221405287));
#44348=CARTESIAN_POINT('Ctrl Pts',(-0.213143562589862,0.00698374221754044,
0.0104092444559369));
#44349=CARTESIAN_POINT('Ctrl Pts',(-0.213141935136846,0.006977658566979,
0.0105142134722975));
#44350=CARTESIAN_POINT('Ctrl Pts',(-0.213037396541874,0.00696892923864034,
0.0105067288521001));
#44351=CARTESIAN_POINT('Ctrl Pts',(-0.213185728279609,0.0122462777113575,
0.0090857895003052));
#44352=CARTESIAN_POINT('Ctrl Pts',(-0.213185605522206,0.0122502256407507,
0.00909215008990704));
#44353=CARTESIAN_POINT('Ctrl Pts',(-0.213184747944004,0.0122548388876003,
0.00909797344983545));
#44354=CARTESIAN_POINT('Ctrl Pts',(-0.213181512007441,0.0122657110834179,
0.00910894984843468));
#44355=CARTESIAN_POINT('Ctrl Pts',(-0.213179018878935,0.0122719649390347,
0.00911383454991018));
#44356=CARTESIAN_POINT('Ctrl Pts',(-0.213170832096408,0.0122892521858956,
0.00912439517024284));
#44357=CARTESIAN_POINT('Ctrl Pts',(-0.213163965267044,0.0123011258937518,
0.00912882261041887));
#44358=CARTESIAN_POINT('Ctrl Pts',(-0.213147672649622,0.0123254768658068,
0.00913286791781534));
#44359=CARTESIAN_POINT('Ctrl Pts',(-0.213138835653607,0.0123372160682492,
0.00913257902200331));
#44360=CARTESIAN_POINT('Ctrl Pts',(-0.213117808936497,0.01236268389567,
0.00912776054568632));
#44361=CARTESIAN_POINT('Ctrl Pts',(-0.213107738955393,0.0123731866485371,
0.00912252033124069));
#44362=CARTESIAN_POINT('Ctrl Pts',(-0.213101344146465,0.0123795035575569,
0.00911897238156799));
#44363=CARTESIAN_POINT('Ctrl Pts',(-0.213099219437922,0.0123817001155079,
0.00911770584894932));
#44364=CARTESIAN_POINT('Ctrl Pts',(-0.213097102033634,0.0123838455880542,
0.00911634252929533));
#44365=CARTESIAN_POINT('Ctrl Pts',(-0.21309647053259,0.012384459580252,
0.0091159441211624));
#44366=CARTESIAN_POINT('Origin',(-0.214347662483129,0.00266871923262899,
0.00905620843311971));
#44367=CARTESIAN_POINT('Ctrl Pts',(-0.214184739127859,0.00275296418162114,
0.00910660044517797));
#44368=CARTESIAN_POINT('Ctrl Pts',(-0.214184705167232,0.00274877407735516,
0.00911318294739935));
#44369=CARTESIAN_POINT('Ctrl Pts',(-0.214185710281598,0.0027438969349025,
0.00911916725721471));
#44370=CARTESIAN_POINT('Ctrl Pts',(-0.214189928699547,0.00273205492134834,
0.00913082903422289));
#44371=CARTESIAN_POINT('Ctrl Pts',(-0.214193454323423,0.00272507453530064,
0.0091360264580834));
#44372=CARTESIAN_POINT('Ctrl Pts',(-0.214204622414102,0.00270667397370094,
0.00914668775089928));
#44373=CARTESIAN_POINT('Ctrl Pts',(-0.214213894585907,0.00269428945700686,
0.00915101610138924));
#44374=CARTESIAN_POINT('Ctrl Pts',(-0.214234997941506,0.00267012597954294,
0.0091545717540337));
#44375=CARTESIAN_POINT('Ctrl Pts',(-0.214245806144954,0.00265912295208112,
0.00915424567834094));
#44376=CARTESIAN_POINT('Ctrl Pts',(-0.214271986514769,0.00263479199100398,
0.00914986381913527));
#44377=CARTESIAN_POINT('Ctrl Pts',(-0.214284570577821,0.00262485942138193,
0.00914497748979659));
#44378=CARTESIAN_POINT('Ctrl Pts',(-0.214290934974484,0.00262004427343166,
0.00914244557852087));
#44379=CARTESIAN_POINT('Ctrl Pts',(-0.214293725152539,0.00261783324017151,
0.00914125976115354));
#44380=CARTESIAN_POINT('Ctrl Pts',(-0.214296516354532,0.00261568157392703,
0.00913997117675835));
#44381=CARTESIAN_POINT('Ctrl Pts',(-0.214296908994206,0.00261538838033364,
0.00913979427543505));
#44382=CARTESIAN_POINT('Origin',(-0.213025165970707,0.0123312822178751,
0.0090298267726731));
#44383=CARTESIAN_POINT('Ctrl Pts',(-0.214186464570385,0.0122466727702326,
0.00910686109075036));
#44384=CARTESIAN_POINT('Ctrl Pts',(-0.214186432446519,0.0122507411748032,
0.00911325092952807));
#44385=CARTESIAN_POINT('Ctrl Pts',(-0.214187379505248,0.012255459315398,
0.00911907945239577));
#44386=CARTESIAN_POINT('Ctrl Pts',(-0.214191362266413,0.0122668921338603,
0.00913047768807081));
#44387=CARTESIAN_POINT('Ctrl Pts',(-0.214194692444062,0.0122736244775929,
0.00913559918392179));
#44388=CARTESIAN_POINT('Ctrl Pts',(-0.214205384205187,0.0122915757188726,
0.00914631422887851));
#44389=CARTESIAN_POINT('Ctrl Pts',(-0.214214366271417,0.0123037547460295,
0.00915077847840976));
#44390=CARTESIAN_POINT('Ctrl Pts',(-0.21423513972337,0.0123278689671253,
0.00915475462039644));
#44391=CARTESIAN_POINT('Ctrl Pts',(-0.214245969070987,0.0123390113447535,
0.00915459131747644));
#44392=CARTESIAN_POINT('Ctrl Pts',(-0.214269715947045,0.012361305516168,
0.00915089521639169));
#44393=CARTESIAN_POINT('Ctrl Pts',(-0.214281568601509,0.0123711055205838,
0.00914706836117744));
#44394=CARTESIAN_POINT('Ctrl Pts',(-0.214292171730787,0.0123794661551032,
0.0091427537421371));
#44395=CARTESIAN_POINT('Ctrl Pts',(-0.214294839359734,0.0123814960193334,
0.00914167679027904));
#44396=CARTESIAN_POINT('Ctrl Pts',(-0.21429751482476,0.0123834705158705,
0.00914052487394618));
#44397=CARTESIAN_POINT('Ctrl Pts',(-0.214298620129385,0.012384296620628,
0.00914002647745522));
#44398=CARTESIAN_POINT('Ctrl Pts',(-0.214216754079608,0.00254864162832996,
0.00897659909113701));
#44399=CARTESIAN_POINT('Ctrl Pts',(-0.214215071756275,0.00249383408308367,
0.00906087149037426));
#44400=CARTESIAN_POINT('Ctrl Pts',(-0.214314737987371,0.00250427417561616,
0.00906900710735247));
#44401=CARTESIAN_POINT('Ctrl Pts',(-0.214098711059485,0.00329387750221925,
0.00946040117636586));
#44402=CARTESIAN_POINT('Ctrl Pts',(-0.214096831881102,0.00324728810829633,
0.00955002047493883));
#44403=CARTESIAN_POINT('Ctrl Pts',(-0.214196461482836,0.00325869649582198,
0.00955741154943173));
#44404=CARTESIAN_POINT('Ctrl Pts',(-0.213868831622076,0.00494124278014463,
0.0102135400153998));
#44405=CARTESIAN_POINT('Ctrl Pts',(-0.213866675848953,0.0049130570953545,
0.0103115153730948));
#44406=CARTESIAN_POINT('Ctrl Pts',(-0.213967812670003,0.00491441191731313,
0.0103113549971935));
#44407=CARTESIAN_POINT('Ctrl Pts',(-0.214026111204022,0.00674788150248729,
0.0104576635446883));
#44408=CARTESIAN_POINT('Ctrl Pts',(-0.214023825957855,0.0067393313698133,
0.0105583088393878));
#44409=CARTESIAN_POINT('Ctrl Pts',(-0.214123907054786,0.00672978090006651,
0.0105592295780455));
#44410=CARTESIAN_POINT('Ctrl Pts',(-0.214108479671163,0.00763963123678071,
0.0104455505972963));
#44411=CARTESIAN_POINT('Ctrl Pts',(-0.214106198989655,0.00764109666123514,
0.0105460513513631));
#44412=CARTESIAN_POINT('Ctrl Pts',(-0.214206299904641,0.00763192741742352,
0.0105479200166305));
#44413=CARTESIAN_POINT('Ctrl Pts',(-0.214095599716215,0.00749962544805674,
0.0104463514425309));
#44414=CARTESIAN_POINT('Ctrl Pts',(-0.214095451794398,0.00749962504495062,
0.0104528968860796));
#44415=CARTESIAN_POINT('Ctrl Pts',(-0.214095949743277,0.0074996247400838,
0.0104594406003646));
#44416=CARTESIAN_POINT('Ctrl Pts',(-0.214098294561895,0.00749962431257035,
0.0104727457995799));
#44417=CARTESIAN_POINT('Ctrl Pts',(-0.214100218529235,0.00749962420408635,
0.0104794572967246));
#44418=CARTESIAN_POINT('Ctrl Pts',(-0.214107649508439,0.00749962419724419,
0.0104978607422557));
#44419=CARTESIAN_POINT('Ctrl Pts',(-0.214114741107808,0.00749962456581655,
0.0105087596981603));
#44420=CARTESIAN_POINT('Ctrl Pts',(-0.214132668598254,0.00749962578572488,
0.0105272808258854));
#44421=CARTESIAN_POINT('Ctrl Pts',(-0.214143338822552,0.00749962674612676,
0.0105347281746056));
#44422=CARTESIAN_POINT('Ctrl Pts',(-0.214165265741731,0.00749962751269912,
0.0105444626034586));
#44423=CARTESIAN_POINT('Ctrl Pts',(-0.214176063329797,0.00749964698774914,
0.0105472478399211));
#44424=CARTESIAN_POINT('Ctrl Pts',(-0.214189258751872,0.00749960790352974,
0.01054842300869));
#44425=CARTESIAN_POINT('Ctrl Pts',(-0.214191533580253,0.00749963570601337,
0.0105485497685965));
#44426=CARTESIAN_POINT('Ctrl Pts',(-0.214193732110184,0.00749963608528694,
0.0105485995171194));
#44427=CARTESIAN_POINT('Ctrl Pts',(-0.214099253446307,0.00745991385637808,
0.0104463443855313));
#44428=CARTESIAN_POINT('Ctrl Pts',(-0.214096974871178,0.0074595664991226,
0.0105467469842101));
#44429=CARTESIAN_POINT('Ctrl Pts',(-0.214196963190226,0.00746877681718598,
0.0105486179406832));
#44430=CARTESIAN_POINT('Ctrl Pts',(-0.214020082389909,0.00831894594433586,
0.0104483989904472));
#44431=CARTESIAN_POINT('Ctrl Pts',(-0.21401780385469,0.00832821903762263,
0.0105488339524259));
#44432=CARTESIAN_POINT('Ctrl Pts',(-0.214117811546728,0.00833738824368495,
0.0105498229681975));
#44433=CARTESIAN_POINT('Ctrl Pts',(-0.213876996985919,0.0100520920635664,
0.010205574644505));
#44434=CARTESIAN_POINT('Ctrl Pts',(-0.213874844832131,0.0100801808822668,
0.0103033571540271));
#44435=CARTESIAN_POINT('Ctrl Pts',(-0.213975821734514,0.010078672567526,
0.0103035150590047));
#44436=CARTESIAN_POINT('Ctrl Pts',(-0.2140923557601,0.0116453800387162,
0.00948777426694368));
#44437=CARTESIAN_POINT('Ctrl Pts',(-0.214090467670465,0.0116912347252608,
0.00957760306600306));
#44438=CARTESIAN_POINT('Ctrl Pts',(-0.214190047996671,0.0116802934198075,
0.00958479083026525));
#44439=CARTESIAN_POINT('Ctrl Pts',(-0.214205194686077,0.0123668777182512,
0.00903080634119371));
#44440=CARTESIAN_POINT('Ctrl Pts',(-0.214203492147884,0.0124206946345659,
0.00911558638282872));
#44441=CARTESIAN_POINT('Ctrl Pts',(-0.214303052117812,0.0124102602652885,
0.00912369507589516));
#44442=CARTESIAN_POINT('Ctrl Pts',(-0.223149958381768,0.00811836849261824,
0.0106277848801897));
#44443=CARTESIAN_POINT('Ctrl Pts',(-0.223149017147776,0.00812607888323874,
0.0107379352117485));
#44444=CARTESIAN_POINT('Ctrl Pts',(-0.223039596559705,0.00813431010703398,
0.0107253955357731));
#44445=CARTESIAN_POINT('Ctrl Pts',(-0.223032128491294,0.00689032892248409,
0.0107121280996051));
#44446=CARTESIAN_POINT('Ctrl Pts',(-0.223031160847443,0.006882589693257,
0.0108233580442053));
#44447=CARTESIAN_POINT('Ctrl Pts',(-0.222922016432433,0.00689506675999886,
0.010812206747988));
#44448=CARTESIAN_POINT('Ctrl Pts',(-0.222896076226969,0.00509605881161538,
0.0104620567002983));
#44449=CARTESIAN_POINT('Ctrl Pts',(-0.222895201503254,0.00506652282554446,
0.010570242247404));
#44450=CARTESIAN_POINT('Ctrl Pts',(-0.222784772879459,0.00507057089023076,
0.0105612791384786));
#44451=CARTESIAN_POINT('Ctrl Pts',(-0.223098674012225,0.00282059013172128,
0.00940055961423081));
#44452=CARTESIAN_POINT('Ctrl Pts',(-0.223098301276066,0.00276261015251879,
0.00949549531498266));
#44453=CARTESIAN_POINT('Ctrl Pts',(-0.222989560059633,0.00275270061654399,
0.00947735836584344));
#44454=CARTESIAN_POINT('Ctrl Pts',(-0.223394109819826,0.00185848636376366,
0.00868366986817202));
#44455=CARTESIAN_POINT('Ctrl Pts',(-0.223394052938567,0.00178892652705542,
0.00876990019161811));
#44456=CARTESIAN_POINT('Ctrl Pts',(-0.223287239065902,0.00177559498381319,
0.00874497678071077));
#44457=CARTESIAN_POINT('Ctrl Pts',(-0.223543079689471,0.0013353842698584,
0.00819234018549985));
#44458=CARTESIAN_POINT('Ctrl Pts',(-0.223543219690721,0.00125922959931456,
0.00827238454094328));
#44459=CARTESIAN_POINT('Ctrl Pts',(-0.223435511657072,0.00125080723173669,
0.00824921551534157));
#44460=CARTESIAN_POINT('Ctrl Pts',(-0.223310598482097,0.00172037988617517,
0.00866504379818179));
#44461=CARTESIAN_POINT('Ctrl Pts',(-0.223334018892059,0.00174295523481006,
0.0086842432411052));
#44462=CARTESIAN_POINT('Ctrl Pts',(-0.223347735408989,0.00175981983936743,
0.00868820455961472));
#44463=CARTESIAN_POINT('Ctrl Pts',(-0.223360552734813,0.00178149963234084,
0.00868907076646229));
#44464=CARTESIAN_POINT('Ctrl Pts',(-0.223361712493225,0.00178346129912069,
0.00868914914401873));
#44465=CARTESIAN_POINT('Ctrl Pts',(-0.223362865477419,0.00178547527971709,
0.00868917146628374));
#44466=CARTESIAN_POINT('Ctrl Pts',(-0.223364018586399,0.00178755268391809,
0.00868912731689215));
#44467=CARTESIAN_POINT('Ctrl Pts',(-0.223377915519196,0.00181258895287393,
0.00868859524131362));
#44468=CARTESIAN_POINT('Ctrl Pts',(-0.223391925265875,0.0018448159954703,
0.00867367215760806));
#44469=CARTESIAN_POINT('Ctrl Pts',(-0.223392285502192,0.00186163021866878,
0.00865321401664211));
#44470=CARTESIAN_POINT('Ctrl Pts',(-0.223092856247512,0.00749585351918229,
0.0106501223902346));
#44471=CARTESIAN_POINT('Ctrl Pts',(-0.223092684188288,0.00749585053885153,
0.0106565243090426));
#44472=CARTESIAN_POINT('Ctrl Pts',(-0.223091895251065,0.00749584774490668,
0.0106628947681154));
#44473=CARTESIAN_POINT('Ctrl Pts',(-0.223088984119591,0.00749584238255244,
0.0106759413684013));
#44474=CARTESIAN_POINT('Ctrl Pts',(-0.223086760080309,0.00749583987015413,
0.0106825588960641));
#44475=CARTESIAN_POINT('Ctrl Pts',(-0.223078509782108,0.00749583362413322,
0.0107006067727498));
#44476=CARTESIAN_POINT('Ctrl Pts',(-0.223070937121219,0.00749583072844963,
0.0107111744299137));
#44477=CARTESIAN_POINT('Ctrl Pts',(-0.223052200495654,0.00749582755061298,
0.0107288668954373));
#44478=CARTESIAN_POINT('Ctrl Pts',(-0.223041210292398,0.00749582731204073,
0.0107358251218091));
#44479=CARTESIAN_POINT('Ctrl Pts',(-0.223016508793546,0.00749582944608222,
0.010745485641849));
#44480=CARTESIAN_POINT('Ctrl Pts',(-0.223004129993207,0.00749585232722507,
0.0107474057105056));
#44481=CARTESIAN_POINT('Ctrl Pts',(-0.222992335031057,0.00749582914091336,
0.0107474337334615));
#44482=CARTESIAN_POINT('Ctrl Pts',(-0.222991908351812,0.00749582812340553,
0.0107474317741862));
#44483=CARTESIAN_POINT('Ctrl Pts',(-0.222991328193623,0.00749582309807586,
0.0107474258711083));
#44484=CARTESIAN_POINT('Ctrl Pts',(-0.222991070791995,0.00749582034034479,
0.0107474224622069));
#44485=CARTESIAN_POINT('Ctrl Pts',(-0.222990717313771,0.00749580780121696,
0.0107474166346042));
#44486=CARTESIAN_POINT('Ctrl Pts',(-0.222990358652687,0.00749571058866991,
0.0107474093363226));
#44487=CARTESIAN_POINT('Ctrl Pts',(-0.223038904064572,0.00685832243219836,
0.010724812432214));
#44488=CARTESIAN_POINT('Ctrl Pts',(-0.223148784830004,0.00686647913663685,
0.010737919478636));
#44489=CARTESIAN_POINT('Ctrl Pts',(-0.223149723157941,0.00687431556120157,
0.0106272599439884));
#44490=CARTESIAN_POINT('Ctrl Pts',(-0.222921342326663,0.00809554936511713,
0.0108125078527399));
#44491=CARTESIAN_POINT('Ctrl Pts',(-0.223030951289103,0.00810806473741712,
0.0108242266003475));
#44492=CARTESIAN_POINT('Ctrl Pts',(-0.223031916258244,0.00810040520679048,
0.0107124723755508));
#44493=CARTESIAN_POINT('Ctrl Pts',(-0.222788345558373,0.00991734046137115,
0.010564156394036));
#44494=CARTESIAN_POINT('Ctrl Pts',(-0.222899221435757,0.00992139891278033,
0.0105737275036333));
#44495=CARTESIAN_POINT('Ctrl Pts',(-0.222900094931727,0.00989188064193713,
0.0104649966425086));
#44496=CARTESIAN_POINT('Ctrl Pts',(-0.222991444217135,0.0122334116145978,
0.0094855742606813));
#44497=CARTESIAN_POINT('Ctrl Pts',(-0.223100651811751,0.0122237070864208,
0.00950419456187707));
#44498=CARTESIAN_POINT('Ctrl Pts',(-0.223101021860234,0.0121656229844738,
0.00940871624898466));
#44499=CARTESIAN_POINT('Ctrl Pts',(-0.223292823363305,0.0132097454493491,
0.0087567416927032));
#44500=CARTESIAN_POINT('Ctrl Pts',(-0.223399985861735,0.0131962649911677,
0.008782420408174));
#44501=CARTESIAN_POINT('Ctrl Pts',(-0.223400039587377,0.0131265633700794,
0.00869563825883883));
#44502=CARTESIAN_POINT('Ctrl Pts',(-0.22344293546994,0.0137344903751146,
0.00826334397677012));
#44503=CARTESIAN_POINT('Ctrl Pts',(-0.223551045285294,0.0137261671689852,
0.00828714676645308));
#44504=CARTESIAN_POINT('Ctrl Pts',(-0.223550904301479,0.0136498450124133,
0.00820654686920794));
#44505=CARTESIAN_POINT('Ctrl Pts',(-0.223398239295461,0.0131236886374436,
0.00866523263057392));
#44506=CARTESIAN_POINT('Ctrl Pts',(-0.223398136457366,0.0131285310204962,
0.0086711516106654));
#44507=CARTESIAN_POINT('Ctrl Pts',(-0.223397333177559,0.0131339979980512,
0.00867643268304301));
#44508=CARTESIAN_POINT('Ctrl Pts',(-0.223394275796221,0.0131465321569875,
0.0086860533648667));
#44509=CARTESIAN_POINT('Ctrl Pts',(-0.223391913440977,0.0131535682654236,
0.00869013199620513));
#44510=CARTESIAN_POINT('Ctrl Pts',(-0.223383973147319,0.013173032799877,
0.00869853055476966));
#44511=CARTESIAN_POINT('Ctrl Pts',(-0.223377414256092,0.0131856216462082,
0.00870103929587356));
#44512=CARTESIAN_POINT('Ctrl Pts',(-0.223362537151336,0.0132101069037078,
0.00870155990773004));
#44513=CARTESIAN_POINT('Ctrl Pts',(-0.223354204813562,0.0132219860216964,
0.00869951986497978));
#44514=CARTESIAN_POINT('Ctrl Pts',(-0.223333099159678,0.0132487347662511,
0.0086901514900253));
#44515=CARTESIAN_POINT('Ctrl Pts',(-0.223322907202441,0.0132589745048153,
0.00868212703059623));
#44516=CARTESIAN_POINT('Ctrl Pts',(-0.223319122967919,0.0132624468986076,
0.00867940053158316));
#44517=CARTESIAN_POINT('Ctrl Pts',(-0.223318458580742,0.0132632291985661,
0.00867876926620867));
#44518=CARTESIAN_POINT('Ctrl Pts',(-0.223317571560149,0.0132642671045371,
0.00867791950814091));
#44519=CARTESIAN_POINT('Ctrl Pts',(-0.223316827901763,0.0132649884239581,
0.00867730857776536));
#44520=CARTESIAN_POINT('Origin',(-0.224556024162841,0.00178554708722032,
0.00861247505820972));
#44521=CARTESIAN_POINT('Ctrl Pts',(-0.224391663448231,0.00186170363230323,
0.00867388685638973));
#44522=CARTESIAN_POINT('Ctrl Pts',(-0.224391690962794,0.00185664352167643,
0.00867986565017952));
#44523=CARTESIAN_POINT('Ctrl Pts',(-0.224392856591787,0.00185099742226291,
0.00868513708397277));
#44524=CARTESIAN_POINT('Ctrl Pts',(-0.224397633435892,0.00183756116645332,
0.00869519920844558));
#44525=CARTESIAN_POINT('Ctrl Pts',(-0.224401634564269,0.00182982774161729,
0.00869943878686519));
#44526=CARTESIAN_POINT('Ctrl Pts',(-0.224414113949786,0.00181002423968987,
0.00870751274989629));
#44527=CARTESIAN_POINT('Ctrl Pts',(-0.22442443867922,0.00179707585700994,
0.00871009377290731));
#44528=CARTESIAN_POINT('Ctrl Pts',(-0.224447611009241,0.00177277200820337,
0.00871020581134868));
#44529=CARTESIAN_POINT('Ctrl Pts',(-0.224459249259747,0.00176213704190661,
0.00870838563173362));
#44530=CARTESIAN_POINT('Ctrl Pts',(-0.224487175198716,0.00173924228049195,
0.00870091542899512));
#44531=CARTESIAN_POINT('Ctrl Pts',(-0.224500555793624,0.00173026352267406,
0.0086949372519814));
#44532=CARTESIAN_POINT('Ctrl Pts',(-0.224507687952234,0.00172570160913579,
0.00869169706224443));
#44533=CARTESIAN_POINT('Ctrl Pts',(-0.224510650816698,0.00172372736060054,
0.00869026741305131));
#44534=CARTESIAN_POINT('Ctrl Pts',(-0.224513611096056,0.00172182181281534,
0.00868875013016184));
#44535=CARTESIAN_POINT('Ctrl Pts',(-0.2245141337222,0.00172149608377577,
0.00868848845801025));
#44536=CARTESIAN_POINT('Origin',(-0.223237201119695,0.0132013902797598,
0.00859864717831064));
#44537=CARTESIAN_POINT('Ctrl Pts',(-0.224519290304243,0.0132629343303462,
0.00870151198403918));
#44538=CARTESIAN_POINT('Ctrl Pts',(-0.224519200559076,0.0132626799782016,
0.00870172096410461));
#44539=CARTESIAN_POINT('Ctrl Pts',(-0.224519196449931,0.0132626715913979,
0.00870172780918351));
#44540=CARTESIAN_POINT('Ctrl Pts',(-0.224519188792359,0.0132626563556557,
0.00870174023641345));
#44541=CARTESIAN_POINT('Ctrl Pts',(-0.224519185274485,0.0132626494990939,
0.00870174582616742));
#44542=CARTESIAN_POINT('Ctrl Pts',(-0.224519178967634,0.0132626374476326,
0.0087017556460159));
#44543=CARTESIAN_POINT('Ctrl Pts',(-0.224519176204388,0.0132626322455634,
0.00870175988314548));
#44544=CARTESIAN_POINT('Ctrl Pts',(-0.224519171386791,0.0132626233061751,
0.00870176716154422));
#44545=CARTESIAN_POINT('Ctrl Pts',(-0.224519169349119,0.01326261956404,
0.0087017702075175));
#44546=CARTESIAN_POINT('Ctrl Pts',(-0.224519165865502,0.0132626132308922,
0.00870177536105968));
#44547=CARTESIAN_POINT('Ctrl Pts',(-0.224519164428724,0.0132626106370534,
0.00870177747136503));
#44548=CARTESIAN_POINT('Ctrl Pts',(-0.224519109814946,0.0132625127185912,
0.00870185712094413));
#44549=CARTESIAN_POINT('Ctrl Pts',(-0.224519044966251,0.0132624206026821,
0.00870193150053024));
#44550=CARTESIAN_POINT('Ctrl Pts',(-0.224518723363153,0.0132620216461391,
0.00870225178079486));
#44551=CARTESIAN_POINT('Ctrl Pts',(-0.22451831276061,0.0132616574362571,
0.00870253961290821));
#44552=CARTESIAN_POINT('Ctrl Pts',(-0.224516797031972,0.0132605153113935,
0.0087034170474696));
#44553=CARTESIAN_POINT('Ctrl Pts',(-0.224515575979251,0.0132596901374382,
0.00870402972759247));
#44554=CARTESIAN_POINT('Ctrl Pts',(-0.224510961241942,0.0132565714802701,
0.00870628548407886));
#44555=CARTESIAN_POINT('Ctrl Pts',(-0.224503324979594,0.0132515404150939,
0.0087097732800045));
#44556=CARTESIAN_POINT('Ctrl Pts',(-0.224475263000761,0.0132307277045983,
0.00871981812048934));
#44557=CARTESIAN_POINT('Ctrl Pts',(-0.224458096051566,0.0132156922405316,
0.00872316939171254));
#44558=CARTESIAN_POINT('Ctrl Pts',(-0.224430971986936,0.0131873371827302,
0.00872296615606519));
#44559=CARTESIAN_POINT('Ctrl Pts',(-0.224420615526776,0.0131743978476805,
0.00872035132447665));
#44560=CARTESIAN_POINT('Ctrl Pts',(-0.224408099207843,0.0131546171954294,
0.00871222719279687));
#44561=CARTESIAN_POINT('Ctrl Pts',(-0.224404085463319,0.0131468940503105,
0.00870796860159257));
#44562=CARTESIAN_POINT('Ctrl Pts',(-0.22439929544596,0.0131334846526406,
0.00869787714577718));
#44563=CARTESIAN_POINT('Ctrl Pts',(-0.224398126033773,0.0131278539099209,
0.0086925975449782));
#44564=CARTESIAN_POINT('Ctrl Pts',(-0.224398096309527,0.0131228084948154,
0.00868661304198621));
#44565=CARTESIAN_POINT('Ctrl Pts',(-0.224249357172095,0.00812340187734315,
0.0107538157471281));
#44566=CARTESIAN_POINT('Ctrl Pts',(-0.224146973897669,0.00813179493343109,
0.0107527927564782));
#44567=CARTESIAN_POINT('Ctrl Pts',(-0.224150079053515,0.00812453493531191,
0.0106503798565657));
#44568=CARTESIAN_POINT('Ctrl Pts',(-0.22413240338219,0.00688538717073963,
0.0108391603821318));
#44569=CARTESIAN_POINT('Ctrl Pts',(-0.224030305893638,0.00689634351625541,
0.0108395260737771));
#44570=CARTESIAN_POINT('Ctrl Pts',(-0.224033442754283,0.00690340499464296,
0.0107361019261074));
#44571=CARTESIAN_POINT('Ctrl Pts',(-0.223994325524645,0.00506403357770048,
0.0105862477504909));
#44572=CARTESIAN_POINT('Ctrl Pts',(-0.22389096912139,0.00506508187178619,
0.0105884758775558));
#44573=CARTESIAN_POINT('Ctrl Pts',(-0.223893996001451,0.00509264619037901,
0.010487856035286));
#44574=CARTESIAN_POINT('Ctrl Pts',(-0.224201604501605,0.00275240868515444,
0.00950201908119746));
#44575=CARTESIAN_POINT('Ctrl Pts',(-0.224100039602147,0.00273684373946514,
0.0094938587310791));
#44576=CARTESIAN_POINT('Ctrl Pts',(-0.224102620321083,0.0027912050241893,
0.00940582756518366));
#44577=CARTESIAN_POINT('Ctrl Pts',(-0.224501847843731,0.00177835042191264,
0.00877050099325137));
#44578=CARTESIAN_POINT('Ctrl Pts',(-0.224401973174767,0.00175931878963782,
0.00875562557648048));
#44579=CARTESIAN_POINT('Ctrl Pts',(-0.224404292962857,0.00182452912855932,
0.00867585493377426));
#44580=CARTESIAN_POINT('Ctrl Pts',(-0.224648447652107,0.00125404116273978,
0.00827422479137384));
#44581=CARTESIAN_POINT('Ctrl Pts',(-0.224547784514112,0.00123874181242394,
0.00826029823960483));
#44582=CARTESIAN_POINT('Ctrl Pts',(-0.22454990776902,0.00130997806636779,
0.00818626753716696));
#44583=CARTESIAN_POINT('Ctrl Pts',(-0.224092574620247,0.00749537127813137,
0.0106722901056483));
#44584=CARTESIAN_POINT('Ctrl Pts',(-0.224092426749193,0.00749536783406251,
0.0106788326616221));
#44585=CARTESIAN_POINT('Ctrl Pts',(-0.224092923860089,0.00749536420926534,
0.0106853735535888));
#44586=CARTESIAN_POINT('Ctrl Pts',(-0.224095265168082,0.00749535646538972,
0.0106986729281663));
#44587=CARTESIAN_POINT('Ctrl Pts',(-0.224097186314513,0.00749535235120555,
0.0107053816423148));
#44588=CARTESIAN_POINT('Ctrl Pts',(-0.224104608477795,0.00749534046510422,
0.0107237822010604));
#44589=CARTESIAN_POINT('Ctrl Pts',(-0.224111693885709,0.00749533267179103,
0.0107346822263825));
#44590=CARTESIAN_POINT('Ctrl Pts',(-0.224129608634221,0.00749531781049727,
0.0107532062850313));
#44591=CARTESIAN_POINT('Ctrl Pts',(-0.22414027204642,0.00749531087304268,
0.0107606558993738));
#44592=CARTESIAN_POINT('Ctrl Pts',(-0.224171640221325,0.00749529490524347,
0.0107745952453094));
#44593=CARTESIAN_POINT('Ctrl Pts',(-0.224188233088826,0.0074952638518399,
0.0107744682362007));
#44594=CARTESIAN_POINT('Ctrl Pts',(-0.224190202947882,0.00749531042008945,
0.0107745260061853));
#44595=CARTESIAN_POINT('Ctrl Pts',(-0.224190645755837,0.00749528925575554,
0.0107745367966582));
#44596=CARTESIAN_POINT('Ctrl Pts',(-0.224149812609561,0.00686720535741763,
0.010649790663496));
#44597=CARTESIAN_POINT('Ctrl Pts',(-0.224146711244469,0.00685983841997734,
0.0107523672886193));
#44598=CARTESIAN_POINT('Ctrl Pts',(-0.224249268941159,0.00686819969821718,
0.0107532186162631));
#44599=CARTESIAN_POINT('Ctrl Pts',(-0.224033310137068,0.00808631398537909,
0.0107365279258389));
#44600=CARTESIAN_POINT('Ctrl Pts',(-0.22403017708648,0.00809326520017373,
0.0108401277556867));
#44601=CARTESIAN_POINT('Ctrl Pts',(-0.22413245162769,0.00810418695798438,
0.0108395912055622));
#44602=CARTESIAN_POINT('Ctrl Pts',(-0.2238976842394,0.00989438682845739,
0.0104910133496839));
#44603=CARTESIAN_POINT('Ctrl Pts',(-0.223894659126775,0.00992184394931338,
0.0105918383770759));
#44604=CARTESIAN_POINT('Ctrl Pts',(-0.223998181022725,0.0099227443382153,
0.010589479005002));
#44605=CARTESIAN_POINT('Ctrl Pts',(-0.224105465849081,0.0121940707688781,
0.00941469086371163));
#44606=CARTESIAN_POINT('Ctrl Pts',(-0.224102886673673,0.0122483552961644,
0.00950296817005453));
#44607=CARTESIAN_POINT('Ctrl Pts',(-0.224204619171975,0.0122326177690983,
0.0095109744704432));
#44608=CARTESIAN_POINT('Ctrl Pts',(-0.224411006674875,0.0131602565471824,
0.00868824099025048));
#44609=CARTESIAN_POINT('Ctrl Pts',(-0.224408686153195,0.0132254016455477,
0.00876828599846793));
#44610=CARTESIAN_POINT('Ctrl Pts',(-0.224508634511665,0.013205870656239,
0.00878325506714548));
#44611=CARTESIAN_POINT('Ctrl Pts',(-0.224558309212759,0.0136746544994099,
0.0082011925670837));
#44612=CARTESIAN_POINT('Ctrl Pts',(-0.224556183524894,0.0137458268082903,
0.00827552216554079));
#44613=CARTESIAN_POINT('Ctrl Pts',(-0.224656964137442,0.0137301873698191,
0.00828947824167215));
#44614=CARTESIAN_POINT('Ctrl Pts',(-0.211142486563875,0.0080074480565038,
0.0103648761595404));
#44615=CARTESIAN_POINT('Ctrl Pts',(-0.211140614754186,0.00801345371234465,
0.0104703133205799));
#44616=CARTESIAN_POINT('Ctrl Pts',(-0.211035650930516,0.00802210230267836,
0.01046212346533));
#44617=CARTESIAN_POINT('Ctrl Pts',(-0.211050986105208,0.00698795766404281,
0.010420173009799));
#44618=CARTESIAN_POINT('Ctrl Pts',(-0.211049098556023,0.00698197862819438,
0.0105262957002229));
#44619=CARTESIAN_POINT('Ctrl Pts',(-0.210944362702546,0.00699359357385201,
0.0105192069513736));
#44620=CARTESIAN_POINT('Ctrl Pts',(-0.210843042872648,0.00493702977004334,
0.0101824991063636));
#44621=CARTESIAN_POINT('Ctrl Pts',(-0.2108412497187,0.00490752878610045,
0.0102859125807657));
#44622=CARTESIAN_POINT('Ctrl Pts',(-0.210735016148891,0.00490827075542475,
0.0102812729590393));
#44623=CARTESIAN_POINT('Ctrl Pts',(-0.211127743567256,0.0030792588706987,
0.00929899472494895));
#44624=CARTESIAN_POINT('Ctrl Pts',(-0.211126355522171,0.00302779946025978,
0.00939201828722784));
#44625=CARTESIAN_POINT('Ctrl Pts',(-0.211022153864861,0.00301706240296407,
0.00937797060777647));
#44626=CARTESIAN_POINT('Ctrl Pts',(-0.21126360341789,0.00224772336844146,
0.00871402935073148));
#44627=CARTESIAN_POINT('Ctrl Pts',(-0.211262455310447,0.00218683116784316,
0.00880031650240356));
#44628=CARTESIAN_POINT('Ctrl Pts',(-0.211157900322863,0.00218003268842091,
0.00878692414041944));
#44629=CARTESIAN_POINT('Ctrl Pts',(-0.21109423290342,0.00261222544444838,
0.00907399385816615));
#44630=CARTESIAN_POINT('Ctrl Pts',(-0.211095031960242,0.00261300460420345,
0.00907449760819488));
#44631=CARTESIAN_POINT('Ctrl Pts',(-0.211097157079409,0.00261503310819839,
0.00907577366587372));
#44632=CARTESIAN_POINT('Ctrl Pts',(-0.211099274163331,0.00261711947062296,
0.00907696675928809));
#44633=CARTESIAN_POINT('Ctrl Pts',(-0.211106432645342,0.00262449778379525,
0.00908107870213868));
#44634=CARTESIAN_POINT('Ctrl Pts',(-0.21111600284729,0.00263459647919183,
0.00908575699516419));
#44635=CARTESIAN_POINT('Ctrl Pts',(-0.211135588383209,0.00265827370691382,
0.00909042483809797));
#44636=CARTESIAN_POINT('Ctrl Pts',(-0.211144153168982,0.00266957861391556,
0.00909085164184115));
#44637=CARTESIAN_POINT('Ctrl Pts',(-0.211160507568082,0.00269370053702988,
0.00908736306728261));
#44638=CARTESIAN_POINT('Ctrl Pts',(-0.21116761520281,0.00270579305709638,
0.00908311389605883));
#44639=CARTESIAN_POINT('Ctrl Pts',(-0.211176248866459,0.00272362436611357,
0.00907263073110103));
#44640=CARTESIAN_POINT('Ctrl Pts',(-0.211178930690465,0.00273018991641854,
0.00906763592813339));
#44641=CARTESIAN_POINT('Ctrl Pts',(-0.211182404594494,0.00274156776870138,
0.00905631334382395));
#44642=CARTESIAN_POINT('Ctrl Pts',(-0.211183323601348,0.00274637390157652,
0.0090502845748891));
#44643=CARTESIAN_POINT('Ctrl Pts',(-0.211183450833508,0.00275046291514153,
0.0090436740602087));
#44644=CARTESIAN_POINT('Ctrl Pts',(-0.21109653717437,0.00749997694345283,
0.0103787828226083));
#44645=CARTESIAN_POINT('Ctrl Pts',(-0.211096377051465,0.0074999768281518,
0.0103852568676532));
#44646=CARTESIAN_POINT('Ctrl Pts',(-0.211095585865638,0.00749997659773733,
0.0103916996961516));
#44647=CARTESIAN_POINT('Ctrl Pts',(-0.211092658094877,0.00749997587113233,
0.0104048162942189));
#44648=CARTESIAN_POINT('Ctrl Pts',(-0.211090433159657,0.00749997535858776,
0.0104114340036142));
#44649=CARTESIAN_POINT('Ctrl Pts',(-0.211082179478388,0.00749997349822519,
0.0104294826171081));
#44650=CARTESIAN_POINT('Ctrl Pts',(-0.211074603814682,0.00749997184524541,
0.0104400500418335));
#44651=CARTESIAN_POINT('Ctrl Pts',(-0.211055860329739,0.00749996745397796,
0.0104577422926592));
#44652=CARTESIAN_POINT('Ctrl Pts',(-0.211044865979588,0.0074999649596482,
0.010464700090393));
#44653=CARTESIAN_POINT('Ctrl Pts',(-0.211020921400677,0.00749995680559278,
0.0104740606920776));
#44654=CARTESIAN_POINT('Ctrl Pts',(-0.211009742857274,0.00749997562380762,
0.0104758098878422));
#44655=CARTESIAN_POINT('Ctrl Pts',(-0.210998444007994,0.00749991418408376,
0.010476303815204));
#44656=CARTESIAN_POINT('Ctrl Pts',(-0.210996046515157,0.00749996002718701,
0.0104763293718199));
#44657=CARTESIAN_POINT('Ctrl Pts',(-0.210993907311933,0.00749995962611463,
0.0104762811460141));
#44658=CARTESIAN_POINT('Ctrl Pts',(-0.211264233927682,0.0127511389206587,
0.00871469219517674));
#44659=CARTESIAN_POINT('Ctrl Pts',(-0.211263339626816,0.0128119565920338,
0.00880095561734849));
#44660=CARTESIAN_POINT('Ctrl Pts',(-0.211158825258817,0.0128189223440845,
0.00878785171549552));
#44661=CARTESIAN_POINT('Ctrl Pts',(-0.211128617377145,0.0119162340263877,
0.00930117032032682));
#44662=CARTESIAN_POINT('Ctrl Pts',(-0.211127481783243,0.0119675771074036,
0.00939418426185652));
#44663=CARTESIAN_POINT('Ctrl Pts',(-0.211023317817383,0.0119783876644333,
0.00938046409104126));
#44664=CARTESIAN_POINT('Ctrl Pts',(-0.210843657835916,0.0100628466537089,
0.0101822731973737));
#44665=CARTESIAN_POINT('Ctrl Pts',(-0.210842123435839,0.0100923256739967,
0.0102856191594558));
#44666=CARTESIAN_POINT('Ctrl Pts',(-0.210735935133894,0.0100919118355424,
0.0102812355219947));
#44667=CARTESIAN_POINT('Ctrl Pts',(-0.211051061885002,0.00800517834552088,
0.0104208257432116));
#44668=CARTESIAN_POINT('Ctrl Pts',(-0.211049429352862,0.00801110099720398,
0.0105268952080997));
#44669=CARTESIAN_POINT('Ctrl Pts',(-0.21094474436933,0.00799938724367094,
0.010520142978524));
#44670=CARTESIAN_POINT('Ctrl Pts',(-0.21114359232468,0.00698385841965477,
0.0103640872892378));
#44671=CARTESIAN_POINT('Ctrl Pts',(-0.211141976460829,0.00697777627165395,
0.0104694570977041));
#44672=CARTESIAN_POINT('Ctrl Pts',(-0.211037057567724,0.00696911234332138,
0.0104615765116688));
#44673=CARTESIAN_POINT('Ctrl Pts',(-0.211184221002222,0.0122473944266094,
0.00904500436478942));
#44674=CARTESIAN_POINT('Ctrl Pts',(-0.211184098199553,0.0122513346632141,
0.00905137936580629));
#44675=CARTESIAN_POINT('Ctrl Pts',(-0.211183238943289,0.0122559428744482,
0.00905721691973273));
#44676=CARTESIAN_POINT('Ctrl Pts',(-0.211179996364333,0.0122668101284925,
0.0090682227412344));
#44677=CARTESIAN_POINT('Ctrl Pts',(-0.211177497911413,0.0122730645346206,
0.00907312167743916));
#44678=CARTESIAN_POINT('Ctrl Pts',(-0.211169298567438,0.0122903498693054,
0.00908371038952613));
#44679=CARTESIAN_POINT('Ctrl Pts',(-0.211162424900141,0.0123022235298793,
0.0090881533960612));
#44680=CARTESIAN_POINT('Ctrl Pts',(-0.211146016988589,0.0123267344228518,
0.00909225293758861));
#44681=CARTESIAN_POINT('Ctrl Pts',(-0.211137049460936,0.0123386291345285,
0.00909194384282742));
#44682=CARTESIAN_POINT('Ctrl Pts',(-0.211114733857186,0.0123655993569228,
0.00908674967640739));
#44683=CARTESIAN_POINT('Ctrl Pts',(-0.211104000080846,0.0123765165947633,
0.00908073975421946));
#44684=CARTESIAN_POINT('Ctrl Pts',(-0.211098076742061,0.0123822937242966,
0.00907744499712002));
#44685=CARTESIAN_POINT('Ctrl Pts',(-0.211096579367605,0.0123839782188275,
0.00907641698839438));
#44686=CARTESIAN_POINT('Ctrl Pts',(-0.211094964997266,0.012385550393988,
0.00907540111084567));
#44687=CARTESIAN_POINT('Origin',(-0.21234691445843,0.00266705858836579,
0.00901527131884535));
#44688=CARTESIAN_POINT('Ctrl Pts',(-0.212183839051124,0.00275127645488708,
0.00906545020201979));
#44689=CARTESIAN_POINT('Ctrl Pts',(-0.212183806161036,0.00274710028676507,
0.00907203561543755));
#44690=CARTESIAN_POINT('Ctrl Pts',(-0.212184810900476,0.0027422375390462,
0.00907802538757539));
#44691=CARTESIAN_POINT('Ctrl Pts',(-0.212189027067766,0.00273042441974619,
0.00908970636821214));
#44692=CARTESIAN_POINT('Ctrl Pts',(-0.212192551418784,0.00272345730579584,
0.00909491757756041));
#44693=CARTESIAN_POINT('Ctrl Pts',(-0.212203716791087,0.00270508615455126,
0.00910561706884515));
#44694=CARTESIAN_POINT('Ctrl Pts',(-0.212212986854008,0.00269271750821749,
0.00910997223485915));
#44695=CARTESIAN_POINT('Ctrl Pts',(-0.212234368520539,0.00266825497643102,
0.00911363069173713));
#44696=CARTESIAN_POINT('Ctrl Pts',(-0.212245511720789,0.00265695351087488,
0.0091132640080577));
#44697=CARTESIAN_POINT('Ctrl Pts',(-0.212273582499721,0.00263101628233386,
0.00910841099827345));
#44698=CARTESIAN_POINT('Ctrl Pts',(-0.212287289141522,0.002620499708973,
0.00910266326508716));
#44699=CARTESIAN_POINT('Ctrl Pts',(-0.21229225893459,0.00261687235876597,
0.00910069349159562));
#44700=CARTESIAN_POINT('Ctrl Pts',(-0.212293365405452,0.00261594584361789,
0.00910016633472597));
#44701=CARTESIAN_POINT('Ctrl Pts',(-0.212294848987994,0.00261471070565374,
0.00909944936359943));
#44702=CARTESIAN_POINT('Ctrl Pts',(-0.212296006564873,0.00261384619513498,
0.00909892989563823));
#44703=CARTESIAN_POINT('Origin',(-0.21102377360653,0.0123325634480328,0.00898917035815447));
#44704=CARTESIAN_POINT('Ctrl Pts',(-0.212185024851611,0.0122473868968752,
0.00906629440501006));
#44705=CARTESIAN_POINT('Ctrl Pts',(-0.21218499368264,0.0122514417819006,
0.00907268872464956));
#44706=CARTESIAN_POINT('Ctrl Pts',(-0.212185940713764,0.0122561465343213,
0.00907852372725697));
#44707=CARTESIAN_POINT('Ctrl Pts',(-0.212189922634149,0.0122675536441838,
0.00908994240071966));
#44708=CARTESIAN_POINT('Ctrl Pts',(-0.212193252686342,0.012274274904222,
0.00909507756545489));
#44709=CARTESIAN_POINT('Ctrl Pts',(-0.212203944292361,0.0122922017002173,
0.00910582928455576));
#44710=CARTESIAN_POINT('Ctrl Pts',(-0.212212926014891,0.0123043686350945,
0.00911031870680742));
#44711=CARTESIAN_POINT('Ctrl Pts',(-0.212233698933047,0.0123284672250172,
0.00911434545853006));
#44712=CARTESIAN_POINT('Ctrl Pts',(-0.212244528204772,0.0123396058993226,
0.00911420588103199));
#44713=CARTESIAN_POINT('Ctrl Pts',(-0.212268288631956,0.0123619113149257,
0.00911055546564033));
#44714=CARTESIAN_POINT('Ctrl Pts',(-0.212280174342974,0.01237173556129,
0.00910673512663782));
#44715=CARTESIAN_POINT('Ctrl Pts',(-0.212290708620157,0.0123800530976797,
0.00910246249537526));
#44716=CARTESIAN_POINT('Ctrl Pts',(-0.212293399168351,0.0123820998196263,
0.00910138307795224));
#44717=CARTESIAN_POINT('Ctrl Pts',(-0.212296097533959,0.0123840891664848,
0.00910022666793963));
#44718=CARTESIAN_POINT('Ctrl Pts',(-0.212297179495208,0.0123848983299051,
0.00909974062817284));
#44719=CARTESIAN_POINT('Ctrl Pts',(-0.212223983669684,0.00249578230024466,
0.0089026290048257));
#44720=CARTESIAN_POINT('Ctrl Pts',(-0.212222315239459,0.00244051993255814,
0.00898671564148847));
#44721=CARTESIAN_POINT('Ctrl Pts',(-0.212322077234447,0.00245097194074628,
0.00899481297505414));
#44722=CARTESIAN_POINT('Ctrl Pts',(-0.212102881444989,0.00325528982487909,
0.00940104945131877));
#44723=CARTESIAN_POINT('Ctrl Pts',(-0.212101008701363,0.00320837525514172,
0.00949063004707617));
#44724=CARTESIAN_POINT('Ctrl Pts',(-0.212200694817127,0.00322011434363844,
0.00949811209657471));
#44725=CARTESIAN_POINT('Ctrl Pts',(-0.211865003483227,0.00494001687375164,
0.0101751329037738));
#44726=CARTESIAN_POINT('Ctrl Pts',(-0.211862844425244,0.00491188107110286,
0.0102732804691239));
#44727=CARTESIAN_POINT('Ctrl Pts',(-0.21196410551886,0.00491301061554956,
0.0102728695412691));
#44728=CARTESIAN_POINT('Ctrl Pts',(-0.212031241817383,0.00678912318233929,
0.0104179560391845));
#44729=CARTESIAN_POINT('Ctrl Pts',(-0.212028952115924,0.00678104752068375,
0.0105187548105473));
#44730=CARTESIAN_POINT('Ctrl Pts',(-0.212129112768025,0.00677136833426455,
0.0105196250578453));
#44731=CARTESIAN_POINT('Ctrl Pts',(-0.212114504545825,0.00770097981231512,
0.0103993205832573));
#44732=CARTESIAN_POINT('Ctrl Pts',(-0.212112222397844,0.00770313035708446,
0.0104999025723028));
#44733=CARTESIAN_POINT('Ctrl Pts',(-0.212212429687323,0.00769408823802094,
0.0105017420392689));
#44734=CARTESIAN_POINT('Ctrl Pts',(-0.212096206023604,0.00749993571117328,
0.0104011636214085));
#44735=CARTESIAN_POINT('Ctrl Pts',(-0.212096058107311,0.00749993554536779,
0.0104077087912101));
#44736=CARTESIAN_POINT('Ctrl Pts',(-0.212096555950432,0.00749993549141056,
0.0104142522424083));
#44737=CARTESIAN_POINT('Ctrl Pts',(-0.212098900330544,0.0074999356028455,
0.0104275568839437));
#44738=CARTESIAN_POINT('Ctrl Pts',(-0.212100823945479,0.00749993578221901,
0.0104342681194624));
#44739=CARTESIAN_POINT('Ctrl Pts',(-0.21210825374142,0.00749993661233937,
0.0104526711907501));
#44740=CARTESIAN_POINT('Ctrl Pts',(-0.212115344415089,0.00749993753547336,
0.0104635702349915));
#44741=CARTESIAN_POINT('Ctrl Pts',(-0.212133269910862,0.00749993983848996,
0.0104820915741914));
#44742=CARTESIAN_POINT('Ctrl Pts',(-0.212143939004055,0.00749994130999428,
0.0104895391360646));
#44743=CARTESIAN_POINT('Ctrl Pts',(-0.212165862168942,0.00749994301250812,
0.010499273169891));
#44744=CARTESIAN_POINT('Ctrl Pts',(-0.21217665941563,0.00749996174420459,
0.0105020595732478));
#44745=CARTESIAN_POINT('Ctrl Pts',(-0.212189860872875,0.00749992542283543,
0.0105032352134824));
#44746=CARTESIAN_POINT('Ctrl Pts',(-0.21219212844858,0.00749995163156639,
0.0105033615643368));
#44747=CARTESIAN_POINT('Ctrl Pts',(-0.212194330077505,0.0074999520583401,
0.0105034113689146));
#44748=CARTESIAN_POINT('Ctrl Pts',(-0.212122643014497,0.00721116078184923,
0.0103971097759903));
#44749=CARTESIAN_POINT('Ctrl Pts',(-0.212120363487194,0.00720802729624083,
0.010497586965253));
#44750=CARTESIAN_POINT('Ctrl Pts',(-0.212220493457096,0.00721701301401138,
0.0104996005393699));
#44751=CARTESIAN_POINT('Ctrl Pts',(-0.212036325010947,0.00815119828716712,
0.0104254852752672));
#44752=CARTESIAN_POINT('Ctrl Pts',(-0.212034033518481,0.00815861469739573,
0.0105262875146844));
#44753=CARTESIAN_POINT('Ctrl Pts',(-0.212134073861582,0.00816870458555384,
0.0105272711067881));
#44754=CARTESIAN_POINT('Ctrl Pts',(-0.211859115886666,0.0100584037447509,
0.0101853003279626));
#44755=CARTESIAN_POINT('Ctrl Pts',(-0.21185695613268,0.0100864888835407,
0.0102834827569533));
#44756=CARTESIAN_POINT('Ctrl Pts',(-0.211958176233036,0.0100851831560035,
0.0102830553358484));
#44757=CARTESIAN_POINT('Ctrl Pts',(-0.212112363322094,0.0117994791176497,
0.00937556698882922));
#44758=CARTESIAN_POINT('Ctrl Pts',(-0.21211050258229,0.0118469745004918,
0.00946479106560511));
#44759=CARTESIAN_POINT('Ctrl Pts',(-0.212210060685816,0.0118349787021983,
0.00947257912918343));
#44760=CARTESIAN_POINT('Ctrl Pts',(-0.212236638315871,0.0125752680371152,
0.00885550734677693));
#44761=CARTESIAN_POINT('Ctrl Pts',(-0.212234990566732,0.0126312664694345,
0.00893900834297023));
#44762=CARTESIAN_POINT('Ctrl Pts',(-0.212334686483614,0.0126210294980898,
0.00894719768338886));
#44763=CARTESIAN_POINT('Ctrl Pts',(-0.201155083193269,0.00216605663322667,
0.00858641232141098));
#44764=CARTESIAN_POINT('Ctrl Pts',(-0.20126096852948,0.00217232885330737,
0.00860101494802211));
#44765=CARTESIAN_POINT('Ctrl Pts',(-0.201261986180025,0.00223315111724539,
0.00851290633848732));
#44766=CARTESIAN_POINT('Ctrl Pts',(-0.201015029040136,0.00301234855195945,
0.00917044619233868));
#44767=CARTESIAN_POINT('Ctrl Pts',(-0.201120551074898,0.00302307644571231,
0.00918585713566367));
#44768=CARTESIAN_POINT('Ctrl Pts',(-0.201121818425293,0.00307436667035424,
0.00909110352796063));
#44769=CARTESIAN_POINT('Ctrl Pts',(-0.200741067091076,0.00490726025933776,
0.0100583553626889));
#44770=CARTESIAN_POINT('Ctrl Pts',(-0.200848644805918,0.00490457525049167,
0.0100640174517916));
#44771=CARTESIAN_POINT('Ctrl Pts',(-0.200850325606794,0.00493402244947655,
0.00995912466295495));
#44772=CARTESIAN_POINT('Ctrl Pts',(-0.200951724696489,0.00699776383342617,
0.0102933591526183));
#44773=CARTESIAN_POINT('Ctrl Pts',(-0.201057850521067,0.00698686745950293,
0.0103020115942979));
#44774=CARTESIAN_POINT('Ctrl Pts',(-0.201059631591013,0.00699277642326086,
0.0101944386176339));
#44775=CARTESIAN_POINT('Ctrl Pts',(-0.201035033694427,0.00803074714201528,
0.0102357737307844));
#44776=CARTESIAN_POINT('Ctrl Pts',(-0.201141386046049,0.00802257307788267,
0.0102453298409531));
#44777=CARTESIAN_POINT('Ctrl Pts',(-0.201143149297188,0.00801650549987341,
0.0101384442232337));
#44778=CARTESIAN_POINT('Ctrl Pts',(-0.201091335837404,0.0026023195479385,
0.00887000708307585));
#44779=CARTESIAN_POINT('Ctrl Pts',(-0.201092103354299,0.00260307247533696,
0.00887048379371787));
#44780=CARTESIAN_POINT('Ctrl Pts',(-0.201094259127555,0.00260513759398771,
0.00887175759780278));
#44781=CARTESIAN_POINT('Ctrl Pts',(-0.201096406464209,0.00260726257920991,
0.00887294403254245));
#44782=CARTESIAN_POINT('Ctrl Pts',(-0.201103264331842,0.00261437781908026,
0.0088768215853111));
#44783=CARTESIAN_POINT('Ctrl Pts',(-0.201112806708188,0.00262443779776055,
0.00888148334083447));
#44784=CARTESIAN_POINT('Ctrl Pts',(-0.20113267431363,0.00264850045287698,
0.00888598603513365));
#44785=CARTESIAN_POINT('Ctrl Pts',(-0.201141236183842,0.00265980541514074,
0.00888630262824218));
#44786=CARTESIAN_POINT('Ctrl Pts',(-0.201157583248774,0.00268388487459801,
0.0088825801587399));
#44787=CARTESIAN_POINT('Ctrl Pts',(-0.201164687512606,0.00269593311189708,
0.0088782145592798));
#44788=CARTESIAN_POINT('Ctrl Pts',(-0.201173315148115,0.00271365901443599,
0.00886756153217392));
#44789=CARTESIAN_POINT('Ctrl Pts',(-0.201175994276017,0.00272017405179653,
0.00886250578309987));
#44790=CARTESIAN_POINT('Ctrl Pts',(-0.201179464367247,0.00273144061067142,
0.00885107958730227));
#44791=CARTESIAN_POINT('Ctrl Pts',(-0.201180382062519,0.00273618870506716,
0.00884500762653599));
#44792=CARTESIAN_POINT('Ctrl Pts',(-0.201180508584589,0.00274021505325842,
0.00883836137431511));
#44793=CARTESIAN_POINT('Ctrl Pts',(-0.201099833981514,0.00749931673585989,
0.0101528932886838));
#44794=CARTESIAN_POINT('Ctrl Pts',(-0.201098485659853,0.00749931248699838,
0.0102056974765971));
#44795=CARTESIAN_POINT('Ctrl Pts',(-0.201049336965903,0.00749928794470734,
0.010251525133989));
#44796=CARTESIAN_POINT('Ctrl Pts',(-0.200997245792689,0.0074992653969341,
0.0102503478276375));
#44797=CARTESIAN_POINT('Ctrl Pts',(-0.201256650812755,0.0127742337711833,
0.00853880624905052));
#44798=CARTESIAN_POINT('Ctrl Pts',(-0.201250184418728,0.0127904275512369,
0.00856079060756085));
#44799=CARTESIAN_POINT('Ctrl Pts',(-0.201237195582423,0.0128229554728312,
0.00860494987658638));
#44800=CARTESIAN_POINT('Ctrl Pts',(-0.201182619048712,0.0128358773798212,
0.00861051744946986));
#44801=CARTESIAN_POINT('Ctrl Pts',(-0.201155303926009,0.0128424090648251,
0.00861339759601743));
#44802=CARTESIAN_POINT('Ctrl Pts',(-0.201208595417358,0.0124465598212127,
0.00871977498087392));
#44803=CARTESIAN_POINT('Ctrl Pts',(-0.201202102965136,0.0124617746892246,
0.00874233334840889));
#44804=CARTESIAN_POINT('Ctrl Pts',(-0.201189061786604,0.0124923363019008,
0.00878764561077419));
#44805=CARTESIAN_POINT('Ctrl Pts',(-0.201134434005491,0.0125046664137396,
0.00879380973072894));
#44806=CARTESIAN_POINT('Ctrl Pts',(-0.201107093146125,0.0125108979201374,
0.00879699065408895));
#44807=CARTESIAN_POINT('Ctrl Pts',(-0.201127094918058,0.0119476316067464,
0.00903388131834477));
#44808=CARTESIAN_POINT('Ctrl Pts',(-0.201120570437375,0.0119614484304572,
0.00905738721554734));
#44809=CARTESIAN_POINT('Ctrl Pts',(-0.201107464924307,0.0119892018368183,
0.00910460275007228));
#44810=CARTESIAN_POINT('Ctrl Pts',(-0.201052858340458,0.012001410986791,
0.00911138733244231));
#44811=CARTESIAN_POINT('Ctrl Pts',(-0.201025527938516,0.0120075758779105,
0.00911488262945839));
#44812=CARTESIAN_POINT('Ctrl Pts',(-0.201008085070164,0.0110295302488516,
0.00946855886042181));
#44813=CARTESIAN_POINT('Ctrl Pts',(-0.201001473220532,0.0110404306864664,
0.0094935350509485));
#44814=CARTESIAN_POINT('Ctrl Pts',(-0.200988192212286,0.0110623260425169,
0.00954370391606149));
#44815=CARTESIAN_POINT('Ctrl Pts',(-0.200933255780015,0.0110714126965106,
0.00955270028796668));
#44816=CARTESIAN_POINT('Ctrl Pts',(-0.200905760079558,0.0110760036237351,
0.00955730787255131));
#44817=CARTESIAN_POINT('Ctrl Pts',(-0.2009503980621,0.0100226663357829,
0.00982992257831994));
#44818=CARTESIAN_POINT('Ctrl Pts',(-0.200943711780911,0.010030070211669,
0.00985618971045741));
#44819=CARTESIAN_POINT('Ctrl Pts',(-0.200930281264408,0.0100449421374034,
0.00990895164817973));
#44820=CARTESIAN_POINT('Ctrl Pts',(-0.200875054282338,0.0100483822204513,
0.00992028137773493));
#44821=CARTESIAN_POINT('Ctrl Pts',(-0.200847412988371,0.0100501346700953,
0.00992606124313427));
#44822=CARTESIAN_POINT('Ctrl Pts',(-0.200985752557974,0.00896573313553926,
0.010048170465822));
#44823=CARTESIAN_POINT('Ctrl Pts',(-0.200979059787987,0.00896968565447399,
0.0100751056398674));
#44824=CARTESIAN_POINT('Ctrl Pts',(-0.200965616237646,0.00897762495126472,
0.0101292094517371));
#44825=CARTESIAN_POINT('Ctrl Pts',(-0.200910533124437,0.00897646676150334,
0.010141131282486));
#44826=CARTESIAN_POINT('Ctrl Pts',(-0.20088296373237,0.00897590505164646,
0.0101472101147103));
#44827=CARTESIAN_POINT('Ctrl Pts',(-0.20105982521262,0.00795581183071892,
0.0101560920619458));
#44828=CARTESIAN_POINT('Ctrl Pts',(-0.201053134234794,0.0079566211870063,
0.0101833039398003));
#44829=CARTESIAN_POINT('Ctrl Pts',(-0.201039694284309,0.00795824691477156,
0.0102379635576509));
#44830=CARTESIAN_POINT('Ctrl Pts',(-0.200984724529276,0.00795415818384021,
0.0102497134489866));
#44831=CARTESIAN_POINT('Ctrl Pts',(-0.200957211820981,0.00795211748649824,
0.0102557075311292));
#44832=CARTESIAN_POINT('Ctrl Pts',(-0.201111796847579,0.00736530035222225,
0.0101482803792522));
#44833=CARTESIAN_POINT('Ctrl Pts',(-0.201105107498193,0.00736435844767988,
0.0101754262075262));
#44834=CARTESIAN_POINT('Ctrl Pts',(-0.2010916708187,0.00736246647452709,
0.0102299531537233));
#44835=CARTESIAN_POINT('Ctrl Pts',(-0.201036707330346,0.00735763278097222,
0.0102413477195797));
#44836=CARTESIAN_POINT('Ctrl Pts',(-0.201009197762365,0.00735521193479846,
0.0102471638589911));
#44837=CARTESIAN_POINT('Ctrl Pts',(-0.201142066721907,0.00699237110554977,
0.0101642439779473));
#44838=CARTESIAN_POINT('Ctrl Pts',(-0.201135378229863,0.00699029770385,
0.0101914152333036));
#44839=CARTESIAN_POINT('Ctrl Pts',(-0.201121943272494,0.00698613292899819,
0.0102459932540579));
#44840=CARTESIAN_POINT('Ctrl Pts',(-0.20106700142688,0.00698054335286895,
0.0102572385002951));
#44841=CARTESIAN_POINT('Ctrl Pts',(-0.201039502683419,0.00697773961910315,
0.0102629800957228));
#44842=CARTESIAN_POINT('Ctrl Pts',(-0.201177053601335,0.0122550060276839,
0.00884070721774072));
#44843=CARTESIAN_POINT('Ctrl Pts',(-0.20117084753263,0.0122690513730654,
0.0088625295460327));
#44844=CARTESIAN_POINT('Ctrl Pts',(-0.201164660143918,0.0122901709254442,
0.00888140040275825));
#44845=CARTESIAN_POINT('Ctrl Pts',(-0.201150491997757,0.012310871344524,
0.00888736415769192));
#44846=CARTESIAN_POINT('Ctrl Pts',(-0.201132286732426,0.0123374702105669,
0.00889502724499377));
#44847=CARTESIAN_POINT('Ctrl Pts',(-0.201103744801886,0.0123645072421567,
0.00888409859256188));
#44848=CARTESIAN_POINT('Ctrl Pts',(-0.20108848344321,0.0123927133101065,
0.00887232988670267));
#44849=CARTESIAN_POINT('Origin',(-0.202343907248651,0.0026559890716155,
0.00881026065166738));
#44850=CARTESIAN_POINT('Ctrl Pts',(-0.202180796597781,0.00274072101466718,
0.00885976287803625));
#44851=CARTESIAN_POINT('Ctrl Pts',(-0.20218076839761,0.00273661010376764,
0.0088663730597778));
#44852=CARTESIAN_POINT('Ctrl Pts',(-0.202181774626836,0.00273180944123569,
0.00887239520899083));
#44853=CARTESIAN_POINT('Ctrl Pts',(-0.202185992690961,0.00272010970759771,
0.00888417484072343));
#44854=CARTESIAN_POINT('Ctrl Pts',(-0.202189521425533,0.00271318748468188,
0.00888944907905161));
#44855=CARTESIAN_POINT('Ctrl Pts',(-0.202200697689997,0.0026949096883953,
0.00890031160453069));
#44856=CARTESIAN_POINT('Ctrl Pts',(-0.202209975776181,0.00268257757595377,
0.00890477601358085));
#44857=CARTESIAN_POINT('Ctrl Pts',(-0.202231502282787,0.00265799781199361,
0.00890867262799436));
#44858=CARTESIAN_POINT('Ctrl Pts',(-0.202242804632951,0.00264655434339955,
0.00890837604318305));
#44859=CARTESIAN_POINT('Ctrl Pts',(-0.202271224259584,0.00262032723305801,
0.00890360222775761));
#44860=CARTESIAN_POINT('Ctrl Pts',(-0.202285063897618,0.00260966649176247,
0.00889780688643869));
#44861=CARTESIAN_POINT('Ctrl Pts',(-0.202290010562206,0.00260614356034156,
0.00889590681455424));
#44862=CARTESIAN_POINT('Ctrl Pts',(-0.202290907367527,0.00260535459335703,
0.00889546010904801));
#44863=CARTESIAN_POINT('Ctrl Pts',(-0.202292110547019,0.00260430091210787,
0.00889485527913338));
#44864=CARTESIAN_POINT('Ctrl Pts',(-0.202293070892211,0.00260358016718893,
0.00889443116859542));
#44865=CARTESIAN_POINT('Origin',(-0.201017179898206,0.0123408640444401,
0.0087860767507338));
#44866=CARTESIAN_POINT('Ctrl Pts',(-0.202178488577975,0.0122548116993251,
0.00886238997990231));
#44867=CARTESIAN_POINT('Ctrl Pts',(-0.202178460670578,0.0122588178162135,
0.00886883835749566));
#44868=CARTESIAN_POINT('Ctrl Pts',(-0.202179416149129,0.0122634820086249,
0.00887473017188245));
#44869=CARTESIAN_POINT('Ctrl Pts',(-0.202183428804187,0.0122748259653014,
0.00888628518227572));
#44870=CARTESIAN_POINT('Ctrl Pts',(-0.202186785687581,0.0122815298877756,
0.00889149430525874));
#44871=CARTESIAN_POINT('Ctrl Pts',(-0.202197543161461,0.0122994101048659,
0.00890240889430388));
#44872=CARTESIAN_POINT('Ctrl Pts',(-0.202206565485128,0.0123115589479267,
0.0089069960771264));
#44873=CARTESIAN_POINT('Ctrl Pts',(-0.202227367447855,0.0123355961269311,
0.00891119198501783));
#44874=CARTESIAN_POINT('Ctrl Pts',(-0.202238171446361,0.0123466906680839,
0.00891114135503747));
#44875=CARTESIAN_POINT('Ctrl Pts',(-0.202262860105077,0.0123698697743196,
0.00890754832784731));
#44876=CARTESIAN_POINT('Ctrl Pts',(-0.202275059499577,0.0123798177466737,
0.00890344762387098));
#44877=CARTESIAN_POINT('Ctrl Pts',(-0.20228416687705,0.012387051170581,
0.00889981733451039));
#44878=CARTESIAN_POINT('Ctrl Pts',(-0.202286920089651,0.0123891504139199,
0.0088987392573964));
#44879=CARTESIAN_POINT('Ctrl Pts',(-0.202289679251312,0.01239118638763,
0.00889757906871427));
#44880=CARTESIAN_POINT('Ctrl Pts',(-0.202290700091811,0.0123919533806702,
0.00889712834741086));
#44881=CARTESIAN_POINT('Ctrl Pts',(-0.202265283386786,0.00221674355360878,
0.0085200608006989));
#44882=CARTESIAN_POINT('Ctrl Pts',(-0.202262903766929,0.00215815693190638,
0.00860438499719491));
#44883=CARTESIAN_POINT('Ctrl Pts',(-0.202364785162833,0.00216892793183714,
0.00861155864805056));
#44884=CARTESIAN_POINT('Ctrl Pts',(-0.202126393174205,0.00304878504751519,
0.0090976895221217));
#44885=CARTESIAN_POINT('Ctrl Pts',(-0.202123767066444,0.00299929247320867,
0.00918838770691312));
#44886=CARTESIAN_POINT('Ctrl Pts',(-0.202225299563324,0.00301370238024901,
0.00919586042731392));
#44887=CARTESIAN_POINT('Ctrl Pts',(-0.201846780434746,0.00493160127209062,
0.00998542514888836));
#44888=CARTESIAN_POINT('Ctrl Pts',(-0.20184379305394,0.00490326887046296,
0.0100860430326691));
#44889=CARTESIAN_POINT('Ctrl Pts',(-0.20194732115168,0.00490316112478149,
0.0100833805366352));
#44890=CARTESIAN_POINT('Ctrl Pts',(-0.202060558052025,0.00700518294088309,
0.0102172780069111));
#44891=CARTESIAN_POINT('Ctrl Pts',(-0.202057443704119,0.00699955579133595,
0.0103204291575386));
#44892=CARTESIAN_POINT('Ctrl Pts',(-0.202159605819829,0.00698941479977137,
0.0103203063255642));
#44893=CARTESIAN_POINT('Ctrl Pts',(-0.202143361846868,0.00802345793181346,
0.0101604293836056));
#44894=CARTESIAN_POINT('Ctrl Pts',(-0.202140271632653,0.00802931137431162,
0.0102629275659062));
#44895=CARTESIAN_POINT('Ctrl Pts',(-0.202242659763401,0.00802100637154811,
0.0102637647012907));
#44896=CARTESIAN_POINT('Ctrl Pts',(-0.202099463949638,0.00749950457486307,
0.0101752294684686));
#44897=CARTESIAN_POINT('Ctrl Pts',(-0.20209931606238,0.00749950424735862,
0.0101817730524425));
#44898=CARTESIAN_POINT('Ctrl Pts',(-0.202099813307759,0.0074995041438527,
0.010188314976911));
#44899=CARTESIAN_POINT('Ctrl Pts',(-0.202102155212527,0.00749950439525637,
0.0102016163950763));
#44900=CARTESIAN_POINT('Ctrl Pts',(-0.202104076840267,0.00749950477897649,
0.0102083261168978));
#44901=CARTESIAN_POINT('Ctrl Pts',(-0.202111500004307,0.00749950657857423,
0.0102267270920281));
#44902=CARTESIAN_POINT('Ctrl Pts',(-0.202118585533017,0.00749950857758533,
0.0102376266605826));
#44903=CARTESIAN_POINT('Ctrl Pts',(-0.202136499996345,0.00749951401374605,
0.0102561492958782));
#44904=CARTESIAN_POINT('Ctrl Pts',(-0.202147162872982,0.00749951740124023,
0.0102635981106341));
#44905=CARTESIAN_POINT('Ctrl Pts',(-0.202175158064661,0.0074995265905247,
0.0102760372628172));
#44906=CARTESIAN_POINT('Ctrl Pts',(-0.202189268457591,0.00749954163844324,
0.0102772369414757));
#44907=CARTESIAN_POINT('Ctrl Pts',(-0.202197037592779,0.00749953297569803,
0.0102774630649767));
#44908=CARTESIAN_POINT('Ctrl Pts',(-0.202197541742858,0.00749953433505264,
0.0102774756030113));
#44909=CARTESIAN_POINT('Ctrl Pts',(-0.202361880888437,0.0128264515031921,
0.0086147092298632));
#44910=CARTESIAN_POINT('Ctrl Pts',(-0.202260113951347,0.0128370847197872,
0.0086074593432484));
#44911=CARTESIAN_POINT('Ctrl Pts',(-0.202262517511821,0.0127786173864275,
0.00852320316472772));
#44912=CARTESIAN_POINT('Ctrl Pts',(-0.202223258922033,0.0119819745234462,
0.00919807175636186));
#44913=CARTESIAN_POINT('Ctrl Pts',(-0.20212183907179,0.0119962328416967,
0.00919051456852261));
#44914=CARTESIAN_POINT('Ctrl Pts',(-0.202124488350021,0.0119468443820253,
0.00909990279227285));
#44915=CARTESIAN_POINT('Ctrl Pts',(-0.201945876329119,0.0100935785167927,
0.010083967214963));
#44916=CARTESIAN_POINT('Ctrl Pts',(-0.201842473337064,0.0100934554540095,
0.0100864724546506));
#44917=CARTESIAN_POINT('Ctrl Pts',(-0.201845483364813,0.0100651943495382,
0.00998596792976334));
#44918=CARTESIAN_POINT('Ctrl Pts',(-0.202159081801773,0.00800919428865958,
0.0103202693714982));
#44919=CARTESIAN_POINT('Ctrl Pts',(-0.202057049752887,0.0079989680904996,
0.0103202497035326));
#44920=CARTESIAN_POINT('Ctrl Pts',(-0.202060185966541,0.00799336645668808,
0.0102172231029901));
#44921=CARTESIAN_POINT('Ctrl Pts',(-0.202242858976565,0.00697850976193525,
0.0102637454365422));
#44922=CARTESIAN_POINT('Ctrl Pts',(-0.202140599979829,0.0069701564498707,
0.0102627551815556));
#44923=CARTESIAN_POINT('Ctrl Pts',(-0.20214371220484,0.0069760105515131,
0.0101603809964741));
#44924=CARTESIAN_POINT('Ctrl Pts',(-0.199153917445656,0.00216330382806559,
0.0085466816420894));
#44925=CARTESIAN_POINT('Ctrl Pts',(-0.199259854338567,0.00216954278467004,
0.00856124395669496));
#44926=CARTESIAN_POINT('Ctrl Pts',(-0.199260840617245,0.00223019704828265,
0.00847296600068187));
#44927=CARTESIAN_POINT('Ctrl Pts',(-0.199014559592398,0.00301082025703676,
0.00912885805490715));
#44928=CARTESIAN_POINT('Ctrl Pts',(-0.199120135788544,0.0030215055052538,
0.0091442300040962));
#44929=CARTESIAN_POINT('Ctrl Pts',(-0.19912137309385,0.00307263960711639,
0.00904934758541328));
#44930=CARTESIAN_POINT('Ctrl Pts',(-0.198742264019069,0.00490687946315208,
0.0100137040478795));
#44931=CARTESIAN_POINT('Ctrl Pts',(-0.198849878408609,0.0049041364027777,
0.0100193895857334));
#44932=CARTESIAN_POINT('Ctrl Pts',(-0.19885152983239,0.00493349699554989,
0.00991444126272149));
#44933=CARTESIAN_POINT('Ctrl Pts',(-0.198952774929459,0.00699674633684083,
0.0102479409536527));
#44934=CARTESIAN_POINT('Ctrl Pts',(-0.199058944563945,0.0069858644231249,
0.0102566134579587));
#44935=CARTESIAN_POINT('Ctrl Pts',(-0.199060696986617,0.00699176666959928,
0.0101490006187123));
#44936=CARTESIAN_POINT('Ctrl Pts',(-0.199035988933059,0.00802971819184572,
0.0101907130089996));
#44937=CARTESIAN_POINT('Ctrl Pts',(-0.199142384098032,0.00802154341492879,
0.0102002834057196));
#44938=CARTESIAN_POINT('Ctrl Pts',(-0.19914411851978,0.00801551120631029,
0.0100933513992024));
#44939=CARTESIAN_POINT('Ctrl Pts',(-0.199090544161673,0.00260012940780254,
0.0088293656616242));
#44940=CARTESIAN_POINT('Ctrl Pts',(-0.19909130728753,0.00260087836723755,
0.00882983779134686));
#44941=CARTESIAN_POINT('Ctrl Pts',(-0.199093469606293,0.00260294996891118,
0.00883111025990233));
#44942=CARTESIAN_POINT('Ctrl Pts',(-0.199095623457249,0.00260508172848499,
0.00883229463920616));
#44943=CARTESIAN_POINT('Ctrl Pts',(-0.199102455445532,0.00261217358753728,
0.00883614138729688));
#44944=CARTESIAN_POINT('Ctrl Pts',(-0.199112010710586,0.00262224476993763,
0.00884079237775844));
#44945=CARTESIAN_POINT('Ctrl Pts',(-0.199131908567056,0.00264633414288908,
0.0088452514389217));
#44946=CARTESIAN_POINT('Ctrl Pts',(-0.199140475861325,0.00265763798807928,
0.0088455461646959));
#44947=CARTESIAN_POINT('Ctrl Pts',(-0.199156834842009,0.00268170883000255,
0.00884177770164222));
#44948=CARTESIAN_POINT('Ctrl Pts',(-0.199163944618197,0.00269374857837251,
0.00883738897005369));
#44949=CARTESIAN_POINT('Ctrl Pts',(-0.199172579209817,0.00271145441669992,
0.0088267017145877));
#44950=CARTESIAN_POINT('Ctrl Pts',(-0.19917526070757,0.002717960405818,
0.00882163297988479));
#44951=CARTESIAN_POINT('Ctrl Pts',(-0.199178733682342,0.00272920614009963,
0.00881018371261812));
#44952=CARTESIAN_POINT('Ctrl Pts',(-0.19917965205846,0.00273394296772727,
0.00880410193455148));
#44953=CARTESIAN_POINT('Ctrl Pts',(-0.19917977849694,0.0027379568580951,
0.00879744706911775));
#44954=CARTESIAN_POINT('Ctrl Pts',(-0.199100846801734,0.00749833347458839,
0.0101077255427978));
#44955=CARTESIAN_POINT('Ctrl Pts',(-0.19909949185117,0.00749832362100577,
0.0101605248182571));
#44956=CARTESIAN_POINT('Ctrl Pts',(-0.199050347020319,0.00749829538362156,
0.0102063461419179));
#44957=CARTESIAN_POINT('Ctrl Pts',(-0.198998259704992,0.00749827421839395,
0.0102051689206332));
#44958=CARTESIAN_POINT('Ctrl Pts',(-0.199252995072792,0.0127774882842919,
0.00849852558719801));
#44959=CARTESIAN_POINT('Ctrl Pts',(-0.199246529899215,0.0127936285615535,
0.00852055158884003));
#44960=CARTESIAN_POINT('Ctrl Pts',(-0.199233543673028,0.0128260486178342,
0.00856479396468572));
#44961=CARTESIAN_POINT('Ctrl Pts',(-0.199178953436479,0.0128388912776996,
0.00857043901569242));
#44962=CARTESIAN_POINT('Ctrl Pts',(-0.199151631540807,0.0128453829053665,
0.00857335780561756));
#44963=CARTESIAN_POINT('Ctrl Pts',(-0.199205485012669,0.0124493328032341,
0.00867900065461348));
#44964=CARTESIAN_POINT('Ctrl Pts',(-0.199198993780824,0.0124644960051388,
0.00870159673323534));
#44965=CARTESIAN_POINT('Ctrl Pts',(-0.199185955212879,0.0124949534657617,
0.00874698419026339));
#44966=CARTESIAN_POINT('Ctrl Pts',(-0.199131314364772,0.0125072036339993,
0.0087532195982415));
#44967=CARTESIAN_POINT('Ctrl Pts',(-0.19910396705067,0.0125133947551101,
0.00875643604575879));
#44968=CARTESIAN_POINT('Ctrl Pts',(-0.199124866985969,0.0119495412903626,
0.00899228522622666));
#44969=CARTESIAN_POINT('Ctrl Pts',(-0.199118343519783,0.0119633083281558,
0.00901582261420499));
#44970=CARTESIAN_POINT('Ctrl Pts',(-0.199105240204551,0.0119909613933932,
0.00906310082576092));
#44971=CARTESIAN_POINT('Ctrl Pts',(-0.199050620029599,0.0120030870736398,
0.00906994918457371));
#44972=CARTESIAN_POINT('Ctrl Pts',(-0.199023282910386,0.0120092098423158,
0.00907347621110877));
#44973=CARTESIAN_POINT('Ctrl Pts',(-0.199007287267715,0.0110303351348565,
0.00942571112218718));
#44974=CARTESIAN_POINT('Ctrl Pts',(-0.199000676818597,0.0110411926535879,
0.00945070822400934));
#44975=CARTESIAN_POINT('Ctrl Pts',(-0.198987398785699,0.0110630015334869,
0.00950091847968093));
#44976=CARTESIAN_POINT('Ctrl Pts',(-0.198932453345222,0.0110720073961954,
0.00950995769117948));
#44977=CARTESIAN_POINT('Ctrl Pts',(-0.198904953221552,0.0110765576063949,
0.00951458647297514));
#44978=CARTESIAN_POINT('Ctrl Pts',(-0.198950876441888,0.0100226308845471,
0.00978597479287774));
#44979=CARTESIAN_POINT('Ctrl Pts',(-0.198944192313863,0.0100300028344982,
0.00981225272852039));
#44980=CARTESIAN_POINT('Ctrl Pts',(-0.198930766286339,0.0100448104507761,
0.00986503572218605));
#44981=CARTESIAN_POINT('Ctrl Pts',(-0.198875537616916,0.0100481896171548,
0.0098763822509411));
#44982=CARTESIAN_POINT('Ctrl Pts',(-0.198847895564142,0.0100499113777636,
0.00988217023395557));
#44983=CARTESIAN_POINT('Ctrl Pts',(-0.198986795866928,0.00896522208316481,
0.0100034584399927));
#44984=CARTESIAN_POINT('Ctrl Pts',(-0.198980105148717,0.0089691562897449,
0.0100303985815119));
#44985=CARTESIAN_POINT('Ctrl Pts',(-0.198966665883862,0.00897705870657931,
0.0100845117104313));
#44986=CARTESIAN_POINT('Ctrl Pts',(-0.198911580935987,0.00897588131856843,
0.0100964358107904));
#44987=CARTESIAN_POINT('Ctrl Pts',(-0.198884010711124,0.00897530988002672,
0.0101025154623784));
#44988=CARTESIAN_POINT('Ctrl Pts',(-0.199060893012184,0.00795492981715577,
0.0101109376831195));
#44989=CARTESIAN_POINT('Ctrl Pts',(-0.19905420386632,0.00795573250050825,
0.0101381519892747));
#44990=CARTESIAN_POINT('Ctrl Pts',(-0.199040767759749,0.00795734480487209,
0.0101928158170936));
#44991=CARTESIAN_POINT('Ctrl Pts',(-0.198985794732566,0.00795325937128545,
0.0102045659851305));
#44992=CARTESIAN_POINT('Ctrl Pts',(-0.198958280471805,0.00795122028247677,
0.0102105598756125));
#44993=CARTESIAN_POINT('Ctrl Pts',(-0.199112792949338,0.00736427983216101,
0.0101030859175174));
#44994=CARTESIAN_POINT('Ctrl Pts',(-0.199106105446657,0.00736333742444203,
0.0101302344227966));
#44995=CARTESIAN_POINT('Ctrl Pts',(-0.199092672640656,0.00736144446369592,
0.0101847660801409));
#44996=CARTESIAN_POINT('Ctrl Pts',(-0.199037705857924,0.00735661611559613,
0.0101961630417089));
#44997=CARTESIAN_POINT('Ctrl Pts',(-0.199010194726408,0.00735419795088647,
0.0102019800507694));
#44998=CARTESIAN_POINT('Ctrl Pts',(-0.199143042960716,0.00699123828422424,
0.0101189604526251));
#44999=CARTESIAN_POINT('Ctrl Pts',(-0.199136356282475,0.0069891684572404,
0.0101461340332429));
#45000=CARTESIAN_POINT('Ctrl Pts',(-0.199122925132461,0.00698501091358601,
0.0102007160579938));
#45001=CARTESIAN_POINT('Ctrl Pts',(-0.199067979737894,0.00697943123747824,
0.0102119640717528));
#45002=CARTESIAN_POINT('Ctrl Pts',(-0.199040479303471,0.00697663249430555,
0.0102177067208405));
#45003=CARTESIAN_POINT('Ctrl Pts',(-0.199174846040548,0.0122573379664025,
0.00879984889793131));
#45004=CARTESIAN_POINT('Ctrl Pts',(-0.199174163106151,0.0122823816012495,
0.00884168590479541));
#45005=CARTESIAN_POINT('Ctrl Pts',(-0.199137777220614,0.0123252893097993,
0.00885359374849819));
#45006=CARTESIAN_POINT('Ctrl Pts',(-0.19910812755215,0.0123635456293657,
0.00884505562956225));
#45007=CARTESIAN_POINT('Ctrl Pts',(-0.199099738487824,0.0123743698558192,
0.00884263985789638));
#45008=CARTESIAN_POINT('Ctrl Pts',(-0.199091892717798,0.0123851046964944,
0.00883840677396556));
#45009=CARTESIAN_POINT('Ctrl Pts',(-0.19908556181331,0.0123952967315942,
0.00883206936057618));
#45010=CARTESIAN_POINT('Origin',(-0.20034316899928,0.00265361948026404,
0.00876944888039472));
#45011=CARTESIAN_POINT('Ctrl Pts',(-0.200180138467595,0.00273845005850156,
0.00881880524816497));
#45012=CARTESIAN_POINT('Ctrl Pts',(-0.200180111069365,0.0027343534632471,
0.0088254195296896));
#45013=CARTESIAN_POINT('Ctrl Pts',(-0.20018111626804,0.00272956660640373,
0.00883144775892295));
#45014=CARTESIAN_POINT('Ctrl Pts',(-0.200185329611713,0.00271789323850519,
0.00884324632224045));
#45015=CARTESIAN_POINT('Ctrl Pts',(-0.200188854916373,0.00271098217482735,
0.00884853338008211));
#45016=CARTESIAN_POINT('Ctrl Pts',(-0.200200021494589,0.00269272660018771,
0.00885943065655154));
#45017=CARTESIAN_POINT('Ctrl Pts',(-0.200209291703764,0.00268040388413873,
0.00886391870869385));
#45018=CARTESIAN_POINT('Ctrl Pts',(-0.200230849539644,0.00265577661479843,
0.00886787204504395));
#45019=CARTESIAN_POINT('Ctrl Pts',(-0.200242201866841,0.00264427919255049,
0.00886758640057448));
#45020=CARTESIAN_POINT('Ctrl Pts',(-0.200270784471942,0.00261789598308321,
0.00886279510022952));
#45021=CARTESIAN_POINT('Ctrl Pts',(-0.20028469313402,0.00260716979711846,
0.00885693527935284));
#45022=CARTESIAN_POINT('Ctrl Pts',(-0.200289538153472,0.00260376631764392,
0.00885509819941641));
#45023=CARTESIAN_POINT('Ctrl Pts',(-0.200290353810089,0.00260302859526534,
0.00885467958226884));
#45024=CARTESIAN_POINT('Ctrl Pts',(-0.200291448570889,0.0026020425860909,
0.00885411375756756));
#45025=CARTESIAN_POINT('Ctrl Pts',(-0.200292333969178,0.00260137683365692,
0.00885372371479089));
#45026=CARTESIAN_POINT('Origin',(-0.199015160118143,0.0123433413565343,
0.00874522744837511));
#45027=CARTESIAN_POINT('Ctrl Pts',(-0.200176391911418,0.0122568678944164,
0.00882151754982349));
#45028=CARTESIAN_POINT('Ctrl Pts',(-0.20017636446585,0.0122608604306115,
0.00882797128920379));
#45029=CARTESIAN_POINT('Ctrl Pts',(-0.200177318434311,0.0122655116038751,
0.00883387049142189));
#45030=CARTESIAN_POINT('Ctrl Pts',(-0.200181324848676,0.0122768299522418,
0.00884544598348673));
#45031=CARTESIAN_POINT('Ctrl Pts',(-0.200184676853031,0.0122835225431615,
0.00885066860115435));
#45032=CARTESIAN_POINT('Ctrl Pts',(-0.200195420287465,0.012301379346308,
0.00886161958207752));
#45033=CARTESIAN_POINT('Ctrl Pts',(-0.200204430514006,0.0123135167776523,
0.00886623133374718));
#45034=CARTESIAN_POINT('Ctrl Pts',(-0.200225204203302,0.0123375397346441,
0.00887047629071223));
#45035=CARTESIAN_POINT('Ctrl Pts',(-0.200235993979062,0.0123486318822383,
0.00887044874845416));
#45036=CARTESIAN_POINT('Ctrl Pts',(-0.200260725447184,0.0123718830794046,
0.00886689271441571));
#45037=CARTESIAN_POINT('Ctrl Pts',(-0.200272949041827,0.0123818561551207,
0.00886277886901737));
#45038=CARTESIAN_POINT('Ctrl Pts',(-0.200281908067139,0.012388990717191,
0.00885921502571013));
#45039=CARTESIAN_POINT('Ctrl Pts',(-0.200284679859229,0.0123911072988095,
0.00885813444516822));
#45040=CARTESIAN_POINT('Ctrl Pts',(-0.200287457775747,0.0123931591103749,
0.00885696952162079));
#45041=CARTESIAN_POINT('Ctrl Pts',(-0.200288454700047,0.0123939097369423,
0.00885653037079223));
#45042=CARTESIAN_POINT('Ctrl Pts',(-0.200264179876147,0.00221381594909614,
0.00848015784889415));
#45043=CARTESIAN_POINT('Ctrl Pts',(-0.20026179025018,0.00215534095857477,
0.00856470365446266));
#45044=CARTESIAN_POINT('Ctrl Pts',(-0.200363797814067,0.00216614310006481,
0.00857172965097436));
#45045=CARTESIAN_POINT('Ctrl Pts',(-0.200125957436327,0.00304715701388984,
0.00905604306368936));
#45046=CARTESIAN_POINT('Ctrl Pts',(-0.200123320123447,0.00299777112378732,
0.00914692946592738));
#45047=CARTESIAN_POINT('Ctrl Pts',(-0.200224981899174,0.00301219654003019,
0.0091542509252648));
#45048=CARTESIAN_POINT('Ctrl Pts',(-0.199848200870376,0.00493136048449093,
0.00994083078053965));
#45049=CARTESIAN_POINT('Ctrl Pts',(-0.199845199746795,0.00490309257337129,
0.0100415783091978));
#45050=CARTESIAN_POINT('Ctrl Pts',(-0.199948841338395,0.00490294139784739,
0.0100388091649515));
#45051=CARTESIAN_POINT('Ctrl Pts',(-0.200061558378191,0.00700447670195284,
0.0101718827938119));
#45052=CARTESIAN_POINT('Ctrl Pts',(-0.200058430539336,0.00699885912125533,
0.0102751489227272));
#45053=CARTESIAN_POINT('Ctrl Pts',(-0.200160714440828,0.00698875414792091,
0.0102749221532313));
#45054=CARTESIAN_POINT('Ctrl Pts',(-0.200144088013061,0.00802290026385727,
0.0101153280660965));
#45055=CARTESIAN_POINT('Ctrl Pts',(-0.200140984359156,0.0080287326218905,
0.0102179459412791));
#45056=CARTESIAN_POINT('Ctrl Pts',(-0.200243492857047,0.00802043167606583,
0.0102186707749455));
#45057=CARTESIAN_POINT('Ctrl Pts',(-0.200100323214919,0.00749890966891628,
0.0101300471986839));
#45058=CARTESIAN_POINT('Ctrl Pts',(-0.200100175329577,0.0074989089326428,
0.0101365907504349));
#45059=CARTESIAN_POINT('Ctrl Pts',(-0.20010067256581,0.00749890851664256,
0.0101431326434737));
#45060=CARTESIAN_POINT('Ctrl Pts',(-0.200103014429842,0.00749890833111619,
0.0101564339958254));
#45061=CARTESIAN_POINT('Ctrl Pts',(-0.200104936024074,0.00749890860481728,
0.010163143686125));
#45062=CARTESIAN_POINT('Ctrl Pts',(-0.200112359078578,0.00749891042409756,
0.0101815446193971));
#45063=CARTESIAN_POINT('Ctrl Pts',(-0.200119444524665,0.0074989128359811,
0.0101924441940189));
#45064=CARTESIAN_POINT('Ctrl Pts',(-0.200137358813104,0.00749891985374453,
0.0102109668500448));
#45065=CARTESIAN_POINT('Ctrl Pts',(-0.200148021593063,0.00749892439464753,
0.0102184156855726));
#45066=CARTESIAN_POINT('Ctrl Pts',(-0.200175045045713,0.00749893661254169,
0.0102304232056775));
#45067=CARTESIAN_POINT('Ctrl Pts',(-0.200188714108781,0.00749893573954711,
0.0102320135358485));
#45068=CARTESIAN_POINT('Ctrl Pts',(-0.200197940246902,0.00749894856295794,
0.0102322820181257));
#45069=CARTESIAN_POINT('Ctrl Pts',(-0.200198400285571,0.00749894802607654,
0.0102322932741428));
#45070=CARTESIAN_POINT('Ctrl Pts',(-0.20035891519497,0.012829115342383,
0.00857491507414323));
#45071=CARTESIAN_POINT('Ctrl Pts',(-0.20025717573531,0.0128396259952154,
0.00856772156231838));
#45072=CARTESIAN_POINT('Ctrl Pts',(-0.200259586169385,0.0127813643735082,
0.00848337674133248));
#45073=CARTESIAN_POINT('Ctrl Pts',(-0.200221630466784,0.0119831507262477,
0.00915663829108513));
#45074=CARTESIAN_POINT('Ctrl Pts',(-0.200120232456941,0.0119972551590367,
0.00914913325111272));
#45075=CARTESIAN_POINT('Ctrl Pts',(-0.200122889507142,0.0119480558515039,
0.00905847473897322));
#45076=CARTESIAN_POINT('Ctrl Pts',(-0.199946820616977,0.0100930042470462,
0.0100396703535222));
#45077=CARTESIAN_POINT('Ctrl Pts',(-0.199843471700871,0.0100928272432444,
0.0100421051316997));
#45078=CARTESIAN_POINT('Ctrl Pts',(-0.199846491720836,0.0100646842389006,
0.00994162695940243));
#45079=CARTESIAN_POINT('Ctrl Pts',(-0.200159800951594,0.00800872160038045,
0.0102749558378368));
#45080=CARTESIAN_POINT('Ctrl Pts',(-0.200057812077642,0.00799849597590558,
0.0102748799873785));
#45081=CARTESIAN_POINT('Ctrl Pts',(-0.20006095755435,0.00799292564384356,
0.0101719009533559));
#45082=CARTESIAN_POINT('Ctrl Pts',(-0.200243718387518,0.00697783487179026,
0.0102185848089423));
#45083=CARTESIAN_POINT('Ctrl Pts',(-0.200141504405587,0.00696947970956505,
0.0102175413210191));
#45084=CARTESIAN_POINT('Ctrl Pts',(-0.200144625882982,0.00697531736293823,
0.0101152105196031));
#45085=CARTESIAN_POINT('Ctrl Pts',(-0.197152652670088,0.0021605811934014,
0.00850709261495718));
#45086=CARTESIAN_POINT('Ctrl Pts',(-0.197258645563439,0.00216678404947317,
0.00852161638163525));
#45087=CARTESIAN_POINT('Ctrl Pts',(-0.197259599012086,0.00222726834004635,
0.00843316287831881));
#45088=CARTESIAN_POINT('Ctrl Pts',(-0.197014009033787,0.00300933269914294,
0.00908736405676043));
#45089=CARTESIAN_POINT('Ctrl Pts',(-0.197119643888281,0.00301997324048751,
0.00910269918253681));
#45090=CARTESIAN_POINT('Ctrl Pts',(-0.197120849704256,0.00307094934136566,
0.00900768228901369));
#45091=CARTESIAN_POINT('Ctrl Pts',(-0.196743444704333,0.00490654029458651,
0.009969069964755));
#45092=CARTESIAN_POINT('Ctrl Pts',(-0.196851099911388,0.00490373400048392,
0.00997478148765791));
#45093=CARTESIAN_POINT('Ctrl Pts',(-0.196852720516954,0.00493300694734234,
0.00986977292339073));
#45094=CARTESIAN_POINT('Ctrl Pts',(-0.196953821593501,0.00699572957181629,
0.0102025186563745));
#45095=CARTESIAN_POINT('Ctrl Pts',(-0.197060039270723,0.0069848622369541,
0.0102112148095307));
#45096=CARTESIAN_POINT('Ctrl Pts',(-0.197061761627991,0.00699075765333439,
0.0101035576162893));
#45097=CARTESIAN_POINT('Ctrl Pts',(-0.197036936888857,0.00802867877765998,
0.0101456529653734));
#45098=CARTESIAN_POINT('Ctrl Pts',(-0.197143379084148,0.00802050281413876,
0.0101552409857996));
#45099=CARTESIAN_POINT('Ctrl Pts',(-0.197145083256844,0.00801450629794631,
0.0100482580482319));
#45100=CARTESIAN_POINT('Ctrl Pts',(-0.19708966640812,0.00259797400119342,
0.00878884298022014));
#45101=CARTESIAN_POINT('Ctrl Pts',(-0.197090422962005,0.00259871688481011,
0.00878930919013162));
#45102=CARTESIAN_POINT('Ctrl Pts',(-0.197092594086397,0.00260079696505936,
0.00879058153882454));
#45103=CARTESIAN_POINT('Ctrl Pts',(-0.197094756701536,0.00260293768788332,
0.00879176480312747));
#45104=CARTESIAN_POINT('Ctrl Pts',(-0.197101550058633,0.00260999384516736,
0.00879557393678802));
#45105=CARTESIAN_POINT('Ctrl Pts',(-0.197111121274289,0.00262007842499146,
0.00880021806540418));
#45106=CARTESIAN_POINT('Ctrl Pts',(-0.197131056914606,0.00264420422969141,
0.0088046346515727));
#45107=CARTESIAN_POINT('Ctrl Pts',(-0.197139629688112,0.00265550717491842,
0.00880490734767921));
#45108=CARTESIAN_POINT('Ctrl Pts',(-0.197156000870632,0.00267956982940497,
0.00880109254121348));
#45109=CARTESIAN_POINT('Ctrl Pts',(-0.197163116330695,0.00269160121674832,
0.00879668045913739));
#45110=CARTESIAN_POINT('Ctrl Pts',(-0.197171758146352,0.00270928700228767,
0.00878595857646887));
#45111=CARTESIAN_POINT('Ctrl Pts',(-0.197174442130602,0.00271578394302307,
0.00878087664097018));
#45112=CARTESIAN_POINT('Ctrl Pts',(-0.197177918132516,0.00272700868139428,
0.00876940382769687));
#45113=CARTESIAN_POINT('Ctrl Pts',(-0.197178837227364,0.00273173408342081,
0.00876331200781784));
#45114=CARTESIAN_POINT('Ctrl Pts',(-0.197178963584415,0.00273573528602628,
0.00875664828842276));
#45115=CARTESIAN_POINT('Ctrl Pts',(-0.197101855005559,0.00749734545555895,
0.0100625711568172));
#45116=CARTESIAN_POINT('Ctrl Pts',(-0.197101690442853,0.00749734357232736,
0.0100690161322291));
#45117=CARTESIAN_POINT('Ctrl Pts',(-0.197100900765169,0.00749734148888539,
0.0100754298692072));
#45118=CARTESIAN_POINT('Ctrl Pts',(-0.197097981899033,0.00749733679991958,
0.0100885161664239));
#45119=CARTESIAN_POINT('Ctrl Pts',(-0.197095759406202,0.00749733417927401,
0.0100951318714899));
#45120=CARTESIAN_POINT('Ctrl Pts',(-0.197087513364756,0.00749732629771051,
0.0101131783932643));
#45121=CARTESIAN_POINT('Ctrl Pts',(-0.197079943180104,0.00749732076252694,
0.0101237468493541));
#45122=CARTESIAN_POINT('Ctrl Pts',(-0.197061211216097,0.00749730944906349,
0.0101414416276148));
#45123=CARTESIAN_POINT('Ctrl Pts',(-0.197050223203192,0.00749730378248083,
0.0101484013861565));
#45124=CARTESIAN_POINT('Ctrl Pts',(-0.197018046539333,0.0074972892795021,
0.0101609916103687));
#45125=CARTESIAN_POINT('Ctrl Pts',(-0.197001302675901,0.00749729577011255,
0.0101600246187684));
#45126=CARTESIAN_POINT('Ctrl Pts',(-0.19699971712443,0.00749726941310258,
0.0101599992595542));
#45127=CARTESIAN_POINT('Ctrl Pts',(-0.196999275842678,0.00749728354040296,
0.0101599900590452));
#45128=CARTESIAN_POINT('Ctrl Pts',(-0.197256820089405,0.0127679866759842,
0.00843621590655516));
#45129=CARTESIAN_POINT('Ctrl Pts',(-0.197255983919717,0.0128285304405105,
0.00852489944995749));
#45130=CARTESIAN_POINT('Ctrl Pts',(-0.197149776203591,0.0128346755026245,
0.00851027926216887));
#45131=CARTESIAN_POINT('Ctrl Pts',(-0.197118253662537,0.0119239787910673,
0.00901021072020725));
#45132=CARTESIAN_POINT('Ctrl Pts',(-0.197117164455696,0.0119749872889838,
0.0091054653969711));
#45133=CARTESIAN_POINT('Ctrl Pts',(-0.197011315898106,0.0119856063978868,
0.00909002022551536));
#45134=CARTESIAN_POINT('Ctrl Pts',(-0.196850600591309,0.0100615170300595,
0.00987110312810501));
#45135=CARTESIAN_POINT('Ctrl Pts',(-0.196849098706584,0.0100907877610896,
0.00997634525975825));
#45136=CARTESIAN_POINT('Ctrl Pts',(-0.196741224795717,0.0100878459637636,
0.00997055758727937));
#45137=CARTESIAN_POINT('Ctrl Pts',(-0.197061500370654,0.00800384808569401,
0.0101037236165437));
#45138=CARTESIAN_POINT('Ctrl Pts',(-0.19705989562741,0.00800970369698869,
0.0102116092393013));
#45139=CARTESIAN_POINT('Ctrl Pts',(-0.196953473326002,0.00799874894913888,
0.0102027890447947));
#45140=CARTESIAN_POINT('Ctrl Pts',(-0.197145405828628,0.00698025475593223,
0.0100478570432307));
#45141=CARTESIAN_POINT('Ctrl Pts',(-0.197143819563754,0.00697419554098605,
0.0101550610895007));
#45142=CARTESIAN_POINT('Ctrl Pts',(-0.197037170579532,0.00696594143372946,
0.0101453456903674));
#45143=CARTESIAN_POINT('Ctrl Pts',(-0.197176298810346,0.0122593881381477,
0.00875948681888613));
#45144=CARTESIAN_POINT('Ctrl Pts',(-0.197176176439832,0.0122632507361322,
0.0087659306057829));
#45145=CARTESIAN_POINT('Ctrl Pts',(-0.197175313201552,0.0122677917440443,
0.00877184319222938));
#45146=CARTESIAN_POINT('Ctrl Pts',(-0.197172053774191,0.0122785410350562,
0.00878301774032121));
#45147=CARTESIAN_POINT('Ctrl Pts',(-0.197169541543235,0.0122847481433668,
0.0087880082107202));
#45148=CARTESIAN_POINT('Ctrl Pts',(-0.197161307159831,0.0123019228673441,
0.00879882601323132));
#45149=CARTESIAN_POINT('Ctrl Pts',(-0.197154411747571,0.0123137493536575,
0.00880341874342543));
#45150=CARTESIAN_POINT('Ctrl Pts',(-0.197137656856923,0.0123386748828606,
0.00880790236212758));
#45151=CARTESIAN_POINT('Ctrl Pts',(-0.197128297243567,0.0123510214261447,
0.00880764252441401));
#45152=CARTESIAN_POINT('Ctrl Pts',(-0.197104538659764,0.0123795609881269,
0.00880212446974175));
#45153=CARTESIAN_POINT('Ctrl Pts',(-0.197093039129748,0.0123911488545319,
0.00879532119320332));
#45154=CARTESIAN_POINT('Ctrl Pts',(-0.197089059974131,0.0123947079343662,
0.00879324060162505));
#45155=CARTESIAN_POINT('Ctrl Pts',(-0.19708846547414,0.012395450350782,
0.00879279541010521));
#45156=CARTESIAN_POINT('Ctrl Pts',(-0.197087666832481,0.0123964431722424,
0.00879219355122506));
#45157=CARTESIAN_POINT('Ctrl Pts',(-0.19708698285431,0.0123971147297022,
0.00879177268117346));
#45158=CARTESIAN_POINT('Origin',(-0.198342348487265,0.00265133456699769,
0.00872878636643693));
#45159=CARTESIAN_POINT('Ctrl Pts',(-0.198179411628685,0.00273625916616763,
0.00877798858090942));
#45160=CARTESIAN_POINT('Ctrl Pts',(-0.19817938500885,0.00273217717639081,
0.0087846072054196));
#45161=CARTESIAN_POINT('Ctrl Pts',(-0.198180389211287,0.00272740441884125,
0.00879064180724154));
#45162=CARTESIAN_POINT('Ctrl Pts',(-0.198184597990081,0.00271575815394672,
0.00880245994552571));
#45163=CARTESIAN_POINT('Ctrl Pts',(-0.19818811996947,0.00270885869545007,
0.00880776021054462));
#45164=CARTESIAN_POINT('Ctrl Pts',(-0.198199277211723,0.00269062642511689,
0.00881869335267521));
#45165=CARTESIAN_POINT('Ctrl Pts',(-0.198208539838762,0.00267831376926954,
0.00882320585945375));
#45166=CARTESIAN_POINT('Ctrl Pts',(-0.198230164370323,0.00265360052534109,
0.00882722432949729));
#45167=CARTESIAN_POINT('Ctrl Pts',(-0.198241608709373,0.00264201182077982,
0.00882694238263359));
#45168=CARTESIAN_POINT('Ctrl Pts',(-0.198270526973544,0.00261533210442332,
0.0088220795568075));
#45169=CARTESIAN_POINT('Ctrl Pts',(-0.19828458157657,0.00260448296114289,
0.00881606909428004));
#45170=CARTESIAN_POINT('Ctrl Pts',(-0.198289191848955,0.00260135615922656,
0.00881437505335988));
#45171=CARTESIAN_POINT('Ctrl Pts',(-0.198289866723518,0.00260070421971694,
0.00881400226185802));
#45172=CARTESIAN_POINT('Ctrl Pts',(-0.198290773684868,0.00259983144512114,
0.00881349978351456));
#45173=CARTESIAN_POINT('Ctrl Pts',(-0.198291531830531,0.00259926033540328,
0.00881316668848207));
#45174=CARTESIAN_POINT('Origin',(-0.197012620205462,0.0123453294618211,
0.00870476452362944));
#45175=CARTESIAN_POINT('Ctrl Pts',(-0.198174121550572,0.0122590158781096,
0.00878068088066938));
#45176=CARTESIAN_POINT('Ctrl Pts',(-0.198174094633242,0.012262978212402,
0.0087871132810639));
#45177=CARTESIAN_POINT('Ctrl Pts',(-0.198175038857425,0.0122675950228917,
0.00879299782819372));
#45178=CARTESIAN_POINT('Ctrl Pts',(-0.198179006095641,0.0122788340702126,
0.00880455626725186));
#45179=CARTESIAN_POINT('Ctrl Pts',(-0.198182326296455,0.0122854833920715,
0.00880978080657457));
#45180=CARTESIAN_POINT('Ctrl Pts',(-0.198192988871284,0.0123032595928686,
0.00882077167374966));
#45181=CARTESIAN_POINT('Ctrl Pts',(-0.198201945539821,0.0123153606316044,
0.00882542376076332));
#45182=CARTESIAN_POINT('Ctrl Pts',(-0.198222665756589,0.0123393976026421,
0.00882977557378687));
#45183=CARTESIAN_POINT('Ctrl Pts',(-0.198233470933688,0.0123505370415491,
0.00882978651421305));
#45184=CARTESIAN_POINT('Ctrl Pts',(-0.198258231999181,0.0123738810923607,
0.00882628789418516));
#45185=CARTESIAN_POINT('Ctrl Pts',(-0.19827047719199,0.0123839022446484,
0.00882218439658351));
#45186=CARTESIAN_POINT('Ctrl Pts',(-0.198279479382352,0.0123910906192307,
0.00881861094792741));
#45187=CARTESIAN_POINT('Ctrl Pts',(-0.198282242019807,0.0123932064780831,
0.00881753555986399));
#45188=CARTESIAN_POINT('Ctrl Pts',(-0.198285010804024,0.0123952581516283,
0.00881637615689229));
#45189=CARTESIAN_POINT('Ctrl Pts',(-0.198286011292521,0.0123960137502511,
0.00881593605607644));
#45190=CARTESIAN_POINT('Ctrl Pts',(-0.198263015582683,0.00221100833647082,
0.00844046058749481));
#45191=CARTESIAN_POINT('Ctrl Pts',(-0.198260617033187,0.00215267264060678,
0.00852519920881164));
#45192=CARTESIAN_POINT('Ctrl Pts',(-0.198362711813689,0.00216348282904155,
0.00853210786931248));
#45193=CARTESIAN_POINT('Ctrl Pts',(-0.198125466898689,0.00304557461821688,
0.00901447908689848));
#45194=CARTESIAN_POINT('Ctrl Pts',(-0.198122819594458,0.00299631796672872,
0.00910552077863998));
#45195=CARTESIAN_POINT('Ctrl Pts',(-0.198224571337662,0.00301073675780382,
0.00911272370854456));
#45196=CARTESIAN_POINT('Ctrl Pts',(-0.197849391405799,0.00493093979824749,
0.00989615351262796));
#45197=CARTESIAN_POINT('Ctrl Pts',(-0.197846378014324,0.00490274745865633,
0.00999699175877014));
#45198=CARTESIAN_POINT('Ctrl Pts',(-0.197950095003213,0.00490255268693708,
0.00999415547963392));
#45199=CARTESIAN_POINT('Ctrl Pts',(-0.198062615765221,0.00700335854996127,
0.0101264491950313));
#45200=CARTESIAN_POINT('Ctrl Pts',(-0.198059475798075,0.00699774833958211,
0.0102297907905905));
#45201=CARTESIAN_POINT('Ctrl Pts',(-0.198161840565047,0.00698765712520676,
0.0102294964296498));
#45202=CARTESIAN_POINT('Ctrl Pts',(-0.198145063363228,0.00802177486531964,
0.01007026479514));
#45203=CARTESIAN_POINT('Ctrl Pts',(-0.198141947620127,0.00802757715642436,
0.0101729638783758));
#45204=CARTESIAN_POINT('Ctrl Pts',(-0.198244536051857,0.00801926856690324,
0.0101736154882906));
#45205=CARTESIAN_POINT('Ctrl Pts',(-0.198101337934465,0.00749782688006727,
0.0100848682832439));
#45206=CARTESIAN_POINT('Ctrl Pts',(-0.198101190049774,0.00749782537457631,
0.010091411792284));
#45207=CARTESIAN_POINT('Ctrl Pts',(-0.198101687271057,0.00749782413947803,
0.0100979536440257));
#45208=CARTESIAN_POINT('Ctrl Pts',(-0.198104029073436,0.0074978221853558,
0.0101112549096639));
#45209=CARTESIAN_POINT('Ctrl Pts',(-0.198105950618229,0.00749782150952789,
0.0101179645588641));
#45210=CARTESIAN_POINT('Ctrl Pts',(-0.198113373509982,0.00749782055821905,
0.0101363654365789));
#45211=CARTESIAN_POINT('Ctrl Pts',(-0.198120458831957,0.0074978211208926,
0.0101472650224001));
#45212=CARTESIAN_POINT('Ctrl Pts',(-0.198138372856713,0.00749782454491441,
0.0101657877107848));
#45213=CARTESIAN_POINT('Ctrl Pts',(-0.19814903548975,0.00749782737340509,
0.0101732365777307));
#45214=CARTESIAN_POINT('Ctrl Pts',(-0.198172666729056,0.00749783500127251,
0.0101837369998498));
#45215=CARTESIAN_POINT('Ctrl Pts',(-0.198185793394253,0.0074977794521,0.0101867201386191));
#45216=CARTESIAN_POINT('Ctrl Pts',(-0.198198977094684,0.00749784953224362,
0.010187103726467));
#45217=CARTESIAN_POINT('Ctrl Pts',(-0.19819941389096,0.00749784541675471,
0.0101871143080195));
#45218=CARTESIAN_POINT('Ctrl Pts',(-0.198355693142376,0.0128319883322708,
0.0085350931304057));
#45219=CARTESIAN_POINT('Ctrl Pts',(-0.198253902786949,0.0128424016903643,
0.00852802812650304));
#45220=CARTESIAN_POINT('Ctrl Pts',(-0.198256323072633,0.0127843040832604,
0.00844353196650278));
#45221=CARTESIAN_POINT('Ctrl Pts',(-0.198219976457811,0.0119843975857885,
0.00911525593693403));
#45222=CARTESIAN_POINT('Ctrl Pts',(-0.198118520413737,0.0119983691518567,
0.00910787819325317));
#45223=CARTESIAN_POINT('Ctrl Pts',(-0.198121188461898,0.0119493251148045,
0.00901710497314409));
#45224=CARTESIAN_POINT('Ctrl Pts',(-0.197948583145872,0.0100922420607575,
0.00999549380886804));
#45225=CARTESIAN_POINT('Ctrl Pts',(-0.197845215243418,0.0100919920353229,
0.00999793656072922));
#45226=CARTESIAN_POINT('Ctrl Pts',(-0.197848249040959,0.0100639502008642,
0.00989740899395634));
#45227=CARTESIAN_POINT('Ctrl Pts',(-0.198160910579588,0.00800779606522802,
0.0102296858131739));
#45228=CARTESIAN_POINT('Ctrl Pts',(-0.19805888569194,0.00799760825584394,
0.0102296242114142));
#45229=CARTESIAN_POINT('Ctrl Pts',(-0.198062044056392,0.0079920701657748,
0.0101266163930227));
#45230=CARTESIAN_POINT('Ctrl Pts',(-0.198244657667604,0.00697658890091374,
0.0101733935029984));
#45231=CARTESIAN_POINT('Ctrl Pts',(-0.198142410611714,0.00696824631768505,
0.0101723721389504));
#45232=CARTESIAN_POINT('Ctrl Pts',(-0.198145544916776,0.00697407769767305,
0.0100700094381033));
#45233=CARTESIAN_POINT('Ctrl Pts',(-0.195151474094836,0.0021581839665313,
0.00846785476566089));
#45234=CARTESIAN_POINT('Ctrl Pts',(-0.19525748673727,0.00216438162946169,
0.00848230606819899));
#45235=CARTESIAN_POINT('Ctrl Pts',(-0.19525840470211,0.00222466604303826,
0.00839370419046678));
#45236=CARTESIAN_POINT('Ctrl Pts',(-0.195013516634162,0.00300817193503215,
0.00904611630303382));
#45237=CARTESIAN_POINT('Ctrl Pts',(-0.195119173493743,0.00301878746404222,
0.00906137595421988));
#45238=CARTESIAN_POINT('Ctrl Pts',(-0.195120345017048,0.00306957996306731,
0.00896625564857248));
#45239=CARTESIAN_POINT('Ctrl Pts',(-0.194744239513626,0.00490645046054183,
0.00992449906340472));
#45240=CARTESIAN_POINT('Ctrl Pts',(-0.194851902096146,0.00490363285336936,
0.00993020117251484));
#45241=CARTESIAN_POINT('Ctrl Pts',(-0.194853488851879,0.00493280240147255,
0.00982516951400271));
#45242=CARTESIAN_POINT('Ctrl Pts',(-0.194954744898083,0.00699491874387549,
0.0101570965807732));
#45243=CARTESIAN_POINT('Ctrl Pts',(-0.195060972979,0.00698403600339864,
0.0101657685812465));
#45244=CARTESIAN_POINT('Ctrl Pts',(-0.195062662204119,0.00698991992030242,
0.0100581059040497));
#45245=CARTESIAN_POINT('Ctrl Pts',(-0.195038044064419,0.00802772507301438,
0.0101005930890543));
#45246=CARTESIAN_POINT('Ctrl Pts',(-0.195144496335863,0.00801952667954973,
0.0101101565321198));
#45247=CARTESIAN_POINT('Ctrl Pts',(-0.195146167232292,0.0080135677939633,
0.0100031613552704));
#45248=CARTESIAN_POINT('Ctrl Pts',(-0.195088807996151,0.00259613933341528,
0.00874861478558778));
#45249=CARTESIAN_POINT('Ctrl Pts',(-0.195089568324798,0.00259688621242362,
0.00874908133152229));
#45250=CARTESIAN_POINT('Ctrl Pts',(-0.195091737536302,0.00259896565877408,
0.00875034712361913));
#45251=CARTESIAN_POINT('Ctrl Pts',(-0.195093898259448,0.00260110526380068,
0.00875152411652745));
#45252=CARTESIAN_POINT('Ctrl Pts',(-0.195100715212568,0.00260818642304804,
0.00875532749998801));
#45253=CARTESIAN_POINT('Ctrl Pts',(-0.195110287808044,0.00261827529366409,
0.00875994272695168));
#45254=CARTESIAN_POINT('Ctrl Pts',(-0.195130224176016,0.00264239001717091,
0.00876430394263768));
#45255=CARTESIAN_POINT('Ctrl Pts',(-0.195138802238907,0.00265369079223031,
0.00876455232971158));
#45256=CARTESIAN_POINT('Ctrl Pts',(-0.1951551844026,0.00267774154735868,
0.00876068640337326));
#45257=CARTESIAN_POINT('Ctrl Pts',(-0.195162304784493,0.00268976245709861,
0.00875624883714372));
#45258=CARTESIAN_POINT('Ctrl Pts',(-0.195170952608934,0.00270742477528601,
0.00874548965920323));
#45259=CARTESIAN_POINT('Ctrl Pts',(-0.195173638543081,0.00271391111696078,
0.00874039389129896));
#45260=CARTESIAN_POINT('Ctrl Pts',(-0.195177116914226,0.00272511226812696,
0.0087288969971338));
#45261=CARTESIAN_POINT('Ctrl Pts',(-0.195178036555258,0.00272982522991645,
0.00872279506055263));
#45262=CARTESIAN_POINT('Ctrl Pts',(-0.195178162823842,0.00273381293378166,
0.00871612270254606));
#45263=CARTESIAN_POINT('Ctrl Pts',(-0.195102853656511,0.00749647337670453,
0.0100174036489879));
#45264=CARTESIAN_POINT('Ctrl Pts',(-0.195102688430028,0.00749647092519468,
0.0100238445717337));
#45265=CARTESIAN_POINT('Ctrl Pts',(-0.19510189888294,0.0074964684868887,
0.0100302542422684));
#45266=CARTESIAN_POINT('Ctrl Pts',(-0.195098980964152,0.00749646351205413,
0.0100433365704581));
#45267=CARTESIAN_POINT('Ctrl Pts',(-0.195096758536737,0.00749646099736017,
0.0100499522302527));
#45268=CARTESIAN_POINT('Ctrl Pts',(-0.195088512706634,0.00749645413866188,
0.0100679986980086));
#45269=CARTESIAN_POINT('Ctrl Pts',(-0.195080942680449,0.00749645012399971,
0.0100785671796805));
#45270=CARTESIAN_POINT('Ctrl Pts',(-0.195062211056929,0.00749644338711119,
0.0100962620160301));
#45271=CARTESIAN_POINT('Ctrl Pts',(-0.195051223236752,0.00749644073745807,
0.0101032218231675));
#45272=CARTESIAN_POINT('Ctrl Pts',(-0.195019263724858,0.00749643580110644,
0.0101157274017836));
#45273=CARTESIAN_POINT('Ctrl Pts',(-0.195002697944291,0.00749646333374549,
0.0101148515365255));
#45274=CARTESIAN_POINT('Ctrl Pts',(-0.195000719135785,0.00749641518058753,
0.0101148199248467));
#45275=CARTESIAN_POINT('Ctrl Pts',(-0.195000276360688,0.00749643658133645,
0.0101148106853962));
#45276=CARTESIAN_POINT('Ctrl Pts',(-0.195258464889861,0.0127716222143721,
0.00839609631068042));
#45277=CARTESIAN_POINT('Ctrl Pts',(-0.195257661598623,0.0128320002529834,
0.00848495188464948));
#45278=CARTESIAN_POINT('Ctrl Pts',(-0.195151404514474,0.0128381542818839,
0.008470338536568));
#45279=CARTESIAN_POINT('Ctrl Pts',(-0.195119985170156,0.0119260586777307,
0.0089685011811852));
#45280=CARTESIAN_POINT('Ctrl Pts',(-0.195118927457144,0.0119769105830198,
0.00906388973756854));
#45281=CARTESIAN_POINT('Ctrl Pts',(-0.195013028416401,0.0119875277897504,
0.00904845632888441));
#45282=CARTESIAN_POINT('Ctrl Pts',(-0.194853120499905,0.0100615551736861,
0.00982677140189363));
#45283=CARTESIAN_POINT('Ctrl Pts',(-0.194851649079398,0.0100907329171985,
0.00993207689887392));
#45284=CARTESIAN_POINT('Ctrl Pts',(-0.19474373346643,0.0100878065962746,
0.00992624268005921));
#45285=CARTESIAN_POINT('Ctrl Pts',(-0.195062697269868,0.00800323442767928,
0.0100584301848728));
#45286=CARTESIAN_POINT('Ctrl Pts',(-0.195061122180014,0.0080090637473043,
0.0101663618724557));
#45287=CARTESIAN_POINT('Ctrl Pts',(-0.194954647414871,0.00799816636004166,
0.0101575142891252));
#45288=CARTESIAN_POINT('Ctrl Pts',(-0.195146171428379,0.00697914415917188,
0.0100026415787786));
#45289=CARTESIAN_POINT('Ctrl Pts',(-0.195144615154365,0.00697309723419385,
0.0101098951507728));
#45290=CARTESIAN_POINT('Ctrl Pts',(-0.195037915324914,0.00696489230979399,
0.0101001621065224));
#45291=CARTESIAN_POINT('Ctrl Pts',(-0.195178017022907,0.0122621355963516,
0.00871851959969473));
#45292=CARTESIAN_POINT('Ctrl Pts',(-0.195177580509937,0.0122758282388325,
0.00874146027159947));
#45293=CARTESIAN_POINT('Ctrl Pts',(-0.195163460529544,0.012307420071114,
0.00876039280475504));
#45294=CARTESIAN_POINT('Ctrl Pts',(-0.195146437813832,0.0123308055228815,
0.00876514629123138));
#45295=CARTESIAN_POINT('Ctrl Pts',(-0.195131119021796,0.0123518501598455,
0.00876942396772028));
#45296=CARTESIAN_POINT('Ctrl Pts',(-0.195119235232368,0.0123684243934701,
0.00876737961119782));
#45297=CARTESIAN_POINT('Ctrl Pts',(-0.195096603924478,0.0123918748609315,
0.00875552780766066));
#45298=CARTESIAN_POINT('Ctrl Pts',(-0.195094086595983,0.0123944833062879,
0.00875420950635378));
#45299=CARTESIAN_POINT('Ctrl Pts',(-0.19509144745469,0.0123971472448317,
0.00875272329131383));
#45300=CARTESIAN_POINT('Ctrl Pts',(-0.195088692557014,0.012399858493754,
0.00875103165054581));
#45301=CARTESIAN_POINT('Origin',(-0.196341530644781,0.00264910622819491,
0.00868825771150032));
#45302=CARTESIAN_POINT('Ctrl Pts',(-0.196178605749969,0.00273416037407678,
0.00873731991783359));
#45303=CARTESIAN_POINT('Ctrl Pts',(-0.196178579860494,0.00273009299958139,
0.00874394353981102));
#45304=CARTESIAN_POINT('Ctrl Pts',(-0.196179583205907,0.00272533404646618,
0.00874998493616834));
#45305=CARTESIAN_POINT('Ctrl Pts',(-0.196183787973507,0.00271371373445172,
0.00876182314931958));
#45306=CARTESIAN_POINT('Ctrl Pts',(-0.196187307070579,0.00270682499517073,
0.0087671365420531));
#45307=CARTESIAN_POINT('Ctrl Pts',(-0.196198455940222,0.00268861365389419,
0.00877810476957485));
#45308=CARTESIAN_POINT('Ctrl Pts',(-0.196207711713408,0.00267630899606189,
0.00878264090943895));
#45309=CARTESIAN_POINT('Ctrl Pts',(-0.196229260457889,0.0026516694477696,
0.00878669559224456));
#45310=CARTESIAN_POINT('Ctrl Pts',(-0.196240624737327,0.00264014354081433,
0.00878645001839778));
#45311=CARTESIAN_POINT('Ctrl Pts',(-0.1962692611573,0.00261366083176474,
0.00878172908321917));
#45312=CARTESIAN_POINT('Ctrl Pts',(-0.196283191869981,0.00260288006357014,
0.00877586776937855));
#45313=CARTESIAN_POINT('Ctrl Pts',(-0.196287978139581,0.00259953252469863,
0.0087740737788129));
#45314=CARTESIAN_POINT('Ctrl Pts',(-0.196288756787266,0.00259881568571221,
0.0087736695208446));
#45315=CARTESIAN_POINT('Ctrl Pts',(-0.196289802132512,0.00259785720803007,
0.00877312348153903));
#45316=CARTESIAN_POINT('Ctrl Pts',(-0.196290653689677,0.00259721438487426,
0.00877275027888147));
#45317=CARTESIAN_POINT('Origin',(-0.195016314063637,0.0123482798341224,
0.00866394192729312));
#45318=CARTESIAN_POINT('Ctrl Pts',(-0.196177629385444,0.0122611626189316,
0.00874006375723914));
#45319=CARTESIAN_POINT('Ctrl Pts',(-0.196177604684899,0.0122650166111309,
0.00874634656815966));
#45320=CARTESIAN_POINT('Ctrl Pts',(-0.196178505761057,0.0122694952960258,
0.00875211144220574));
#45321=CARTESIAN_POINT('Ctrl Pts',(-0.196182296395684,0.0122803850364228,
0.00876347360160108));
#45322=CARTESIAN_POINT('Ctrl Pts',(-0.196185470343792,0.0122868251469942,
0.0087686457365702));
#45323=CARTESIAN_POINT('Ctrl Pts',(-0.196195776348067,0.0123042086992948,
0.00877970743094284));
#45324=CARTESIAN_POINT('Ctrl Pts',(-0.196204518680032,0.0123161242904747,
0.00878449099801561));
#45325=CARTESIAN_POINT('Ctrl Pts',(-0.196225148046997,0.0123402424928695,
0.00878927088270124));
#45326=CARTESIAN_POINT('Ctrl Pts',(-0.19623615481724,0.0123516331750604,
0.00878941853515255));
#45327=CARTESIAN_POINT('Ctrl Pts',(-0.196261828351012,0.0123758886765458,
0.00878601069113465));
#45328=CARTESIAN_POINT('Ctrl Pts',(-0.196274345460426,0.0123860640870079,
0.00878176003385096));
#45329=CARTESIAN_POINT('Ctrl Pts',(-0.19628311218831,0.0123930638981874,
0.0087782975856912));
#45330=CARTESIAN_POINT('Ctrl Pts',(-0.196285923619682,0.0123952124629935,
0.00877721360122813));
#45331=CARTESIAN_POINT('Ctrl Pts',(-0.196288741215603,0.0123972935671941,
0.00877604129610507));
#45332=CARTESIAN_POINT('Ctrl Pts',(-0.196289697990218,0.0123980152811994,
0.00877562292559277));
#45333=CARTESIAN_POINT('Ctrl Pts',(-0.196261761273723,0.00220825086283849,
0.00840092612408506));
#45334=CARTESIAN_POINT('Ctrl Pts',(-0.196259359103124,0.00215010776402942,
0.00848578996319967));
#45335=CARTESIAN_POINT('Ctrl Pts',(-0.196361456778984,0.0021608707734272,
0.00849264249435443));
#45336=CARTESIAN_POINT('Ctrl Pts',(-0.196124935041166,0.00304408419344697,
0.00897303747973618));
#45337=CARTESIAN_POINT('Ctrl Pts',(-0.196122283249963,0.00299500238841375,
0.00906416088238421));
#45338=CARTESIAN_POINT('Ctrl Pts',(-0.19622404056787,0.00300935915833106,
0.00907131055929637));
#45339=CARTESIAN_POINT('Ctrl Pts',(-0.195850357502235,0.00493054266441542,
0.00985151168271769));
#45340=CARTESIAN_POINT('Ctrl Pts',(-0.195847337738017,0.0049024516121403,
0.00995235738966955));
#45341=CARTESIAN_POINT('Ctrl Pts',(-0.195951044646213,0.0049022109327829,
0.00994954044800188));
#45342=CARTESIAN_POINT('Ctrl Pts',(-0.196063682956604,0.00700246999388266,
0.0100810223901609));
#45343=CARTESIAN_POINT('Ctrl Pts',(-0.196060536777505,0.00699687455558653,
0.0101843537059636));
#45344=CARTESIAN_POINT('Ctrl Pts',(-0.196162895346769,0.00698677679606697,
0.0101840722583427));
#45345=CARTESIAN_POINT('Ctrl Pts',(-0.19614623552346,0.00802067462636459,
0.0100252039093978));
#45346=CARTESIAN_POINT('Ctrl Pts',(-0.196143113583024,0.00802644166365842,
0.0101278989422097));
#45347=CARTESIAN_POINT('Ctrl Pts',(-0.196245695189478,0.00801812145293573,
0.0101285601406757));
#45348=CARTESIAN_POINT('Ctrl Pts',(-0.196102458894692,0.00749683730988234,
0.0100396916414689));
#45349=CARTESIAN_POINT('Ctrl Pts',(-0.196102311008966,0.00749683509874942,
0.0100462351503637));
#45350=CARTESIAN_POINT('Ctrl Pts',(-0.196102808227049,0.00749683305950545,
0.0100527770024187));
#45351=CARTESIAN_POINT('Ctrl Pts',(-0.196105150018785,0.00749682926719129,
0.0100660782667755));
#45352=CARTESIAN_POINT('Ctrl Pts',(-0.196107071555501,0.00749682755110485,
0.010072787915366));
#45353=CARTESIAN_POINT('Ctrl Pts',(-0.196114494416142,0.00749682341853911,
0.0100911887837042));
#45354=CARTESIAN_POINT('Ctrl Pts',(-0.196121579709176,0.00749682168655211,
0.0101020883679008));
#45355=CARTESIAN_POINT('Ctrl Pts',(-0.196139493665661,0.00749682031724726,
0.0101206110477672));
#45356=CARTESIAN_POINT('Ctrl Pts',(-0.196150156255171,0.00749682068764585,
0.0101280599128218));
#45357=CARTESIAN_POINT('Ctrl Pts',(-0.196181811356627,0.0074968245635932,
0.0101421257479467));
#45358=CARTESIAN_POINT('Ctrl Pts',(-0.196198651212673,0.00749682018921974,
0.0101418849547825));
#45359=CARTESIAN_POINT('Ctrl Pts',(-0.196200096295123,0.0074968426416852,
0.0101419270317423));
#45360=CARTESIAN_POINT('Ctrl Pts',(-0.196200203314133,0.00749682939312149,
0.0101419301637073));
#45361=CARTESIAN_POINT('Ctrl Pts',(-0.196200533508802,0.00749682933724156,
0.0101419376171861));
#45362=CARTESIAN_POINT('Ctrl Pts',(-0.19636080552077,0.0128345631145169,
0.00849574728918621));
#45363=CARTESIAN_POINT('Ctrl Pts',(-0.196258557059731,0.0128454370666705,
0.0084889752095364));
#45364=CARTESIAN_POINT('Ctrl Pts',(-0.19626099705554,0.0127872520572483,
0.00840395151994793));
#45365=CARTESIAN_POINT('Ctrl Pts',(-0.196223005201044,0.0119856357125536,
0.00907398755842464));
#45366=CARTESIAN_POINT('Ctrl Pts',(-0.196121099622317,0.0120001214234957,
0.00906692248765129));
#45367=CARTESIAN_POINT('Ctrl Pts',(-0.196123789273586,0.0119510144111196,
0.00897563473339434));
#45368=CARTESIAN_POINT('Ctrl Pts',(-0.195949420026854,0.0100919430838383,
0.0099511818246222));
#45369=CARTESIAN_POINT('Ctrl Pts',(-0.195845548801905,0.0100916748893939,
0.00995415151336621));
#45370=CARTESIAN_POINT('Ctrl Pts',(-0.195848607042909,0.0100636041876074,
0.0098531341357168));
#45371=CARTESIAN_POINT('Ctrl Pts',(-0.196162792162144,0.00800692503941795,
0.0101844280639557));
#45372=CARTESIAN_POINT('Ctrl Pts',(-0.196060284308471,0.00799676411255229,
0.0101848280330257));
#45373=CARTESIAN_POINT('Ctrl Pts',(-0.196063468158884,0.00799123551783281,
0.010081336579869));
#45374=CARTESIAN_POINT('Ctrl Pts',(-0.196246080332815,0.00697549324604494,
0.0101282087141702));
#45375=CARTESIAN_POINT('Ctrl Pts',(-0.196143346637859,0.00696709994606931,
0.0101276618554586));
#45376=CARTESIAN_POINT('Ctrl Pts',(-0.196146506172932,0.00697294832614626,
0.0100248157795735));
#45377=CARTESIAN_POINT('Ctrl Pts',(-0.221150461937767,0.00811962085575298,
0.0105825552134681));
#45378=CARTESIAN_POINT('Ctrl Pts',(-0.2211495396963,0.00812732088454214,
0.0106927229483897));
#45379=CARTESIAN_POINT('Ctrl Pts',(-0.221040101821991,0.00813555022692369,
0.0106801850925946));
#45380=CARTESIAN_POINT('Ctrl Pts',(-0.221032677065535,0.00689153715468521,
0.0106668145952798));
#45381=CARTESIAN_POINT('Ctrl Pts',(-0.22103172824819,0.00688383601422594,
0.0107780583691776));
#45382=CARTESIAN_POINT('Ctrl Pts',(-0.220922567010128,0.00689630991786673,
0.0107669036634824));
#45383=CARTESIAN_POINT('Ctrl Pts',(-0.220896608196396,0.0050972250828522,
0.0104177246389459));
#45384=CARTESIAN_POINT('Ctrl Pts',(-0.220895752802238,0.00506778132256289,
0.0105259415777043));
#45385=CARTESIAN_POINT('Ctrl Pts',(-0.220785305656289,0.00507181257794575,
0.0105169696830634));
#45386=CARTESIAN_POINT('Ctrl Pts',(-0.221099672568277,0.00282025323552542,
0.00935943618997168));
#45387=CARTESIAN_POINT('Ctrl Pts',(-0.221099319942786,0.00276243769422579,
0.00945448593572196));
#45388=CARTESIAN_POINT('Ctrl Pts',(-0.220990565430845,0.00275247842578777,
0.00943635408645135));
#45389=CARTESIAN_POINT('Ctrl Pts',(-0.22139514771026,0.00185666417523725,
0.00864445166450529));
#45390=CARTESIAN_POINT('Ctrl Pts',(-0.22139511152028,0.00178727927747294,
0.00873084239674152));
#45391=CARTESIAN_POINT('Ctrl Pts',(-0.221288280479528,0.00177389461696801,
0.00870594947214869));
#45392=CARTESIAN_POINT('Ctrl Pts',(-0.221544108200661,0.00133248767187958,
0.00815434837593592));
#45393=CARTESIAN_POINT('Ctrl Pts',(-0.221544269965813,0.00125651031431327,
0.00823458355479384));
#45394=CARTESIAN_POINT('Ctrl Pts',(-0.221436545998082,0.00124802503912297,
0.00821143217143996));
#45395=CARTESIAN_POINT('Ctrl Pts',(-0.221311628769438,0.00171848642413581,
0.00862619824224493));
#45396=CARTESIAN_POINT('Ctrl Pts',(-0.221335049690428,0.00174110173044518,
0.00864534820546848));
#45397=CARTESIAN_POINT('Ctrl Pts',(-0.221348766211921,0.00175797442052312,
0.00864927269533899));
#45398=CARTESIAN_POINT('Ctrl Pts',(-0.221361583393583,0.0017796554992303,
0.00865009179604268));
#45399=CARTESIAN_POINT('Ctrl Pts',(-0.221362743032725,0.00178161710266088,
0.00865016590447483));
#45400=CARTESIAN_POINT('Ctrl Pts',(-0.221363895896245,0.00178363088934365,
0.00865018385643546));
#45401=CARTESIAN_POINT('Ctrl Pts',(-0.221365048880398,0.00178570794336532,
0.00865013521475478));
#45402=CARTESIAN_POINT('Ctrl Pts',(-0.221378945476116,0.00181074209492944,
0.0086495489501735));
#45403=CARTESIAN_POINT('Ctrl Pts',(-0.221392953879523,0.00184293580361415,
0.00863455712906129));
#45404=CARTESIAN_POINT('Ctrl Pts',(-0.22139331361059,0.0018597065642107,
0.00861406379669157));
#45405=CARTESIAN_POINT('Ctrl Pts',(-0.221093378117463,0.00749708146235502,
0.0106049495976336));
#45406=CARTESIAN_POINT('Ctrl Pts',(-0.221093205142074,0.00749707938042166,
0.0106113459163336));
#45407=CARTESIAN_POINT('Ctrl Pts',(-0.221092416367657,0.00749707747540696,
0.010617710754281));
#45408=CARTESIAN_POINT('Ctrl Pts',(-0.221089506457863,0.00749707392137382,
0.0106307519256261));
#45409=CARTESIAN_POINT('Ctrl Pts',(-0.221087282431476,0.00749707231971561,
0.0106373694403386));
#45410=CARTESIAN_POINT('Ctrl Pts',(-0.221079032172649,0.00749706854074414,
0.0106554173015107));
#45411=CARTESIAN_POINT('Ctrl Pts',(-0.221071459539386,0.00749706706830675,
0.0106659849606413));
#45412=CARTESIAN_POINT('Ctrl Pts',(-0.221052722966754,0.00749706622792382,
0.0106836774393237));
#45413=CARTESIAN_POINT('Ctrl Pts',(-0.221041732788639,0.00749706687881053,
0.0106906356764216));
#45414=CARTESIAN_POINT('Ctrl Pts',(-0.221016370204857,0.00749707029332032,
0.010700554781231));
#45415=CARTESIAN_POINT('Ctrl Pts',(-0.221003692357774,0.00749708761297438,
0.0107022186490283));
#45416=CARTESIAN_POINT('Ctrl Pts',(-0.220992859660385,0.00749707123864509,
0.0107022443220174));
#45417=CARTESIAN_POINT('Ctrl Pts',(-0.220992434802756,0.00749707047723624,
0.0107022424122139));
#45418=CARTESIAN_POINT('Ctrl Pts',(-0.220991842577576,0.00749706643585074,
0.0107022363855843));
#45419=CARTESIAN_POINT('Ctrl Pts',(-0.2209915935623,0.00749706431881418,
0.0107022330643159));
#45420=CARTESIAN_POINT('Ctrl Pts',(-0.220991241417974,0.00749705445135643,
0.010702227262308));
#45421=CARTESIAN_POINT('Ctrl Pts',(-0.220990864889388,0.00749696165836036,
0.0107022195991458));
#45422=CARTESIAN_POINT('Ctrl Pts',(-0.221039491002263,0.00685968436868825,
0.0106798040221069));
#45423=CARTESIAN_POINT('Ctrl Pts',(-0.2211492365355,0.00686784362818015,
0.0106927234678917));
#45424=CARTESIAN_POINT('Ctrl Pts',(-0.221150162182504,0.00687562622327931,
0.0105822167718128));
#45425=CARTESIAN_POINT('Ctrl Pts',(-0.220922250319514,0.0080967120552641,
0.0107670355630445));
#45426=CARTESIAN_POINT('Ctrl Pts',(-0.221031721906841,0.00810919801080945,
0.0107785744055876));
#45427=CARTESIAN_POINT('Ctrl Pts',(-0.221032674276105,0.00810155969385244,
0.0106669825539216));
#45428=CARTESIAN_POINT('Ctrl Pts',(-0.220788218290202,0.00991813533979832,
0.0105192170441643));
#45429=CARTESIAN_POINT('Ctrl Pts',(-0.220898965091819,0.00992213316049332,
0.0105286086746672));
#45430=CARTESIAN_POINT('Ctrl Pts',(-0.220899825135949,0.00989272597187494,
0.0104200247978636));
#45431=CARTESIAN_POINT('Ctrl Pts',(-0.220993366234941,0.0122349103118159,
0.00944376699900189));
#45432=CARTESIAN_POINT('Ctrl Pts',(-0.221102422349815,0.0122250398274275,
0.00946224918086765));
#45433=CARTESIAN_POINT('Ctrl Pts',(-0.221102779185047,0.0121671951175703,
0.00936681518662684));
#45434=CARTESIAN_POINT('Ctrl Pts',(-0.221293686408273,0.0132125520200273,
0.00871678626296279));
#45435=CARTESIAN_POINT('Ctrl Pts',(-0.221400740809213,0.0131990319642865,
0.00874220143421774));
#45436=CARTESIAN_POINT('Ctrl Pts',(-0.221400781399722,0.0131295984931284,
0.00865540763741799));
#45437=CARTESIAN_POINT('Ctrl Pts',(-0.221443349927793,0.0137382361695334,
0.00822458347293278));
#45438=CARTESIAN_POINT('Ctrl Pts',(-0.221551332642022,0.0137297760742548,
0.0082481846551935));
#45439=CARTESIAN_POINT('Ctrl Pts',(-0.221551177097651,0.013653735905962,
0.00816753405499274));
#45440=CARTESIAN_POINT('Ctrl Pts',(-0.221398994600239,0.0131267929917585,
0.00862507463528867));
#45441=CARTESIAN_POINT('Ctrl Pts',(-0.221398891939579,0.0131316229516505,
0.00863100166036205));
#45442=CARTESIAN_POINT('Ctrl Pts',(-0.221398088470179,0.0131370777877344,
0.00863629298538617));
#45443=CARTESIAN_POINT('Ctrl Pts',(-0.22139502985258,0.0131495873621591,
0.00864593890691218));
#45444=CARTESIAN_POINT('Ctrl Pts',(-0.221392666461445,0.0131566114257431,
0.00865003283544232));
#45445=CARTESIAN_POINT('Ctrl Pts',(-0.221384721392673,0.0131760488259407,
0.00865847676490165));
#45446=CARTESIAN_POINT('Ctrl Pts',(-0.221378157530941,0.0131886255371438,
0.00866101697794908));
#45447=CARTESIAN_POINT('Ctrl Pts',(-0.221363533028657,0.0132126585780711,
0.00866158988192774));
#45448=CARTESIAN_POINT('Ctrl Pts',(-0.221355517305592,0.0132241274980054,
0.00865973056392319));
#45449=CARTESIAN_POINT('Ctrl Pts',(-0.221335852230188,0.0132492406714318,
0.00865134678022098));
#45450=CARTESIAN_POINT('Ctrl Pts',(-0.221326472378544,0.0132589786142125,
0.0086444552679184));
#45451=CARTESIAN_POINT('Ctrl Pts',(-0.221321893750534,0.0132634897311423,
0.0086410835650841));
#45452=CARTESIAN_POINT('Ctrl Pts',(-0.221319816394641,0.0132656643245537,
0.00863943976353927));
#45453=CARTESIAN_POINT('Ctrl Pts',(-0.221317746469157,0.0132677508018423,
0.00863769213611541));
#45454=CARTESIAN_POINT('Ctrl Pts',(-0.221317509604566,0.0132679808638495,
0.0086374981209002));
#45455=CARTESIAN_POINT('Origin',(-0.222557040593836,0.00178348666403939,
0.0085734100013149));
#45456=CARTESIAN_POINT('Ctrl Pts',(-0.222392821469384,0.00185976161919177,
0.00863469597942385));
#45457=CARTESIAN_POINT('Ctrl Pts',(-0.222392851665228,0.00185471841683084,
0.00864067695413965));
#45458=CARTESIAN_POINT('Ctrl Pts',(-0.2223940171567,0.00184908923740676,
0.00864595328592874));
#45459=CARTESIAN_POINT('Ctrl Pts',(-0.222398791623032,0.00183568068451202,
0.00865603804918068));
#45460=CARTESIAN_POINT('Ctrl Pts',(-0.222402792716745,0.001827955969436,
0.00866029353481253));
#45461=CARTESIAN_POINT('Ctrl Pts',(-0.222415271837931,0.00180816896025231,
0.00866840805978246));
#45462=CARTESIAN_POINT('Ctrl Pts',(-0.22242559622064,0.00179522568857694,
0.00867101548583902));
#45463=CARTESIAN_POINT('Ctrl Pts',(-0.222448811324784,0.00177087556880312,
0.00867117726491881));
#45464=CARTESIAN_POINT('Ctrl Pts',(-0.222460500420385,0.0017601953052336,
0.00866936374343137));
#45465=CARTESIAN_POINT('Ctrl Pts',(-0.222488934943182,0.0017368874233403,
0.00866177871632728));
#45466=CARTESIAN_POINT('Ctrl Pts',(-0.222502563560879,0.00172781843157747,
0.00865561058774906));
#45467=CARTESIAN_POINT('Ctrl Pts',(-0.222508821481566,0.00172382527717114,
0.00865277338878037));
#45468=CARTESIAN_POINT('Ctrl Pts',(-0.222511943488237,0.00172173990045585,
0.00865127231333268));
#45469=CARTESIAN_POINT('Ctrl Pts',(-0.222515286760213,0.00171959773431523,
0.00864956320157879));
#45470=CARTESIAN_POINT('Origin',(-0.221237455096366,0.0132044515326223,
0.00855877605601754));
#45471=CARTESIAN_POINT('Ctrl Pts',(-0.22239855467333,0.013126959871322,
0.00864556967094923));
#45472=CARTESIAN_POINT('Ctrl Pts',(-0.222398693734901,0.0131508497456262,
0.00867409420882899));
#45473=CARTESIAN_POINT('Ctrl Pts',(-0.222421879764434,0.0131819804421261,
0.00868215664988287));
#45474=CARTESIAN_POINT('Ctrl Pts',(-0.22244667526595,0.0132098804246437,
0.00867921869573823));
#45475=CARTESIAN_POINT('Ctrl Pts',(-0.222467868815537,0.0132337274786178,
0.00867670752746002));
#45476=CARTESIAN_POINT('Ctrl Pts',(-0.222493016945457,0.0132565629439438,
0.00866887354856461));
#45477=CARTESIAN_POINT('Ctrl Pts',(-0.222521349609231,0.0132671009264466,
0.00866069085884597));
#45478=CARTESIAN_POINT('Ctrl Pts',(-0.222249879452339,0.00812452848998182,
0.010708612169071));
#45479=CARTESIAN_POINT('Ctrl Pts',(-0.222147518448448,0.00813291623381584,
0.0107075640119653));
#45480=CARTESIAN_POINT('Ctrl Pts',(-0.222150626988561,0.00812566746543201,
0.0106051733469215));
#45481=CARTESIAN_POINT('Ctrl Pts',(-0.222133026314569,0.00688653200057354,
0.0107938566452843));
#45482=CARTESIAN_POINT('Ctrl Pts',(-0.222030952328141,0.00689749083265872,
0.0107941909562852));
#45483=CARTESIAN_POINT('Ctrl Pts',(-0.222034092623134,0.0069045120619468,
0.0106907926699249));
#45484=CARTESIAN_POINT('Ctrl Pts',(-0.22199453534553,0.00506519692361534,
0.0105419098967548));
#45485=CARTESIAN_POINT('Ctrl Pts',(-0.221891198357135,0.00506624553307757,
0.0105441068399897));
#45486=CARTESIAN_POINT('Ctrl Pts',(-0.221894228499143,0.00509371640154661,
0.0104434958915309));
#45487=CARTESIAN_POINT('Ctrl Pts',(-0.222202898757155,0.00275215309907751,
0.00946096055553374));
#45488=CARTESIAN_POINT('Ctrl Pts',(-0.222101363550626,0.00273655987836659,
0.00945278298769915));
#45489=CARTESIAN_POINT('Ctrl Pts',(-0.222103946704122,0.0027907538603155,
0.00936468088853639));
#45490=CARTESIAN_POINT('Ctrl Pts',(-0.222502984837095,0.0017766303999828,
0.00873137796397993));
#45491=CARTESIAN_POINT('Ctrl Pts',(-0.222403127086071,0.00175761006895396,
0.00871654143776575));
#45492=CARTESIAN_POINT('Ctrl Pts',(-0.222405448098085,0.00182264005112638,
0.00863665510434452));
#45493=CARTESIAN_POINT('Ctrl Pts',(-0.222649516124785,0.00125128420842517,
0.00823635580503606));
#45494=CARTESIAN_POINT('Ctrl Pts',(-0.222548875458837,0.00123596872506605,
0.00822244965460723));
#45495=CARTESIAN_POINT('Ctrl Pts',(-0.222550999194757,0.00130702015936901,
0.00814827332314741));
#45496=CARTESIAN_POINT('Ctrl Pts',(-0.222093144978732,0.00749648852186606,
0.0106271018238363));
#45497=CARTESIAN_POINT('Ctrl Pts',(-0.222092997107659,0.00749648591386968,
0.0106336443875128));
#45498=CARTESIAN_POINT('Ctrl Pts',(-0.222093494220433,0.00749648312939007,
0.0106401852870836));
#45499=CARTESIAN_POINT('Ctrl Pts',(-0.222095835536279,0.00749647710304743,
0.010653484677253));
#45500=CARTESIAN_POINT('Ctrl Pts',(-0.222097756689006,0.00749647386023141,
0.0106601933989456));
#45501=CARTESIAN_POINT('Ctrl Pts',(-0.222105178870428,0.00749646437817162,
0.0106785939630422));
#45502=CARTESIAN_POINT('Ctrl Pts',(-0.222112264289149,0.00749645802673394,
0.0106894939842665));
#45503=CARTESIAN_POINT('Ctrl Pts',(-0.222130179059406,0.00749644565024443,
0.0107080180341044));
#45504=CARTESIAN_POINT('Ctrl Pts',(-0.222140842483058,0.00749643973517114,
0.0107154676427388));
#45505=CARTESIAN_POINT('Ctrl Pts',(-0.222172400273181,0.00749642562068748,
0.0107294912223153));
#45506=CARTESIAN_POINT('Ctrl Pts',(-0.222189155075009,0.00749640861672746,
0.0107292902671688));
#45507=CARTESIAN_POINT('Ctrl Pts',(-0.222190773040506,0.00749643501029294,
0.0107293377107985));
#45508=CARTESIAN_POINT('Ctrl Pts',(-0.222190885265316,0.00749642040198078,
0.0107293409891968));
#45509=CARTESIAN_POINT('Ctrl Pts',(-0.222191215574431,0.00749642030964181,
0.0107293485047956));
#45510=CARTESIAN_POINT('Ctrl Pts',(-0.22215039542817,0.00686823386554683,
0.0106047411261954));
#45511=CARTESIAN_POINT('Ctrl Pts',(-0.222147291245924,0.00686090299773189,
0.0107073006204878));
#45512=CARTESIAN_POINT('Ctrl Pts',(-0.222249829666163,0.00686926077332403,
0.0107081718176659));
#45513=CARTESIAN_POINT('Ctrl Pts',(-0.222033882153739,0.00808751688966911,
0.0106910818583913));
#45514=CARTESIAN_POINT('Ctrl Pts',(-0.222030746230797,0.00809445663738906,
0.0107946576004359));
#45515=CARTESIAN_POINT('Ctrl Pts',(-0.222133001056444,0.00810538495115661,
0.0107941436327104));
#45516=CARTESIAN_POINT('Ctrl Pts',(-0.22189809572205,0.00989579664481618,
0.0104460000225152));
#45517=CARTESIAN_POINT('Ctrl Pts',(-0.221895068156802,0.00992318971953597,
0.0105468118004952));
#45518=CARTESIAN_POINT('Ctrl Pts',(-0.221998571699939,0.00992407913617585,
0.0105444854422989));
#45519=CARTESIAN_POINT('Ctrl Pts',(-0.222106552859369,0.0121968557973979,
0.00937209506599623));
#45520=CARTESIAN_POINT('Ctrl Pts',(-0.222103972397347,0.0122510011058486,
0.0094604296734285));
#45521=CARTESIAN_POINT('Ctrl Pts',(-0.222205682870112,0.012235266783474,
0.00946843760091433));
#45522=CARTESIAN_POINT('Ctrl Pts',(-0.222411459865652,0.0131644409687035,
0.00864713334535926));
#45523=CARTESIAN_POINT('Ctrl Pts',(-0.222409139563845,0.0132294340807041,
0.0087272747710823));
#45524=CARTESIAN_POINT('Ctrl Pts',(-0.222509083672908,0.0132099447880335,
0.00874218337616711));
#45525=CARTESIAN_POINT('Ctrl Pts',(-0.222558486991795,0.0136798443822662,
0.00816098211452363));
#45526=CARTESIAN_POINT('Ctrl Pts',(-0.222556362475417,0.0137508603207363,
0.00823543380177068));
#45527=CARTESIAN_POINT('Ctrl Pts',(-0.222657130762485,0.013735231609234,
0.00824934739737568));
#45528=CARTESIAN_POINT('Ctrl Pts',(-0.219148404100077,0.00808836362885957,
0.0105397408946697));
#45529=CARTESIAN_POINT('Ctrl Pts',(-0.219147286260384,0.00809560494432423,
0.0106488954886024));
#45530=CARTESIAN_POINT('Ctrl Pts',(-0.219038810118551,0.00810395989687771,
0.0106373208135017));
#45531=CARTESIAN_POINT('Ctrl Pts',(-0.219036260639061,0.00692355290527283,
0.0106150424470077));
#45532=CARTESIAN_POINT('Ctrl Pts',(-0.219035119802892,0.00691634871689329,
0.0107251414266647));
#45533=CARTESIAN_POINT('Ctrl Pts',(-0.218926885305538,0.00692862928927927,
0.0107149222445564));
#45534=CARTESIAN_POINT('Ctrl Pts',(-0.218905493367159,0.00522543643497804,
0.0103925587148312));
#45535=CARTESIAN_POINT('Ctrl Pts',(-0.218904431859709,0.00519797604222467,
0.010500029300181));
#45536=CARTESIAN_POINT('Ctrl Pts',(-0.218795072781458,0.00520197616056926,
0.0104916549790139));
#45537=CARTESIAN_POINT('Ctrl Pts',(-0.219069945774343,0.00304060262385979,
0.00944022647325578));
#45538=CARTESIAN_POINT('Ctrl Pts',(-0.219069332996938,0.00298616501663537,
0.00953594714440858));
#45539=CARTESIAN_POINT('Ctrl Pts',(-0.218961240632144,0.00297739205618275,
0.00951996720256591));
#45540=CARTESIAN_POINT('Ctrl Pts',(-0.219322800899811,0.00209990025679052,
0.00879058344321244));
#45541=CARTESIAN_POINT('Ctrl Pts',(-0.219322481672864,0.00203429555214399,
0.00887852267246854));
#45542=CARTESIAN_POINT('Ctrl Pts',(-0.219216100504328,0.00202134997278713,
0.00885622517805967));
#45543=CARTESIAN_POINT('Ctrl Pts',(-0.219451770062291,0.00158485407297901,
0.00834673001569572));
#45544=CARTESIAN_POINT('Ctrl Pts',(-0.219451626127622,0.00151291782239926,
0.00842920614775955));
#45545=CARTESIAN_POINT('Ctrl Pts',(-0.219344450923872,0.00150470339121809,
0.0084085948337711));
#45546=CARTESIAN_POINT('Ctrl Pts',(-0.219329643945211,0.00206973899609492,
0.00873934399098496));
#45547=CARTESIAN_POINT('Ctrl Pts',(-0.21932954767613,0.00206564252185154,
0.00874469986786621));
#45548=CARTESIAN_POINT('Ctrl Pts',(-0.219328831198008,0.00206126786037065,
0.00874979857642302));
#45549=CARTESIAN_POINT('Ctrl Pts',(-0.219326098049909,0.00205177977988729,
0.00875966351192551));
#45550=CARTESIAN_POINT('Ctrl Pts',(-0.219324006068103,0.00204667681545294,
0.00876433959539986));
#45551=CARTESIAN_POINT('Ctrl Pts',(-0.219316297145377,0.00203190722576044,
0.00877620076329959));
#45552=CARTESIAN_POINT('Ctrl Pts',(-0.219309292282347,0.00202216812127946,
0.00878207855087985));
#45553=CARTESIAN_POINT('Ctrl Pts',(-0.2192921175356,0.00200325932998677,
0.00878988793020369));
#45554=CARTESIAN_POINT('Ctrl Pts',(-0.219282057436856,0.00199427474463678,
0.00879168528662207));
#45555=CARTESIAN_POINT('Ctrl Pts',(-0.219259249035481,0.00197748116797533,
0.00879101814240679));
#45556=CARTESIAN_POINT('Ctrl Pts',(-0.219249069113353,0.00197189892749821,
0.00878821256821367));
#45557=CARTESIAN_POINT('Ctrl Pts',(-0.219242270579201,0.00196834740913877,
0.00878599194012615));
#45558=CARTESIAN_POINT('Ctrl Pts',(-0.219240172952592,0.00196731085858162,
0.00878530517930024));
#45559=CARTESIAN_POINT('Ctrl Pts',(-0.219238073822237,0.00196633000923113,
0.00878455699842097));
#45560=CARTESIAN_POINT('Ctrl Pts',(-0.219237124510089,0.00196588311043685,
0.0087841963906634));
#45561=CARTESIAN_POINT('Ctrl Pts',(-0.219093939821662,0.00749806050132961,
0.010559781147994));
#45562=CARTESIAN_POINT('Ctrl Pts',(-0.219093765728207,0.00749805919151256,
0.0105661708589535));
#45563=CARTESIAN_POINT('Ctrl Pts',(-0.21909297706098,0.00749805803365454,
0.0105725290512502));
#45564=CARTESIAN_POINT('Ctrl Pts',(-0.219090068280447,0.00749805597621986,
0.0105855639856694));
#45565=CARTESIAN_POINT('Ctrl Pts',(-0.219087843995007,0.00749805511454117,
0.0105921816327154));
#45566=CARTESIAN_POINT('Ctrl Pts',(-0.21907959284429,0.00749805332442967,
0.0106102297141528));
#45567=CARTESIAN_POINT('Ctrl Pts',(-0.219072019489481,0.00749805296861923,
0.0106207972909321));
#45568=CARTESIAN_POINT('Ctrl Pts',(-0.2190532813129,0.00749805415624955,
0.0106384896244247));
#45569=CARTESIAN_POINT('Ctrl Pts',(-0.219042290189228,0.00749805556350332,
0.0106454477078487));
#45570=CARTESIAN_POINT('Ctrl Pts',(-0.219019950092807,0.00749806122118377,
0.0106541837873464));
#45571=CARTESIAN_POINT('Ctrl Pts',(-0.219009039840112,0.00749804440964752,
0.0106564778252645));
#45572=CARTESIAN_POINT('Ctrl Pts',(-0.218995817113753,0.00749809073883346,
0.0106570547372539));
#45573=CARTESIAN_POINT('Ctrl Pts',(-0.218993530063054,0.00749806237148593,
0.0106570788650823));
#45574=CARTESIAN_POINT('Ctrl Pts',(-0.218991338855106,0.00749806287369093,
0.0106570293466482));
#45575=CARTESIAN_POINT('Ctrl Pts',(-0.219458972439161,0.0134081066407698,
0.00835293645932442));
#45576=CARTESIAN_POINT('Ctrl Pts',(-0.219458332634967,0.0134799305966825,
0.00843531702472389));
#45577=CARTESIAN_POINT('Ctrl Pts',(-0.219351364553155,0.0134880627422249,
0.00841432815581591));
#45578=CARTESIAN_POINT('Ctrl Pts',(-0.219330919335611,0.0129021834400454,
0.00878997306616953));
#45579=CARTESIAN_POINT('Ctrl Pts',(-0.219330111991264,0.0129678170383922,
0.00887771930160673));
#45580=CARTESIAN_POINT('Ctrl Pts',(-0.219223960476356,0.0129807630116758,
0.00885498650689457));
#45581=CARTESIAN_POINT('Ctrl Pts',(-0.21907217366948,0.0119507491293741,
0.00944613164313236));
#45582=CARTESIAN_POINT('Ctrl Pts',(-0.219071061787161,0.0120050759109758,
0.00954176136696198));
#45583=CARTESIAN_POINT('Ctrl Pts',(-0.218963148115845,0.0120137476734168,
0.00952545967271347));
#45584=CARTESIAN_POINT('Ctrl Pts',(-0.218908878443448,0.00977018641413983,
0.0103930111689677));
#45585=CARTESIAN_POINT('Ctrl Pts',(-0.218907313830057,0.00979754952644692,
0.010500350610888));
#45586=CARTESIAN_POINT('Ctrl Pts',(-0.218798131116708,0.00979356929641045,
0.0104915911911937));
#45587=CARTESIAN_POINT('Ctrl Pts',(-0.21903560702607,0.0080761058161286,
0.0106160018814049));
#45588=CARTESIAN_POINT('Ctrl Pts',(-0.219033968343184,0.00808324228078203,
0.0107259654053647));
#45589=CARTESIAN_POINT('Ctrl Pts',(-0.218925901646514,0.00807099086232866,
0.0107153948463322));
#45590=CARTESIAN_POINT('Ctrl Pts',(-0.219148501134292,0.00690552738431865,
0.0105398630894422));
#45591=CARTESIAN_POINT('Ctrl Pts',(-0.219146884619599,0.00689818019381566,
0.0106488663910279));
#45592=CARTESIAN_POINT('Ctrl Pts',(-0.219038578450512,0.00688992144780411,
0.0106369402406613));
#45593=CARTESIAN_POINT('Ctrl Pts',(-0.219334447815789,0.0129187822150905,
0.00874810840271639));
#45594=CARTESIAN_POINT('Ctrl Pts',(-0.219334349313406,0.0129229875332314,
0.00875361950638557));
#45595=CARTESIAN_POINT('Ctrl Pts',(-0.219333611885487,0.0129275458909777,
0.00875880523042341));
#45596=CARTESIAN_POINT('Ctrl Pts',(-0.219330800131034,0.0129375763567918,
0.00876872890637208));
#45597=CARTESIAN_POINT('Ctrl Pts',(-0.219328645180264,0.0129430363384887,
0.00877334976205868));
#45598=CARTESIAN_POINT('Ctrl Pts',(-0.219320864830539,0.0129587194547766,
0.00878463247984444));
#45599=CARTESIAN_POINT('Ctrl Pts',(-0.219313950560981,0.0129690726824846,
0.00878985601767334));
#45600=CARTESIAN_POINT('Ctrl Pts',(-0.219297070769606,0.012989588910634,
0.00879623291603491));
#45601=CARTESIAN_POINT('Ctrl Pts',(-0.219287139859611,0.0129995534686749,
0.0087971642880923));
#45602=CARTESIAN_POINT('Ctrl Pts',(-0.219268011982728,0.0130157461221668,
0.00879493805234113));
#45603=CARTESIAN_POINT('Ctrl Pts',(-0.219259084995648,0.0130222780130516,
0.00879255390199529));
#45604=CARTESIAN_POINT('Ctrl Pts',(-0.219248202110861,0.0130291638450967,
0.00878810745217938));
#45605=CARTESIAN_POINT('Ctrl Pts',(-0.219246191884804,0.013030361992373,
0.00878724563927881));
#45606=CARTESIAN_POINT('Ctrl Pts',(-0.219244237320854,0.0130315050188546,
0.00878633307433836));
#45607=CARTESIAN_POINT('Ctrl Pts',(-0.220652621774988,0.00171860875021885,
0.00861403983191908));
#45608=CARTESIAN_POINT('Ctrl Pts',(-0.22065070898904,0.00179715124586783,
0.00868074893703625));
#45609=CARTESIAN_POINT('Ctrl Pts',(-0.220652186979373,0.00186150990883231,
0.00860050117613837));
#45610=CARTESIAN_POINT('Ctrl Pts',(-0.22038156151548,0.00172153788266806,
0.00861139809863215));
#45611=CARTESIAN_POINT('Ctrl Pts',(-0.220379331631024,0.0017994467145094,
0.0086774643645163));
#45612=CARTESIAN_POINT('Ctrl Pts',(-0.220380902934705,0.00186376460487148,
0.00859721360678668));
#45613=CARTESIAN_POINT('Ctrl Pts',(-0.219997085557986,0.00169755239672656,
0.00858453373495456));
#45614=CARTESIAN_POINT('Ctrl Pts',(-0.219993559109339,0.00177816495585469,
0.00865325916554496));
#45615=CARTESIAN_POINT('Ctrl Pts',(-0.219994933861779,0.00184264803256065,
0.00857302038288794));
#45616=CARTESIAN_POINT('Ctrl Pts',(-0.219457398216233,0.0018050393200918,
0.00866289593480801));
#45617=CARTESIAN_POINT('Ctrl Pts',(-0.21950512140762,0.00187792237709183,
0.00872395721311587));
#45618=CARTESIAN_POINT('Ctrl Pts',(-0.219505746247963,0.00194139912405486,
0.00864325897028411));
#45619=CARTESIAN_POINT('Ctrl Pts',(-0.219252194129174,0.00195596694160954,
0.00877794624534211));
#45620=CARTESIAN_POINT('Ctrl Pts',(-0.219324471820114,0.00201229795546534,
0.00882429986098872));
#45621=CARTESIAN_POINT('Ctrl Pts',(-0.219325359194532,0.00207418376706999,
0.00874287956348477));
#45622=CARTESIAN_POINT('Ctrl Pts',(-0.219129805649029,0.00203517720513716,
0.0088345274762402));
#45623=CARTESIAN_POINT('Ctrl Pts',(-0.219189125076113,0.00210065585944006,
0.00888677249466793));
#45624=CARTESIAN_POINT('Ctrl Pts',(-0.219190162076039,0.00216143160586825,
0.00880428766836637));
#45625=CARTESIAN_POINT('Ctrl Pts',(-0.220393521722421,0.00185901092063506,
0.00859658671256956));
#45626=CARTESIAN_POINT('Ctrl Pts',(-0.220393545683691,0.00185536086192936,
0.00860093418665886));
#45627=CARTESIAN_POINT('Ctrl Pts',(-0.220394166592933,0.00185139129769321,
0.00860493128106815));
#45628=CARTESIAN_POINT('Ctrl Pts',(-0.220397494433511,0.00183939323794458,
0.00861522365214686));
#45629=CARTESIAN_POINT('Ctrl Pts',(-0.22040142365534,0.00183106621657628,
0.00862036967205643));
#45630=CARTESIAN_POINT('Ctrl Pts',(-0.220413421988607,0.00181115837561913,
0.00862944761777806));
#45631=CARTESIAN_POINT('Ctrl Pts',(-0.220422944779313,0.00179879060235556,
0.00863252660109762));
#45632=CARTESIAN_POINT('Ctrl Pts',(-0.220446693838697,0.00177307264120848,
0.00863403325035388));
#45633=CARTESIAN_POINT('Ctrl Pts',(-0.220460216415066,0.00176067973120046,
0.00863218189800322));
#45634=CARTESIAN_POINT('Ctrl Pts',(-0.220480884415075,0.00174394626121798,
0.00862668378645218));
#45635=CARTESIAN_POINT('Ctrl Pts',(-0.220487970824601,0.00173858167731576,
0.00862434869605683));
#45636=CARTESIAN_POINT('Ctrl Pts',(-0.220498562066858,0.0017310627344125,
0.00862024819021514));
#45637=CARTESIAN_POINT('Ctrl Pts',(-0.220502054976112,0.00172866352663628,
0.00861879861371333));
#45638=CARTESIAN_POINT('Ctrl Pts',(-0.220507287796832,0.00172517941353552,
0.00861647938973381));
#45639=CARTESIAN_POINT('Ctrl Pts',(-0.220509010984543,0.00172405157047886,
0.00861569195890217));
#45640=CARTESIAN_POINT('Ctrl Pts',(-0.220511587454697,0.00172237856914534,
0.00861447017639169));
#45641=CARTESIAN_POINT('Ctrl Pts',(-0.220512494461661,0.00172179370048413,
0.00861403209497913));
#45642=CARTESIAN_POINT('Ctrl Pts',(-0.22051388248347,0.00172087463848556,
0.00861332861068179));
#45643=CARTESIAN_POINT('Ctrl Pts',(-0.220514289505427,0.00172059226538401,
0.00861310745220749));
#45644=CARTESIAN_POINT('Ctrl Pts',(-0.220514747001341,0.00172022865110598,
0.00861282031082267));
#45645=CARTESIAN_POINT('Ctrl Pts',(-0.220514873167071,0.00172010829936638,
0.00861272412883551));
#45646=CARTESIAN_POINT('Ctrl Pts',(-0.220515057375285,0.00171980899790886,
0.00861248132013813));
#45647=CARTESIAN_POINT('Ctrl Pts',(-0.220504895339338,0.0131091095836261,
0.00862176289898313));
#45648=CARTESIAN_POINT('Ctrl Pts',(-0.220503204519676,0.013172278658427,
0.00870065757297661));
#45649=CARTESIAN_POINT('Ctrl Pts',(-0.220524686999525,0.0132489243928214,
0.00863835592833102));
#45650=CARTESIAN_POINT('Ctrl Pts',(-0.220393730780806,0.0131269580310319,
0.00860539375055619));
#45651=CARTESIAN_POINT('Ctrl Pts',(-0.220392045709976,0.0131903179698247,
0.0086841360040918));
#45652=CARTESIAN_POINT('Ctrl Pts',(-0.22041353202268,0.0132668117899861,
0.00862164844129692));
#45653=CARTESIAN_POINT('Ctrl Pts',(-0.220184614434698,0.0131663208471479,
0.00856955272821915));
#45654=CARTESIAN_POINT('Ctrl Pts',(-0.220183091286059,0.0132300952247244,
0.00864807418559056));
#45655=CARTESIAN_POINT('Ctrl Pts',(-0.220190375822233,0.0133093870456292,
0.00858224595417015));
#45656=CARTESIAN_POINT('Ctrl Pts',(-0.219784302265126,0.0131135141202054,
0.00860522420992131));
#45657=CARTESIAN_POINT('Ctrl Pts',(-0.219783539999466,0.0131767153162485,
0.00868397549414707));
#45658=CARTESIAN_POINT('Ctrl Pts',(-0.219739129146227,0.0132501816669398,
0.00862323219516294));
#45659=CARTESIAN_POINT('Ctrl Pts',(-0.219485674564641,0.0129837568423567,
0.00870181479506232));
#45660=CARTESIAN_POINT('Ctrl Pts',(-0.219484575843822,0.0130454250762007,
0.0087816185864055));
#45661=CARTESIAN_POINT('Ctrl Pts',(-0.219437547728755,0.013115180181397,
0.00872598545329776));
#45662=CARTESIAN_POINT('Ctrl Pts',(-0.219285266042446,0.0128973209402166,
0.00876279522307528));
#45663=CARTESIAN_POINT('Ctrl Pts',(-0.219284139925531,0.0129580035698831,
0.00884334030755273));
#45664=CARTESIAN_POINT('Ctrl Pts',(-0.21923709929106,0.0130284151484448,
0.00878856304375625));
#45665=CARTESIAN_POINT('Ctrl Pts',(-0.220398946890659,0.0131276359028523,
0.00860743040991009));
#45666=CARTESIAN_POINT('Ctrl Pts',(-0.220398971642014,0.0131321314775003,
0.00861284084588095));
#45667=CARTESIAN_POINT('Ctrl Pts',(-0.220399881495722,0.013137006554187,
0.00861781950952909));
#45668=CARTESIAN_POINT('Ctrl Pts',(-0.220403652945788,0.0131482971438847,
0.00862767263867194));
#45669=CARTESIAN_POINT('Ctrl Pts',(-0.220406804708496,0.0131546746445743,
0.00863220881639067));
#45670=CARTESIAN_POINT('Ctrl Pts',(-0.220417285354963,0.0131715709114628,
0.00864208462491169));
#45671=CARTESIAN_POINT('Ctrl Pts',(-0.220426267100991,0.0131825846100448,
0.0086463614567408));
#45672=CARTESIAN_POINT('Ctrl Pts',(-0.220451830128197,0.0132080184642301,
0.00865141595330123));
#45673=CARTESIAN_POINT('Ctrl Pts',(-0.220469419124149,0.0132219431230173,
0.00865059776196831));
#45674=CARTESIAN_POINT('Ctrl Pts',(-0.22049334815256,0.0132371769667726,
0.00864495572013383));
#45675=CARTESIAN_POINT('Ctrl Pts',(-0.220498115179498,0.0132400462236785,
0.00864362986672573));
#45676=CARTESIAN_POINT('Ctrl Pts',(-0.220505238671295,0.0132441039903126,
0.00864135545795626));
#45677=CARTESIAN_POINT('Ctrl Pts',(-0.220507582366072,0.0132454010942176,
0.00864056065067561));
#45678=CARTESIAN_POINT('Ctrl Pts',(-0.220511137605847,0.0132473236276702,
0.00863927732404243));
#45679=CARTESIAN_POINT('Ctrl Pts',(-0.220512314305617,0.013247950397367,
0.00863883918371931));
#45680=CARTESIAN_POINT('Ctrl Pts',(-0.220513986335453,0.0132488496923406,
0.00863818618337553));
#45681=CARTESIAN_POINT('Ctrl Pts',(-0.220514656898247,0.0132492117024941,
0.00863791682953718));
#45682=CARTESIAN_POINT('Ctrl Pts',(-0.220515400278411,0.0132496510473206,
0.00863758226858773));
#45683=CARTESIAN_POINT('Ctrl Pts',(-0.220515602204728,0.0132497815996683,
0.00863748127580821));
#45684=CARTESIAN_POINT('Ctrl Pts',(-0.220515865363209,0.0132499845085129,
0.00863732249765459));
#45685=CARTESIAN_POINT('Ctrl Pts',(-0.220515947525014,0.0132500624648397,
0.00863726079027726));
#45686=CARTESIAN_POINT('Ctrl Pts',(-0.220516099934179,0.0132503125103766,
0.00863705970261241));
#45687=CARTESIAN_POINT('Ctrl Pts',(-0.2202504135532,0.00812534913742659,
0.0106634322264908));
#45688=CARTESIAN_POINT('Ctrl Pts',(-0.220147977225147,0.00813374905043262,
0.0106623784596957));
#45689=CARTESIAN_POINT('Ctrl Pts',(-0.220151169572582,0.00812650208014952,
0.010559914278616));
#45690=CARTESIAN_POINT('Ctrl Pts',(-0.220133573386841,0.00688792809120517,
0.0107484830823553));
#45691=CARTESIAN_POINT('Ctrl Pts',(-0.220031425127958,0.0068989046609728,
0.010748807990965));
#45692=CARTESIAN_POINT('Ctrl Pts',(-0.220034649032527,0.00690588109330772,
0.0106453391107511));
#45693=CARTESIAN_POINT('Ctrl Pts',(-0.219994804021819,0.00506747611300468,
0.0104977512748514));
#45694=CARTESIAN_POINT('Ctrl Pts',(-0.219891389349097,0.00506853282168791,
0.010499938160873));
#45695=CARTESIAN_POINT('Ctrl Pts',(-0.219894504064411,0.00509592002633516,
0.0103992372092036));
#45696=CARTESIAN_POINT('Ctrl Pts',(-0.220203419609321,0.00275378968309817,
0.00942103991272318));
#45697=CARTESIAN_POINT('Ctrl Pts',(-0.220101811139137,0.00273816330361558,
0.00941287454677868));
#45698=CARTESIAN_POINT('Ctrl Pts',(-0.220104476366608,0.00279222836967903,
0.00932461133402498));
#45699=CARTESIAN_POINT('Ctrl Pts',(-0.220503433261061,0.00177703780097305,
0.00869404760028399));
#45700=CARTESIAN_POINT('Ctrl Pts',(-0.220403503423106,0.00175796626419382,
0.00867923883869439));
#45701=CARTESIAN_POINT('Ctrl Pts',(-0.22040590406413,0.00182286455694324,
0.00859915204344728));
#45702=CARTESIAN_POINT('Ctrl Pts',(-0.220649949295114,0.00125070731346161,
0.0082007135299242));
#45703=CARTESIAN_POINT('Ctrl Pts',(-0.220549235546056,0.00123534032793399,
0.00818683084179405));
#45704=CARTESIAN_POINT('Ctrl Pts',(-0.220551438904638,0.00130625601097892,
0.00811242254542717));
#45705=CARTESIAN_POINT('Ctrl Pts',(-0.220093674791071,0.0074975850117286,
0.0105819125063979));
#45706=CARTESIAN_POINT('Ctrl Pts',(-0.220093526920449,0.00749758320628809,
0.0105884551073401));
#45707=CARTESIAN_POINT('Ctrl Pts',(-0.220094024045747,0.007497581232436,
0.0105949960431337));
#45708=CARTESIAN_POINT('Ctrl Pts',(-0.220096365411539,0.00749757686947963,
0.0106082955073979));
#45709=CARTESIAN_POINT('Ctrl Pts',(-0.220098286603548,0.00749757447419758,
0.0106150042638252));
#45710=CARTESIAN_POINT('Ctrl Pts',(-0.220105708909756,0.00749756733743141,
0.0106334048657344));
#45711=CARTESIAN_POINT('Ctrl Pts',(-0.220112794418493,0.00749756240258949,
0.0106443048720408));
#45712=CARTESIAN_POINT('Ctrl Pts',(-0.220130709373825,0.00749755245577472,
0.0106628288801252));
#45713=CARTESIAN_POINT('Ctrl Pts',(-0.220141372895899,0.00749754755040115,
0.0106702784560354));
#45714=CARTESIAN_POINT('Ctrl Pts',(-0.220172671231308,0.00749753517796745,
0.0106841865494111));
#45715=CARTESIAN_POINT('Ctrl Pts',(-0.220189205266996,0.00749757396411134,
0.0106840868768587));
#45716=CARTESIAN_POINT('Ctrl Pts',(-0.220191303401166,0.00749750031916177,
0.0106841483771092));
#45717=CARTESIAN_POINT('Ctrl Pts',(-0.220191746640651,0.00749753084563371,
0.0106841591947775));
#45718=CARTESIAN_POINT('Ctrl Pts',(-0.220150708821755,0.00687195702680685,
0.010559884303056));
#45719=CARTESIAN_POINT('Ctrl Pts',(-0.22014759399109,0.00686468413303138,
0.0106625473046195));
#45720=CARTESIAN_POINT('Ctrl Pts',(-0.220250229267773,0.0068730627295562,
0.0106633257059033));
#45721=CARTESIAN_POINT('Ctrl Pts',(-0.220034720928684,0.00808612268880879,
0.0106450343427239));
#45722=CARTESIAN_POINT('Ctrl Pts',(-0.220031574719443,0.00809303072895467,
0.0107486971037965));
#45723=CARTESIAN_POINT('Ctrl Pts',(-0.220133932562721,0.00810398139678503,
0.0107480825139144));
#45724=CARTESIAN_POINT('Ctrl Pts',(-0.219898939957643,0.00988609461928639,
0.0104026796240758));
#45725=CARTESIAN_POINT('Ctrl Pts',(-0.219895900748701,0.00991331796087509,
0.0105036180132768));
#45726=CARTESIAN_POINT('Ctrl Pts',(-0.219999481369186,0.0099141547094306,
0.0105012650911866));
#45727=CARTESIAN_POINT('Ctrl Pts',(-0.220104216028228,0.0121807920431273,
0.00934034778981266));
#45728=CARTESIAN_POINT('Ctrl Pts',(-0.220101623005436,0.0122346429002561,
0.00942896565106837));
#45729=CARTESIAN_POINT('Ctrl Pts',(-0.220203474394453,0.0122190459273884,
0.00943671421502881));
#45730=CARTESIAN_POINT('Ctrl Pts',(-0.220406547486447,0.0131480054901679,
0.00862237289776044));
#45731=CARTESIAN_POINT('Ctrl Pts',(-0.220404214515825,0.0132126844151198,
0.00870289002102647));
#45732=CARTESIAN_POINT('Ctrl Pts',(-0.220504233003487,0.0131929487356747,
0.00871771614458468));
#45733=CARTESIAN_POINT('Ctrl Pts',(-0.220553604100269,0.0136631541416016,
0.00814156304176045));
#45734=CARTESIAN_POINT('Ctrl Pts',(-0.220551464853133,0.0137338357445961,
0.00821646744183325));
#45735=CARTESIAN_POINT('Ctrl Pts',(-0.22065234139264,0.0137181149325072,
0.00823021086189709));
#45736=CARTESIAN_POINT('Ctrl Pts',(-0.217137874468735,0.008030785389101,
0.0104987600271184));
#45737=CARTESIAN_POINT('Ctrl Pts',(-0.217135999376533,0.00803730846625089,
0.010607296817054));
#45738=CARTESIAN_POINT('Ctrl Pts',(-0.217028124738702,0.00804529143374969,
0.0105958336575828));
#45739=CARTESIAN_POINT('Ctrl Pts',(-0.217053923565904,0.00696476469087671,
0.0105605954778132));
#45740=CARTESIAN_POINT('Ctrl Pts',(-0.217052029443782,0.00695824947239747,
0.0106699234267572));
#45741=CARTESIAN_POINT('Ctrl Pts',(-0.216944400117764,0.00696910854709431,
0.0106593295604461));
#45742=CARTESIAN_POINT('Ctrl Pts',(-0.216834795596937,0.0048122033769108,
0.0102961809446762));
#45743=CARTESIAN_POINT('Ctrl Pts',(-0.216833012543114,0.00478002238563605,
0.010402360493829));
#45744=CARTESIAN_POINT('Ctrl Pts',(-0.216723776467451,0.00478370698650778,
0.0103954490239756));
#45745=CARTESIAN_POINT('Ctrl Pts',(-0.217137701377203,0.00290143240652124,
0.00932526468848566));
#45746=CARTESIAN_POINT('Ctrl Pts',(-0.217136369590972,0.00284578989718424,
0.00941959858197015));
#45747=CARTESIAN_POINT('Ctrl Pts',(-0.217029631656927,0.00283459991226262,
0.00940110164852008));
#45748=CARTESIAN_POINT('Ctrl Pts',(-0.217300533120515,0.00206565219928745,
0.00869660496702258));
#45749=CARTESIAN_POINT('Ctrl Pts',(-0.217299461055391,0.00200015998946544,
0.00878340995987883));
#45750=CARTESIAN_POINT('Ctrl Pts',(-0.21719227419963,0.00199426821917551,
0.0087660056028655));
#45751=CARTESIAN_POINT('Ctrl Pts',(-0.217213240235122,0.00253454644557544,
0.00902670532692319));
#45752=CARTESIAN_POINT('Ctrl Pts',(-0.217213132107947,0.00253076598515692,
0.00903238191218357));
#45753=CARTESIAN_POINT('Ctrl Pts',(-0.217212380884729,0.0025266614085604,
0.00903779101041478));
#45754=CARTESIAN_POINT('Ctrl Pts',(-0.217209531777293,0.00251761914705192,
0.00904828662234579));
#45755=CARTESIAN_POINT('Ctrl Pts',(-0.217207353950518,0.00251268911402758,
0.00905326629660996));
#45756=CARTESIAN_POINT('Ctrl Pts',(-0.217199347813401,0.00249824154810511,
0.0090659359008687));
#45757=CARTESIAN_POINT('Ctrl Pts',(-0.217192101359339,0.00248855360873053,
0.0090722069176123));
#45758=CARTESIAN_POINT('Ctrl Pts',(-0.217174446526582,0.00246944770445475,
0.00908065823763552));
#45759=CARTESIAN_POINT('Ctrl Pts',(-0.217164116546706,0.00246020276307118,
0.00908266823978674));
#45760=CARTESIAN_POINT('Ctrl Pts',(-0.217144135035235,0.00244514628396083,
0.00908235046140921));
#45761=CARTESIAN_POINT('Ctrl Pts',(-0.217134775069224,0.00243902751563067,
0.00908076767243162));
#45762=CARTESIAN_POINT('Ctrl Pts',(-0.217123400409096,0.00243272926083712,
0.0090773181822219));
#45763=CARTESIAN_POINT('Ctrl Pts',(-0.217121274018224,0.00243155301768911,
0.00907658389939519));
#45764=CARTESIAN_POINT('Ctrl Pts',(-0.217119277829696,0.00243052048892982,
0.0090758545613406));
#45765=CARTESIAN_POINT('Ctrl Pts',(-0.217094602388958,0.00749884757784041,
0.0105144330190784));
#45766=CARTESIAN_POINT('Ctrl Pts',(-0.21709443736718,0.0074988465877603,
0.0105208742316926));
#45767=CARTESIAN_POINT('Ctrl Pts',(-0.217093648086457,0.00749884575649302,
0.0105272842319109));
#45768=CARTESIAN_POINT('Ctrl Pts',(-0.217090731117228,0.00749884434847888,
0.0105403659619601));
#45769=CARTESIAN_POINT('Ctrl Pts',(-0.217088509644837,0.00749884380187818,
0.0105469808193619));
#45770=CARTESIAN_POINT('Ctrl Pts',(-0.217080266789553,0.00749884271946781,
0.0105650264924206));
#45771=CARTESIAN_POINT('Ctrl Pts',(-0.217072698879009,0.00749884263169673,
0.0105755954190497));
#45772=CARTESIAN_POINT('Ctrl Pts',(-0.2170539717794,0.00749884292283719,
0.0105932912156081));
#45773=CARTESIAN_POINT('Ctrl Pts',(-0.21704298650683,0.0074988437000847,
0.0106002517588459));
#45774=CARTESIAN_POINT('Ctrl Pts',(-0.217019111256083,0.00749884076347341,
0.0106095973639871));
#45775=CARTESIAN_POINT('Ctrl Pts',(-0.217008118866313,0.00749888689621046,
0.0106113615914812));
#45776=CARTESIAN_POINT('Ctrl Pts',(-0.216997761731594,0.0074987818105982,
0.0106118145058692));
#45777=CARTESIAN_POINT('Ctrl Pts',(-0.216995371561048,0.00749881704992926,
0.0106118871769746));
#45778=CARTESIAN_POINT('Ctrl Pts',(-0.216992988389039,0.00749886191827281,
0.0106118645637799));
#45779=CARTESIAN_POINT('Ctrl Pts',(-0.216992039555683,0.0074988622638103,
0.0106118431559742));
#45780=CARTESIAN_POINT('Ctrl Pts',(-0.217307543356349,0.0129460293259321,
0.00868783863166776));
#45781=CARTESIAN_POINT('Ctrl Pts',(-0.217306819903283,0.013011671669317,
0.00877462975554483));
#45782=CARTESIAN_POINT('Ctrl Pts',(-0.217199541099427,0.0130177509641774,
0.00875739725535199));
#45783=CARTESIAN_POINT('Ctrl Pts',(-0.217142206976129,0.0120960223538591,
0.00932778214574832));
#45784=CARTESIAN_POINT('Ctrl Pts',(-0.217141217622965,0.0121516216063133,
0.00942224602098435));
#45785=CARTESIAN_POINT('Ctrl Pts',(-0.217034385733589,0.0121629501148438,
0.00940397474918907));
#45786=CARTESIAN_POINT('Ctrl Pts',(-0.216836257913023,0.010185646463759,
0.0102967050880177));
#45787=CARTESIAN_POINT('Ctrl Pts',(-0.216834826013361,0.010217830511706,
0.0104029574503101));
#45788=CARTESIAN_POINT('Ctrl Pts',(-0.216725490864702,0.0102144787022243,
0.0103962399214122));
#45789=CARTESIAN_POINT('Ctrl Pts',(-0.217054853915967,0.00802435938547715,
0.0105612587075268));
#45790=CARTESIAN_POINT('Ctrl Pts',(-0.217053305388005,0.00803077937328534,
0.0106706759148725));
#45791=CARTESIAN_POINT('Ctrl Pts',(-0.216945574819892,0.00801993045571461,
0.0106603452175849));
#45792=CARTESIAN_POINT('Ctrl Pts',(-0.217138149622957,0.00696060513773728,
0.0104977725037612));
#45793=CARTESIAN_POINT('Ctrl Pts',(-0.217136621510629,0.00695400059961224,
0.010606380722123));
#45794=CARTESIAN_POINT('Ctrl Pts',(-0.217028641347721,0.00694608024100671,
0.0105951772770944));
#45795=CARTESIAN_POINT('Ctrl Pts',(-0.217217404929227,0.0124620146248922,
0.00902905891344479));
#45796=CARTESIAN_POINT('Ctrl Pts',(-0.217217292950013,0.0124659537352925,
0.00903497088109792));
#45797=CARTESIAN_POINT('Ctrl Pts',(-0.217216495254757,0.0124703056948511,
0.00904054042042587));
#45798=CARTESIAN_POINT('Ctrl Pts',(-0.217213467856878,0.0124800507372417,
0.00905123743169844));
#45799=CARTESIAN_POINT('Ctrl Pts',(-0.217211148470925,0.0124854342259932,
0.00905622188096938));
#45800=CARTESIAN_POINT('Ctrl Pts',(-0.21720293947776,0.0125008317760289,
0.00906822295320578));
#45801=CARTESIAN_POINT('Ctrl Pts',(-0.217195796422827,0.0125110476227904,
0.00907375635273045));
#45802=CARTESIAN_POINT('Ctrl Pts',(-0.217178399375296,0.0125317585520276,
0.00908079249600287));
#45803=CARTESIAN_POINT('Ctrl Pts',(-0.217168102183229,0.0125420742072453,
0.0090819563423573));
#45804=CARTESIAN_POINT('Ctrl Pts',(-0.217140656078641,0.0125658047878956,
0.00907922929733444));
#45805=CARTESIAN_POINT('Ctrl Pts',(-0.217127225849111,0.0125741931915602,
0.00907284312855735));
#45806=CARTESIAN_POINT('Ctrl Pts',(-0.217125518265942,0.012575247500853,
0.00907211843792538));
#45807=CARTESIAN_POINT('Ctrl Pts',(-0.217125430481138,0.0125753249905193,
0.00907206576885612));
#45808=CARTESIAN_POINT('Ctrl Pts',(-0.217125136225254,0.0125755132818,0.00907193395437536));
#45809=CARTESIAN_POINT('Ctrl Pts',(-0.218505927384742,0.00219420861527787,
0.00893903540143742));
#45810=CARTESIAN_POINT('Ctrl Pts',(-0.218506576680989,0.00227829750388311,
0.00900996719729256));
#45811=CARTESIAN_POINT('Ctrl Pts',(-0.218508231183922,0.00234104950524819,
0.00892018804324298));
#45812=CARTESIAN_POINT('Ctrl Pts',(-0.218245421085756,0.0022043243771477,
0.0089411823686304));
#45813=CARTESIAN_POINT('Ctrl Pts',(-0.2182472119187,0.0022867159623372,
0.00901075868610424));
#45814=CARTESIAN_POINT('Ctrl Pts',(-0.218249117191188,0.00234931542687908,
0.00892093265387189));
#45815=CARTESIAN_POINT('Ctrl Pts',(-0.217712828506656,0.00217687540292711,
0.00891143052286725));
#45816=CARTESIAN_POINT('Ctrl Pts',(-0.217704611098061,0.00226956574195701,
0.00898827016224622));
#45817=CARTESIAN_POINT('Ctrl Pts',(-0.217705766229126,0.0023324873031235,
0.0088983393941371));
#45818=CARTESIAN_POINT('Ctrl Pts',(-0.217210903661233,0.00234921543953796,
0.00902402719766558));
#45819=CARTESIAN_POINT('Ctrl Pts',(-0.217284478791233,0.00241352385102592,
0.00907980326016165));
#45820=CARTESIAN_POINT('Ctrl Pts',(-0.217285575413226,0.0024746238390022,
0.00898952645001293));
#45821=CARTESIAN_POINT('Ctrl Pts',(-0.217008784931119,0.00249299341869297,
0.00911473622767726));
#45822=CARTESIAN_POINT('Ctrl Pts',(-0.217066036533421,0.00256425859926955,
0.00917304859362285));
#45823=CARTESIAN_POINT('Ctrl Pts',(-0.217067500167738,0.00262345357409097,
0.00908135538656866));
#45824=CARTESIAN_POINT('Ctrl Pts',(-0.218256634048459,0.00234470650638891,
0.00891994458535368));
#45825=CARTESIAN_POINT('Ctrl Pts',(-0.218256626639177,0.00234040530459759,
0.00892588558602306));
#45826=CARTESIAN_POINT('Ctrl Pts',(-0.218257578582534,0.00233552000606212,
0.0089312472304899));
#45827=CARTESIAN_POINT('Ctrl Pts',(-0.218261540417236,0.00232380224523273,
0.00894167585285985));
#45828=CARTESIAN_POINT('Ctrl Pts',(-0.218264856613629,0.00231697352292472,
0.00894629386253098));
#45829=CARTESIAN_POINT('Ctrl Pts',(-0.218275580156686,0.00229875209470095,
0.00895589403300023));
#45830=CARTESIAN_POINT('Ctrl Pts',(-0.218284702888905,0.00228640941556886,
0.00895969840013095));
#45831=CARTESIAN_POINT('Ctrl Pts',(-0.218306314313981,0.00226165582803696,
0.00896251059574449));
#45832=CARTESIAN_POINT('Ctrl Pts',(-0.218317875037794,0.00225009136726339,
0.00896169726079228));
#45833=CARTESIAN_POINT('Ctrl Pts',(-0.218341505795055,0.00222871318891932,
0.00895689458922));
#45834=CARTESIAN_POINT('Ctrl Pts',(-0.218353842689428,0.00221868141491273,
0.00895283427796545));
#45835=CARTESIAN_POINT('Ctrl Pts',(-0.218368730666572,0.00220769525572976,
0.0089463082783215));
#45836=CARTESIAN_POINT('Ctrl Pts',(-0.218371385735275,0.00220579459015017,
0.00894509374435352));
#45837=CARTESIAN_POINT('Ctrl Pts',(-0.218374005680645,0.00220395032896211,
0.00894382649250058));
#45838=CARTESIAN_POINT('Ctrl Pts',(-0.218489629254318,0.012611151918198,
0.00895310221279096));
#45839=CARTESIAN_POINT('Ctrl Pts',(-0.218487674841287,0.0126745742874925,
0.00904502916129814));
#45840=CARTESIAN_POINT('Ctrl Pts',(-0.218504904302657,0.0127576089696995,
0.00897317862838708));
#45841=CARTESIAN_POINT('Ctrl Pts',(-0.218222750307536,0.012661502377565,
0.00891280999119246));
#45842=CARTESIAN_POINT('Ctrl Pts',(-0.218220592929847,0.0127255073996101,
0.00900432897252887));
#45843=CARTESIAN_POINT('Ctrl Pts',(-0.218253673945024,0.0128079644187064,
0.00893229925480229));
#45844=CARTESIAN_POINT('Ctrl Pts',(-0.217766142708494,0.0126829340915357,
0.00888986543619831));
#45845=CARTESIAN_POINT('Ctrl Pts',(-0.217765157221868,0.0127472329221916,
0.00898121583622291));
#45846=CARTESIAN_POINT('Ctrl Pts',(-0.217717535145496,0.0128304182181186,
0.00890691214413009));
#45847=CARTESIAN_POINT('Ctrl Pts',(-0.217283803131409,0.0124821711351596,
0.00901759047954861));
#45848=CARTESIAN_POINT('Ctrl Pts',(-0.217282399769762,0.0125439262817006,
0.00911041470209943));
#45849=CARTESIAN_POINT('Ctrl Pts',(-0.217240271304298,0.012620944820576,
0.009044103947773));
#45850=CARTESIAN_POINT('Ctrl Pts',(-0.217043935029806,0.0124005232817256,
0.00906509087384854));
#45851=CARTESIAN_POINT('Ctrl Pts',(-0.217042471015379,0.012461219665155,
0.0091586465875576));
#45852=CARTESIAN_POINT('Ctrl Pts',(-0.217000060226919,0.0125405600879245,
0.00909203027864609));
#45853=CARTESIAN_POINT('Ctrl Pts',(-0.218253210572638,0.0126493218644601,
0.00892398112026186));
#45854=CARTESIAN_POINT('Ctrl Pts',(-0.218255261351961,0.0126731190888775,
0.00895794646059297));
#45855=CARTESIAN_POINT('Ctrl Pts',(-0.218298695621072,0.0127283794650483,
0.00899134738316015));
#45856=CARTESIAN_POINT('Ctrl Pts',(-0.218374738263889,0.0127707341741232,
0.0089594649654453));
#45857=CARTESIAN_POINT('Ctrl Pts',(-0.218370607902533,0.00180941438383972,
0.00851604478529543));
#45858=CARTESIAN_POINT('Ctrl Pts',(-0.218368285855028,0.00174473477363733,
0.00859546721180872));
#45859=CARTESIAN_POINT('Ctrl Pts',(-0.218469416891288,0.00175757178993804,
0.00860579739743824));
#45860=CARTESIAN_POINT('Ctrl Pts',(-0.218268644565581,0.00230105693080552,
0.00891381537685727));
#45861=CARTESIAN_POINT('Ctrl Pts',(-0.218266160139693,0.00224200310180626,
0.00899779099512986));
#45862=CARTESIAN_POINT('Ctrl Pts',(-0.218366775119483,0.00225777155667148,
0.00900884727234041));
#45863=CARTESIAN_POINT('Ctrl Pts',(-0.218048286160621,0.00322871717535582,
0.00951870881413451));
#45864=CARTESIAN_POINT('Ctrl Pts',(-0.218045567620402,0.00317998919478594,
0.00960947751407076));
#45865=CARTESIAN_POINT('Ctrl Pts',(-0.21814730176867,0.00319244194660178,
0.00961555565315444));
#45866=CARTESIAN_POINT('Ctrl Pts',(-0.217912216784612,0.0053435724410554,
0.0103893198794707));
#45867=CARTESIAN_POINT('Ctrl Pts',(-0.217909140610329,0.00531923057262254,
0.0104901173983572));
#45868=CARTESIAN_POINT('Ctrl Pts',(-0.218012029342262,0.00531695415747033,
0.0104884940391751));
#45869=CARTESIAN_POINT('Ctrl Pts',(-0.218040501648908,0.00696434230067764,
0.0105877544423164));
#45870=CARTESIAN_POINT('Ctrl Pts',(-0.218037334717472,0.00695806260383963,
0.0106907323437167));
#45871=CARTESIAN_POINT('Ctrl Pts',(-0.218139167571268,0.00694719575757316,
0.0106907713966397));
#45872=CARTESIAN_POINT('Ctrl Pts',(-0.218146972284269,0.00806696358112366,
0.0105188716989655));
#45873=CARTESIAN_POINT('Ctrl Pts',(-0.218143831668603,0.00807348051114177,
0.0106210514411844));
#45874=CARTESIAN_POINT('Ctrl Pts',(-0.218245905616467,0.00806488518621087,
0.0106223363913482));
#45875=CARTESIAN_POINT('Ctrl Pts',(-0.218192328422137,0.00749852093264668,
0.0106389711280447));
#45876=CARTESIAN_POINT('Ctrl Pts',(-0.218154305198807,0.00749977351117825,
0.0106381083927364));
#45877=CARTESIAN_POINT('Ctrl Pts',(-0.218121877726077,0.0075010566023537,
0.0106133985656208));
#45878=CARTESIAN_POINT('Ctrl Pts',(-0.218107640643032,0.00750094174584491,
0.0105885860309675));
#45879=CARTESIAN_POINT('Ctrl Pts',(-0.218097197572745,0.00750085749722526,
0.0105703857407404));
#45880=CARTESIAN_POINT('Ctrl Pts',(-0.218094029662777,0.0075002408200837,
0.0105524183613623));
#45881=CARTESIAN_POINT('Ctrl Pts',(-0.218094302901274,0.00749931921466459,
0.0105367255362189));
#45882=CARTESIAN_POINT('Origin',(-0.22171405081414,0.00791637279634685,
0.00318516322693479));
#45883=CARTESIAN_POINT('Ctrl Pts',(-0.215138270481614,0.00801653871855295,
0.0104545941803276));
#45884=CARTESIAN_POINT('Ctrl Pts',(-0.215136339530633,0.00802279480318382,
0.0105617554450719));
#45885=CARTESIAN_POINT('Ctrl Pts',(-0.215029738537428,0.0080309281096567,
0.0105517178004985));
#45886=CARTESIAN_POINT('Ctrl Pts',(-0.215054199654782,0.00697916618023934,
0.01051252586723));
#45887=CARTESIAN_POINT('Ctrl Pts',(-0.21505225151283,0.00697293458855082,
0.0106204169830234));
#45888=CARTESIAN_POINT('Ctrl Pts',(-0.214945874857355,0.00698382690371717,
0.0106113028447007));
#45889=CARTESIAN_POINT('Ctrl Pts',(-0.214841833023336,0.0048911525456576,
0.010264819707883));
#45890=CARTESIAN_POINT('Ctrl Pts',(-0.214839984604383,0.00486043155357993,
0.0103698241720069));
#45891=CARTESIAN_POINT('Ctrl Pts',(-0.214732132555284,0.00486330753472638,
0.0103638864488541));
#45892=CARTESIAN_POINT('Ctrl Pts',(-0.215123102029791,0.00301006841920348,
0.00934454242151527));
#45893=CARTESIAN_POINT('Ctrl Pts',(-0.215121678625563,0.00295659535466086,
0.00943847740912549));
#45894=CARTESIAN_POINT('Ctrl Pts',(-0.215015965458248,0.0029460175374489,
0.00942222581375646));
#45895=CARTESIAN_POINT('Ctrl Pts',(-0.215268667797406,0.00217542510416371,
0.00873918816030454));
#45896=CARTESIAN_POINT('Ctrl Pts',(-0.215267493810616,0.00211227092821834,
0.008825991556164));
#45897=CARTESIAN_POINT('Ctrl Pts',(-0.215161402439874,0.0021063441397646,
0.0088106397707087));
#45898=CARTESIAN_POINT('Ctrl Pts',(-0.215095387779062,0.00254083911603525,
0.00910817608666392));
#45899=CARTESIAN_POINT('Ctrl Pts',(-0.21512037463289,0.00256400002101044,
0.00912360420379185));
#45900=CARTESIAN_POINT('Ctrl Pts',(-0.215133745878006,0.00258169558032891,
0.00912601392496322));
#45901=CARTESIAN_POINT('Ctrl Pts',(-0.215148676560894,0.00260130634252768,
0.00912383356325065));
#45902=CARTESIAN_POINT('Ctrl Pts',(-0.215150273563903,0.00260340393220061,
0.00912360034925493));
#45903=CARTESIAN_POINT('Ctrl Pts',(-0.215151889432577,0.00260554977826508,
0.0091232734480787));
#45904=CARTESIAN_POINT('Ctrl Pts',(-0.215153528948729,0.00260776901397922,
0.00912283471210183));
#45905=CARTESIAN_POINT('Ctrl Pts',(-0.215170496594165,0.00263073628068582,
0.0091182941551298));
#45906=CARTESIAN_POINT('Ctrl Pts',(-0.215184361861634,0.00266180392841244,
0.00909996890792453));
#45907=CARTESIAN_POINT('Ctrl Pts',(-0.21518479796162,0.00267607596988323,
0.00907755560002423));
#45908=CARTESIAN_POINT('Ctrl Pts',(-0.215095211620886,0.00749946305213359,
0.0104691619661793));
#45909=CARTESIAN_POINT('Ctrl Pts',(-0.215095051270524,0.00749946252715341,
0.0104756317925372));
#45910=CARTESIAN_POINT('Ctrl Pts',(-0.215094261018183,0.00749946210845811,
0.0104820704988108));
#45911=CARTESIAN_POINT('Ctrl Pts',(-0.215091337124818,0.00749946144379272,
0.0104951805243167));
#45912=CARTESIAN_POINT('Ctrl Pts',(-0.215089114951798,0.00749946121552005,
0.0105017959519679));
#45913=CARTESIAN_POINT('Ctrl Pts',(-0.215080869890318,0.00749946084296753,
0.0105198422392518));
#45914=CARTESIAN_POINT('Ctrl Pts',(-0.215073300383325,0.00749946096680242,
0.0105304108795332));
#45915=CARTESIAN_POINT('Ctrl Pts',(-0.215054569912047,0.00749946128003418,
0.0105481059791543));
#45916=CARTESIAN_POINT('Ctrl Pts',(-0.21504358277679,0.00749946180673463,
0.0105550659716542));
#45917=CARTESIAN_POINT('Ctrl Pts',(-0.215018712085791,0.00749945861210784,
0.0105647986730059));
#45918=CARTESIAN_POINT('Ctrl Pts',(-0.215007312676018,0.00749948519567766,
0.0105662336960224));
#45919=CARTESIAN_POINT('Ctrl Pts',(-0.214998324007091,0.00749940758554542,
0.0105666280985719));
#45920=CARTESIAN_POINT('Ctrl Pts',(-0.21499598086407,0.00749943731930172,
0.010566697535465));
#45921=CARTESIAN_POINT('Ctrl Pts',(-0.214993636732782,0.00749947573716579,
0.0105666778348444));
#45922=CARTESIAN_POINT('Ctrl Pts',(-0.214992640535139,0.00749947588860775,
0.0105666554240425));
#45923=CARTESIAN_POINT('Ctrl Pts',(-0.215271612902418,0.0128241679430378,
0.00873958050001579));
#45924=CARTESIAN_POINT('Ctrl Pts',(-0.215270600712745,0.0128872591163074,
0.00882634285591854));
#45925=CARTESIAN_POINT('Ctrl Pts',(-0.215164566564404,0.0128933475034878,
0.00881117707783499));
#45926=CARTESIAN_POINT('Ctrl Pts',(-0.215125346805473,0.0119839960519677,
0.00934778460885941));
#45927=CARTESIAN_POINT('Ctrl Pts',(-0.215124083651265,0.0120373410606281,
0.0094417082717187));
#45928=CARTESIAN_POINT('Ctrl Pts',(-0.215018426721982,0.0120480293424221,
0.00942567701482509));
#45929=CARTESIAN_POINT('Ctrl Pts',(-0.214843451277587,0.010112463684472,
0.0102630293596174));
#45930=CARTESIAN_POINT('Ctrl Pts',(-0.214841768792085,0.0101432088582359,
0.0103679387850742));
#45931=CARTESIAN_POINT('Ctrl Pts',(-0.214733973527544,0.0101405822780667,
0.0103621781245389));
#45932=CARTESIAN_POINT('Ctrl Pts',(-0.215054297296728,0.00801821343807021,
0.0105127492974011));
#45933=CARTESIAN_POINT('Ctrl Pts',(-0.215052511950845,0.00802442511231975,
0.0106205721752317));
#45934=CARTESIAN_POINT('Ctrl Pts',(-0.214946184595913,0.00801356394386956,
0.0106117052262838));
#45935=CARTESIAN_POINT('Ctrl Pts',(-0.215138103483795,0.00698312146912351,
0.0104542920384517));
#45936=CARTESIAN_POINT('Ctrl Pts',(-0.215136335928839,0.00697687891345948,
0.0105613808476118));
#45937=CARTESIAN_POINT('Ctrl Pts',(-0.215029785457826,0.0069687779079764,
0.0105515847686282));
#45938=CARTESIAN_POINT('Ctrl Pts',(-0.21518738632965,0.0123215256882542,
0.00907911767190286));
#45939=CARTESIAN_POINT('Ctrl Pts',(-0.215186958732144,0.0123358311960233,
0.00910150651904035));
#45940=CARTESIAN_POINT('Ctrl Pts',(-0.215173114189427,0.0123669940601415,
0.00911976197539705));
#45941=CARTESIAN_POINT('Ctrl Pts',(-0.215156188916878,0.0123899124403107,
0.00912431683714909));
#45942=CARTESIAN_POINT('Ctrl Pts',(-0.215141006736465,0.0124104705129507,
0.00912840260490722));
#45943=CARTESIAN_POINT('Ctrl Pts',(-0.215129055078211,0.0124265747862727,
0.00912637222642325));
#45944=CARTESIAN_POINT('Ctrl Pts',(-0.215106250017454,0.0124489868903362,
0.00911441803181024));
#45945=CARTESIAN_POINT('Ctrl Pts',(-0.215103631701308,0.0124515600899674,
0.00911304553554294));
#45946=CARTESIAN_POINT('Ctrl Pts',(-0.215100882380107,0.0124541833998731,
0.00911149354874494));
#45947=CARTESIAN_POINT('Ctrl Pts',(-0.215098009459442,0.0124568456463797,
0.00910972113216459));
#45948=CARTESIAN_POINT('Origin',(-0.216343132180981,0.00254791657843158,
0.0090181005548472));
#45949=CARTESIAN_POINT('Ctrl Pts',(-0.216191667803065,0.0026370176797586,
0.00907415689238714));
#45950=CARTESIAN_POINT('Ctrl Pts',(-0.216191796566365,0.00262309746236483,
0.00909510774781046));
#45951=CARTESIAN_POINT('Ctrl Pts',(-0.216210204957318,0.00259351228337774,
0.00911334041689735));
#45952=CARTESIAN_POINT('Ctrl Pts',(-0.216228349712416,0.00256888190445406,
0.00911727926076771));
#45953=CARTESIAN_POINT('Ctrl Pts',(-0.21622997958263,0.00256666945679458,
0.00911763307123604));
#45954=CARTESIAN_POINT('Ctrl Pts',(-0.216231607982164,0.00256450993898164,
0.0091179055386048));
#45955=CARTESIAN_POINT('Ctrl Pts',(-0.216233221666543,0.00256242089040709,
0.00911810802884885));
#45956=CARTESIAN_POINT('Ctrl Pts',(-0.216251067152262,0.00253931842564724,
0.00912034733710838));
#45957=CARTESIAN_POINT('Ctrl Pts',(-0.216267135569045,0.00252489955735048,
0.00911810893501753));
#45958=CARTESIAN_POINT('Ctrl Pts',(-0.216295512027883,0.00250229745532596,
0.00910638817612955));
#45959=CARTESIAN_POINT('Ctrl Pts',(-0.216298673982971,0.00249977892995521,
0.00910508214589432));
#45960=CARTESIAN_POINT('Ctrl Pts',(-0.216301989265945,0.00249717858831983,
0.00910360948776118));
#45961=CARTESIAN_POINT('Ctrl Pts',(-0.216305478212088,0.00249450055261697,
0.0091019248989092));
#45962=CARTESIAN_POINT('Origin',(-0.215029763026557,0.0124000795960937,
0.00902581809007369));
#45963=CARTESIAN_POINT('Ctrl Pts',(-0.216308818597444,0.0125017236340575,
0.00910474588717665));
#45964=CARTESIAN_POINT('Ctrl Pts',(-0.216277529676922,0.0124777449670039,
0.00911980894330316));
#45965=CARTESIAN_POINT('Ctrl Pts',(-0.216259955722432,0.0124623601332724,
0.00912198910373754));
#45966=CARTESIAN_POINT('Ctrl Pts',(-0.216242122224109,0.0124407253367735,
0.00912127527717495));
#45967=CARTESIAN_POINT('Ctrl Pts',(-0.21624027025839,0.0124384786154227,
0.0091212011480109));
#45968=CARTESIAN_POINT('Ctrl Pts',(-0.216238415756952,0.0124361530299236,
0.00912105345816178));
#45969=CARTESIAN_POINT('Ctrl Pts',(-0.21623654299763,0.0124337307492349,
0.00912081197832088));
#45970=CARTESIAN_POINT('Ctrl Pts',(-0.21621848869826,0.0124103787999494,
0.00911848399666931));
#45971=CARTESIAN_POINT('Ctrl Pts',(-0.216198675184547,0.0123793078462243,
0.00910311913336652));
#45972=CARTESIAN_POINT('Ctrl Pts',(-0.216195447172136,0.0123631989134075,
0.00908219261644899));
#45973=CARTESIAN_POINT('Ctrl Pts',(-0.216195162186071,0.0123617767313345,
0.00908034511248652));
#45974=CARTESIAN_POINT('Ctrl Pts',(-0.2161950072882,0.012360451903129,0.00907848426629928));
#45975=CARTESIAN_POINT('Ctrl Pts',(-0.216194995682923,0.0123592255510163,
0.0090766289839036));
#45976=CARTESIAN_POINT('Ctrl Pts',(-0.216282811305448,0.00210699698509605,
0.00870789405373815));
#45977=CARTESIAN_POINT('Ctrl Pts',(-0.216280515760285,0.00204578096542595,
0.0087903315284613));
#45978=CARTESIAN_POINT('Ctrl Pts',(-0.216382322956288,0.00205681455673375,
0.00879811835758324));
#45979=CARTESIAN_POINT('Ctrl Pts',(-0.2161336968756,0.00294260178677836,
0.00932798061931376));
#45980=CARTESIAN_POINT('Ctrl Pts',(-0.216131148003743,0.00289072230453424,
0.00941741795418149));
#45981=CARTESIAN_POINT('Ctrl Pts',(-0.216232583643101,0.00290558261026826,
0.00942551757946072));
#45982=CARTESIAN_POINT('Ctrl Pts',(-0.21583544487376,0.00485581975852901,
0.0102857719853994));
#45983=CARTESIAN_POINT('Ctrl Pts',(-0.21583252840372,0.0048259645110555,
0.010386157855722));
#45984=CARTESIAN_POINT('Ctrl Pts',(-0.215936095167298,0.00482604039136546,
0.0103832490778077));
#45985=CARTESIAN_POINT('Ctrl Pts',(-0.216055652321081,0.00699289556514365,
0.0105372650696793));
#45986=CARTESIAN_POINT('Ctrl Pts',(-0.216052599771092,0.00698696979358537,
0.0106404709262405));
#45987=CARTESIAN_POINT('Ctrl Pts',(-0.216154764015332,0.00697690020144171,
0.010640271432368));
#45988=CARTESIAN_POINT('Ctrl Pts',(-0.216139423474306,0.00803607929674203,
0.0104756027513544));
#45989=CARTESIAN_POINT('Ctrl Pts',(-0.216136396349725,0.00804222090374004,
0.0105780850791528));
#45990=CARTESIAN_POINT('Ctrl Pts',(-0.216238791819397,0.00803398924503048,
0.010578878627741));
#45991=CARTESIAN_POINT('Ctrl Pts',(-0.216094905541403,0.00749916574467118,
0.0104915386727778));
#45992=CARTESIAN_POINT('Ctrl Pts',(-0.216094757687043,0.0074991648329644,
0.010498081812457));
#45993=CARTESIAN_POINT('Ctrl Pts',(-0.216095254807929,0.00749916380265483,
0.0105046233037114));
#45994=CARTESIAN_POINT('Ctrl Pts',(-0.216097596140649,0.00749916144150093,
0.0105179238150449));
#45995=CARTESIAN_POINT('Ctrl Pts',(-0.216099517294234,0.00749916010265018,
0.0105246331063143));
#45996=CARTESIAN_POINT('Ctrl Pts',(-0.216106938902494,0.007499155955148,
0.0105430335441308));
#45997=CARTESIAN_POINT('Ctrl Pts',(-0.216114023258208,0.00749915292472183,
0.01055393325295));
#45998=CARTESIAN_POINT('Ctrl Pts',(-0.2161319352607,0.00749914604860085,
0.010572456286503));
#45999=CARTESIAN_POINT('Ctrl Pts',(-0.216142596797795,0.00749914251354345,
0.0105799054483358));
#46000=CARTESIAN_POINT('Ctrl Pts',(-0.216165306353742,0.00749913251202104,
0.0105899977046191));
#46001=CARTESIAN_POINT('Ctrl Pts',(-0.216176121942762,0.00749916225956268,
0.0105925056055666));
#46002=CARTESIAN_POINT('Ctrl Pts',(-0.216187363138591,0.00749908779708458,
0.0105935062401521));
#46003=CARTESIAN_POINT('Ctrl Pts',(-0.216189644461058,0.00749910866675623,
0.0105936746436355));
#46004=CARTESIAN_POINT('Ctrl Pts',(-0.216191923222015,0.00749913622058534,
0.0105937606861201));
#46005=CARTESIAN_POINT('Ctrl Pts',(-0.216192971542667,0.00749913607619458,
0.0105937843838612));
#46006=CARTESIAN_POINT('Ctrl Pts',(-0.216139271434847,0.00696167292438563,
0.0104754199577516));
#46007=CARTESIAN_POINT('Ctrl Pts',(-0.216136032556292,0.0069554754642468,
0.0105781262309377));
#46008=CARTESIAN_POINT('Ctrl Pts',(-0.216238661874465,0.00696368361581323,
0.0105788967963663));
#46009=CARTESIAN_POINT('Ctrl Pts',(-0.216055749080497,0.00800701645360984,
0.0105367407275864));
#46010=CARTESIAN_POINT('Ctrl Pts',(-0.216052485301961,0.00801293344084057,
0.0106401701354799));
#46011=CARTESIAN_POINT('Ctrl Pts',(-0.216154883799805,0.00802300632093563,
0.0106399421743868));
#46012=CARTESIAN_POINT('Ctrl Pts',(-0.215836723914711,0.0101351578949112,
0.010288615649846));
#46013=CARTESIAN_POINT('Ctrl Pts',(-0.215833592413248,0.0101649786171273,
0.0103892619918857));
#46014=CARTESIAN_POINT('Ctrl Pts',(-0.215937391379544,0.010164739474805,
0.0103863667566106));
#46015=CARTESIAN_POINT('Ctrl Pts',(-0.216137685088785,0.0120577995594403,
0.0093274156971316));
#46016=CARTESIAN_POINT('Ctrl Pts',(-0.216134927581704,0.0121098292957299,
0.0094170278487481));
#46017=CARTESIAN_POINT('Ctrl Pts',(-0.216236585824584,0.0120949081867636,
0.00942513537855531));
#46018=CARTESIAN_POINT('Ctrl Pts',(-0.216285885406936,0.0128864817321484,
0.00871227969984319));
#46019=CARTESIAN_POINT('Ctrl Pts',(-0.216283378885618,0.0129477820406068,
0.00879493367149495));
#46020=CARTESIAN_POINT('Ctrl Pts',(-0.216385410595137,0.0129366667576193,
0.00880273281431371));
#46021=CARTESIAN_POINT('Ctrl Pts',(-0.192428879980893,0.0120843945331614,
0.0087649457194958));
#46022=CARTESIAN_POINT('Ctrl Pts',(-0.192427684894032,0.0121357661329368,
0.00885788569507324));
#46023=CARTESIAN_POINT('Ctrl Pts',(-0.192388028297364,0.0122187879722831,
0.00880424655434642));
#46024=CARTESIAN_POINT('Ctrl Pts',(-0.192151323086433,0.0119795060504334,
0.00881770899823756));
#46025=CARTESIAN_POINT('Ctrl Pts',(-0.192149856911976,0.0120295605951977,
0.00891133291804273));
#46026=CARTESIAN_POINT('Ctrl Pts',(-0.192109296359608,0.0121115249848374,
0.00885952921437927));
#46027=CARTESIAN_POINT('Ctrl Pts',(-0.191564603142634,0.0117903694463313,
0.00890698930513747));
#46028=CARTESIAN_POINT('Ctrl Pts',(-0.191564013677017,0.0118387145052195,
0.00900174454816317));
#46029=CARTESIAN_POINT('Ctrl Pts',(-0.191530667510288,0.0119326676422929,
0.00894707674718653));
#46030=CARTESIAN_POINT('Ctrl Pts',(-0.191125489451457,0.0114918545236309,
0.00904483726167067));
#46031=CARTESIAN_POINT('Ctrl Pts',(-0.191124463101182,0.0115367200971647,
0.00914043416370774));
#46032=CARTESIAN_POINT('Ctrl Pts',(-0.191036060600173,0.0115898425845301,
0.00910830917324193));
#46033=CARTESIAN_POINT('Ctrl Pts',(-0.190937349462523,0.0112538014290112,
0.00914481642408066));
#46034=CARTESIAN_POINT('Ctrl Pts',(-0.190936022194301,0.0112957769699949,
0.00924184994069289));
#46035=CARTESIAN_POINT('Ctrl Pts',(-0.190858698051812,0.0113582174074258,
0.0092072657414013));
#46036=CARTESIAN_POINT('Ctrl Pts',(-0.190965604317401,0.0114699046751051,
0.00915921566447933));
#46037=CARTESIAN_POINT('Ctrl Pts',(-0.190965712140185,0.0114693256191559,
0.00915945856588905));
#46038=CARTESIAN_POINT('Ctrl Pts',(-0.19096584960052,0.0114687652071312,
0.00915968912157385));
#46039=CARTESIAN_POINT('Ctrl Pts',(-0.190966623351059,0.0114662430478265,
0.00916070319296896));
#46040=CARTESIAN_POINT('Ctrl Pts',(-0.190967620055349,0.0114644811373346,
0.00916134408901796));
#46041=CARTESIAN_POINT('Ctrl Pts',(-0.190971301001675,0.0114599299463686,
0.00916272534006976));
#46042=CARTESIAN_POINT('Ctrl Pts',(-0.190974434960915,0.011457573567264,
0.00916308429216945));
#46043=CARTESIAN_POINT('Ctrl Pts',(-0.19098349851718,0.0114511312613147,
0.0091634866949268));
#46044=CARTESIAN_POINT('Ctrl Pts',(-0.190993053421979,0.0114456390258318,
0.00916252708498545));
#46045=CARTESIAN_POINT('Ctrl Pts',(-0.191014186860149,0.0114318448089166,
0.00915493967903766));
#46046=CARTESIAN_POINT('Ctrl Pts',(-0.191023959965254,0.0114246414658966,
0.00914875819715902));
#46047=CARTESIAN_POINT('Ctrl Pts',(-0.191038704796521,0.0114114486010586,
0.00913371410696604));
#46048=CARTESIAN_POINT('Ctrl Pts',(-0.191044101370854,0.0114055487134585,
0.00912550309845127));
#46049=CARTESIAN_POINT('Ctrl Pts',(-0.191051294287109,0.0113950265549819,
0.00910780083128093));
#46050=CARTESIAN_POINT('Ctrl Pts',(-0.191053300655896,0.0113904207832051,
0.00909861234382404));
#46051=CARTESIAN_POINT('Ctrl Pts',(-0.191053800278385,0.0113864428152143,
0.00908899053291756));
#46052=CARTESIAN_POINT('Ctrl Pts',(-0.1921323840585,0.0119768370000007,
0.00882020102336473));
#46053=CARTESIAN_POINT('Ctrl Pts',(-0.192132364786965,0.0119786721251219,
0.00882344223574507));
#46054=CARTESIAN_POINT('Ctrl Pts',(-0.192132589966708,0.0119807741225516,
0.0088264991122001));
#46055=CARTESIAN_POINT('Ctrl Pts',(-0.192133582901725,0.0119858894502443,
0.00883275520009954));
#46056=CARTESIAN_POINT('Ctrl Pts',(-0.1921344320636,0.011988948143783,0.00883581682223052));
#46057=CARTESIAN_POINT('Ctrl Pts',(-0.192138118929948,0.0119998831934135,
0.00884502631740865));
#46058=CARTESIAN_POINT('Ctrl Pts',(-0.192142050074175,0.0120085802053719,
0.0088496863821559));
#46059=CARTESIAN_POINT('Ctrl Pts',(-0.192154401339469,0.0120327292412066,
0.00885878096165628));
#46060=CARTESIAN_POINT('Ctrl Pts',(-0.192165255403088,0.0120508336147267,
0.00886133147853749));
#46061=CARTESIAN_POINT('Ctrl Pts',(-0.192196350964399,0.0120972880751649,
0.00885918763376293));
#46062=CARTESIAN_POINT('Ctrl Pts',(-0.192217846207761,0.0121258988100782,
0.00885155820539949));
#46063=CARTESIAN_POINT('Ctrl Pts',(-0.192243109585965,0.0121561496495416,
0.00883674354182499));
#46064=CARTESIAN_POINT('Ctrl Pts',(-0.192245681482551,0.0121592070619706,
0.00883516361505474));
#46065=CARTESIAN_POINT('Ctrl Pts',(-0.192248250704815,0.0121622138291422,
0.00883352725727037));
#46066=CARTESIAN_POINT('Ctrl Pts',(-0.192146287432863,0.007001445991187,
0.00993616740742011));
#46067=CARTESIAN_POINT('Ctrl Pts',(-0.192143234360962,0.0069960223197089,
0.0100379092428061));
#46068=CARTESIAN_POINT('Ctrl Pts',(-0.192244826903568,0.00700429955503233,
0.0100394799668714));
#46069=CARTESIAN_POINT('Ctrl Pts',(-0.192066737897779,0.00796348467110267,
0.00998615353633715));
#46070=CARTESIAN_POINT('Ctrl Pts',(-0.192063663567035,0.00796862002590671,
0.0100884509595953));
#46071=CARTESIAN_POINT('Ctrl Pts',(-0.192165062872102,0.00797874334461845,
0.0100891007288684));
#46072=CARTESIAN_POINT('Ctrl Pts',(-0.191868623073859,0.00992132327542535,
0.00978412510994995));
#46073=CARTESIAN_POINT('Ctrl Pts',(-0.191865654370179,0.00994730546079022,
0.00988429983653193));
#46074=CARTESIAN_POINT('Ctrl Pts',(-0.191968225046628,0.00994788503575821,
0.00988283229722599));
#46075=CARTESIAN_POINT('Ctrl Pts',(-0.192097500947389,0.011726822685467,
0.00900328990038117));
#46076=CARTESIAN_POINT('Ctrl Pts',(-0.192094870340512,0.0117725876792211,
0.00909494068949507));
#46077=CARTESIAN_POINT('Ctrl Pts',(-0.192195977838082,0.0117608643675088,
0.00910140164182352));
#46078=CARTESIAN_POINT('Ctrl Pts',(-0.192204910903453,0.0125394508655713,
0.00849025004975171));
#46079=CARTESIAN_POINT('Ctrl Pts',(-0.192202503077705,0.0125938763574182,
0.00857639379684929));
#46080=CARTESIAN_POINT('Ctrl Pts',(-0.192303866003295,0.0125851484834753,
0.00858255214977472));
#46081=CARTESIAN_POINT('Ctrl Pts',(-0.192104389150085,0.00749606093322131,
0.00994933148053198));
#46082=CARTESIAN_POINT('Ctrl Pts',(-0.192103965966015,0.00749467760198495,
0.00997324747001774));
#46083=CARTESIAN_POINT('Ctrl Pts',(-0.192111877116073,0.00749406236498253,
0.010004922477519));
#46084=CARTESIAN_POINT('Ctrl Pts',(-0.192141205886966,0.00749486189663908,
0.0100289347544931));
#46085=CARTESIAN_POINT('Ctrl Pts',(-0.192157026284705,0.00749529317651977,
0.0100418873522594));
#46086=CARTESIAN_POINT('Ctrl Pts',(-0.192179289265701,0.00749615081568364,
0.010051053680766));
#46087=CARTESIAN_POINT('Ctrl Pts',(-0.192202394110733,0.00749688548776383,
0.0100515763031989));
#46088=CARTESIAN_POINT('Origin',(-0.194644697133607,0.00789563648975762,
0.00208891925293578));
#46089=CARTESIAN_POINT('Ctrl Pts',(-0.191108295474911,0.00749762843016989,
0.00992693903429683));
#46090=CARTESIAN_POINT('Ctrl Pts',(-0.191106599644801,0.00749466645656951,
0.00996733235007675));
#46091=CARTESIAN_POINT('Ctrl Pts',(-0.191068850231782,0.00749416418348105,
0.010026720270591));
#46092=CARTESIAN_POINT('Ctrl Pts',(-0.191002065707968,0.00749708279836953,
0.0100253807384898));
#46093=CARTESIAN_POINT('Origin',(-0.195907470514249,0.00706161748354586,
0.00229602172434024));
#46094=CARTESIAN_POINT('Ctrl Pts',(-0.19224449469211,0.0028417662121083,
0.00883510047266706));
#46095=CARTESIAN_POINT('Ctrl Pts',(-0.192244116214055,0.00284188625041017,
0.00883516237725147));
#46096=CARTESIAN_POINT('Ctrl Pts',(-0.192243945000766,0.00284194509216338,
0.00883519239511538));
#46097=CARTESIAN_POINT('Ctrl Pts',(-0.19224376737675,0.00284200983416614,
0.00883522517817115));
#46098=CARTESIAN_POINT('Ctrl Pts',(-0.192243759668759,0.0028420126509833,
0.00883522660404886));
#46099=CARTESIAN_POINT('Ctrl Pts',(-0.192243661274495,0.00284204870176666,
0.0088352448471908));
#46100=CARTESIAN_POINT('Ctrl Pts',(-0.19224357098158,0.0028420827986193,
0.00883526203851272));
#46101=CARTESIAN_POINT('Ctrl Pts',(-0.192243259650548,0.00284220376464917,
0.00883532282286752));
#46102=CARTESIAN_POINT('Ctrl Pts',(-0.192243040657529,0.00284229483416492,
0.00883536823330852));
#46103=CARTESIAN_POINT('Ctrl Pts',(-0.19224234559644,0.00284260145477907,
0.00883552013874578));
#46104=CARTESIAN_POINT('Ctrl Pts',(-0.192241878182314,0.00284283467675889,
0.0088356342547113));
#46105=CARTESIAN_POINT('Ctrl Pts',(-0.192232081281346,0.00284818838957794,
0.00883822897286899));
#46106=CARTESIAN_POINT('Ctrl Pts',(-0.192217537131995,0.00286541958630876,
0.0088462686043001));
#46107=CARTESIAN_POINT('Ctrl Pts',(-0.192183195336512,0.00290883611484725,
0.00885719354998073));
#46108=CARTESIAN_POINT('Ctrl Pts',(-0.192167532798987,0.00293086406224391,
0.00885906951994799));
#46109=CARTESIAN_POINT('Ctrl Pts',(-0.192144790319268,0.00296657424698169,
0.00885489827767933));
#46110=CARTESIAN_POINT('Ctrl Pts',(-0.192136926370917,0.00298050245508833,
0.00885062267327234));
#46111=CARTESIAN_POINT('Ctrl Pts',(-0.192128608339638,0.00299808673321409,
0.00884076917177549));
#46112=CARTESIAN_POINT('Ctrl Pts',(-0.192126244627568,0.0030037842653694,
0.00883666173174214));
#46113=CARTESIAN_POINT('Ctrl Pts',(-0.192123326144348,0.0030129383334435,
0.00882759558586231));
#46114=CARTESIAN_POINT('Ctrl Pts',(-0.192122534580363,0.00301651956758922,
0.00882306590260883));
#46115=CARTESIAN_POINT('Ctrl Pts',(-0.192122335498293,0.00301948148814979,
0.00881802786499082));
#46116=CARTESIAN_POINT('Origin',(-0.194610820040351,0.00711537823747164,
0.00203978596199847));
#46117=CARTESIAN_POINT('Ctrl Pts',(-0.191053242553077,0.00360271141258139,
0.00908428820748653));
#46118=CARTESIAN_POINT('Ctrl Pts',(-0.191052569970049,0.00359318967230302,
0.00910573763815595));
#46119=CARTESIAN_POINT('Ctrl Pts',(-0.191043275012929,0.00357822482286264,
0.00913268910298602));
#46120=CARTESIAN_POINT('Ctrl Pts',(-0.191014962710414,0.00355712033360826,
0.00914835516048045));
#46121=CARTESIAN_POINT('Ctrl Pts',(-0.190999318265651,0.0035454586887731,
0.00915701170725896));
#46122=CARTESIAN_POINT('Ctrl Pts',(-0.190977649332568,0.00353243205832534,
0.00916064451185934));
#46123=CARTESIAN_POINT('Ctrl Pts',(-0.190954534254184,0.00352393167612197,
0.00915627380277794));
#46124=CARTESIAN_POINT('Ctrl Pts',(-0.190934183649427,0.0037372444874487,
0.00914086988152931));
#46125=CARTESIAN_POINT('Ctrl Pts',(-0.190932852889833,0.00369517829876202,
0.00923782622115866));
#46126=CARTESIAN_POINT('Ctrl Pts',(-0.190855734892733,0.00363259200256237,
0.00920313590394181));
#46127=CARTESIAN_POINT('Ctrl Pts',(-0.191122446529827,0.0035006976223372,
0.00904127409012918));
#46128=CARTESIAN_POINT('Ctrl Pts',(-0.191121414789953,0.00345576162697059,
0.00913680019546882));
#46129=CARTESIAN_POINT('Ctrl Pts',(-0.191033257028283,0.0034024260949739,
0.00910455083415403));
#46130=CARTESIAN_POINT('Ctrl Pts',(-0.191561608589598,0.00320278619904903,
0.00890344310116076));
#46131=CARTESIAN_POINT('Ctrl Pts',(-0.191561013525955,0.00315437706644305,
0.00899812271039178));
#46132=CARTESIAN_POINT('Ctrl Pts',(-0.191527722358912,0.00306053710433882,
0.00894344562862373));
#46133=CARTESIAN_POINT('Ctrl Pts',(-0.192148771194034,0.00301412826261319,
0.00881422045040244));
#46134=CARTESIAN_POINT('Ctrl Pts',(-0.192147303763206,0.00296401287835609,
0.00890776993720604));
#46135=CARTESIAN_POINT('Ctrl Pts',(-0.192106853669778,0.0028820556788135,
0.00885592463034678));
#46136=CARTESIAN_POINT('Ctrl Pts',(-0.192426303994506,0.00290954717981133,
0.00876152705466917));
#46137=CARTESIAN_POINT('Ctrl Pts',(-0.192425106237976,0.00285811942618207,
0.00885439357611185));
#46138=CARTESIAN_POINT('Ctrl Pts',(-0.192385551248651,0.00277512108865769,
0.00880072184303747));
#46139=CARTESIAN_POINT('Origin',(-0.22505940669331,0.00262788566134477,
-0.00925282722029539));
#46140=CARTESIAN_POINT('Ctrl Pts',(-0.225017273462258,0.00228350670705836,
-0.00900753387751742));
#46141=CARTESIAN_POINT('Ctrl Pts',(-0.225016618997253,0.00226753903385881,
-0.00902807321753408));
#46142=CARTESIAN_POINT('Ctrl Pts',(-0.224995064422474,0.00223443663122194,
-0.0090512478955521));
#46143=CARTESIAN_POINT('Ctrl Pts',(-0.224957173953608,0.00220011152757988,
-0.00905137780072061));
#46144=CARTESIAN_POINT('Ctrl Pts',(-0.224939696469926,0.00218427861611907,
-0.00905143772121066));
#46145=CARTESIAN_POINT('Ctrl Pts',(-0.224918567789863,0.00216920129523207,
-0.00904681991919557));
#46146=CARTESIAN_POINT('Ctrl Pts',(-0.224895681452505,0.00215874544783754,
-0.00903810107358197));
#46147=CARTESIAN_POINT('Ctrl Pts',(-0.225202513398594,0.00215390640396955,
-0.00904067530421461));
#46148=CARTESIAN_POINT('Ctrl Pts',(-0.225222962285849,0.0021853939560013,
-0.00906395019002407));
#46149=CARTESIAN_POINT('Ctrl Pts',(-0.225251193905704,0.00223630020952242,
-0.00907966627427055));
#46150=CARTESIAN_POINT('Ctrl Pts',(-0.225265203386337,0.00227752916182422,
-0.00907232786917598));
#46151=CARTESIAN_POINT('Ctrl Pts',(-0.22527246641627,0.0022989037668184,
-0.00906852337011824));
#46152=CARTESIAN_POINT('Ctrl Pts',(-0.225277058816433,0.00231715688114545,
-0.00905899968495788));
#46153=CARTESIAN_POINT('Ctrl Pts',(-0.225277037624834,0.00232818316358624,
-0.009044627616207));
#46154=CARTESIAN_POINT('Origin',(-0.226664408832371,0.00780583959346437,
-0.00183869293915824));
#46155=CARTESIAN_POINT('Ctrl Pts',(-0.225398032236364,0.00187965741570819,
-0.00870574455337625));
#46156=CARTESIAN_POINT('Ctrl Pts',(-0.225397670102207,0.00186284156270298,
-0.00872622281070892));
#46157=CARTESIAN_POINT('Ctrl Pts',(-0.225383677532918,0.00183056037380823,
-0.00874116199336752));
#46158=CARTESIAN_POINT('Ctrl Pts',(-0.225369807377174,0.00180549564236411,
-0.00874167732286142));
#46159=CARTESIAN_POINT('Ctrl Pts',(-0.225357067469305,0.00178247337965452,
-0.00874215065931098));
#46160=CARTESIAN_POINT('Ctrl Pts',(-0.225344270584155,0.00176631228172648,
-0.00873834609751508));
#46161=CARTESIAN_POINT('Ctrl Pts',(-0.225322589017758,0.00174427895566282,
-0.00872225830951696));
#46162=CARTESIAN_POINT('Ctrl Pts',(-0.225320665464812,0.0017423241951762,
-0.00872083102739873));
#46163=CARTESIAN_POINT('Ctrl Pts',(-0.225318672542542,0.00174034173716805,
-0.00871927766735267));
#46164=CARTESIAN_POINT('Ctrl Pts',(-0.225316604397166,0.0017383399119561,
-0.0087175758055758));
#46165=CARTESIAN_POINT('Origin',(-0.221413443561174,0.00402141110915759,
-0.00795211642683932));
#46166=CARTESIAN_POINT('Ctrl Pts',(-0.22512329647086,0.00302740120073959,
-0.0094920048930922));
#46167=CARTESIAN_POINT('Ctrl Pts',(-0.225122829997078,0.00301427597960748,
-0.00951459329922939));
#46168=CARTESIAN_POINT('Ctrl Pts',(-0.225112043106003,0.00299810554080808,
-0.00954228597437161));
#46169=CARTESIAN_POINT('Ctrl Pts',(-0.225080306438971,0.0029854217871898,
-0.00956043404639643));
#46170=CARTESIAN_POINT('Ctrl Pts',(-0.22506440406025,0.00297906630400566,
-0.00956952755057898));
#46171=CARTESIAN_POINT('Ctrl Pts',(-0.225043136430339,0.00297421075602464,
-0.00957511746433099));
#46172=CARTESIAN_POINT('Ctrl Pts',(-0.225021220651722,0.00297339553324741,
-0.00957419359245674));
#46173=CARTESIAN_POINT('Origin',(-0.225236920251344,0.00180210050578165,
-0.00863903021502896));
#46174=CARTESIAN_POINT('Ctrl Pts',(-0.22652065160046,0.00174023860749072,
-0.00874178828015322));
#46175=CARTESIAN_POINT('Ctrl Pts',(-0.226487204106126,0.00176069370205139,
-0.00875884229287255));
#46176=CARTESIAN_POINT('Ctrl Pts',(-0.226470246988884,0.00177636799853321,
-0.0087638065890931));
#46177=CARTESIAN_POINT('Ctrl Pts',(-0.226449412389476,0.00179560312689298,
-0.00876408887588995));
#46178=CARTESIAN_POINT('Ctrl Pts',(-0.226447161748294,0.00179768098647492,
-0.00876411936969872));
#46179=CARTESIAN_POINT('Ctrl Pts',(-0.226444880102038,0.00179983146927284,
-0.00876406231823839));
#46180=CARTESIAN_POINT('Ctrl Pts',(-0.226442559673134,0.00180208740374035,
-0.00876390573224407));
#46181=CARTESIAN_POINT('Ctrl Pts',(-0.226421164393966,0.00182288801850279,
-0.0087624619469782));
#46182=CARTESIAN_POINT('Ctrl Pts',(-0.226399628888184,0.00185516923677106,
-0.00875058152146249));
#46183=CARTESIAN_POINT('Ctrl Pts',(-0.226396806525128,0.00187493136781516,
-0.0087321638437343));
#46184=CARTESIAN_POINT('Ctrl Pts',(-0.226396489163485,0.00187715352784392,
-0.00873009286124872));
#46185=CARTESIAN_POINT('Ctrl Pts',(-0.226396357073774,0.00187919374951108,
-0.00872795259181485));
#46186=CARTESIAN_POINT('Ctrl Pts',(-0.226396396172104,0.00188100664625559,
-0.00872574966728709));
#46187=CARTESIAN_POINT('Ctrl Pts',(-0.225204446336403,0.0026266116901076,
-0.00924432147987809));
#46188=CARTESIAN_POINT('Ctrl Pts',(-0.225204186385791,0.00256699386850615,
-0.0093357214718889));
#46189=CARTESIAN_POINT('Ctrl Pts',(-0.225097536665866,0.00255469103811688,
-0.0093160140711595));
#46190=CARTESIAN_POINT('Ctrl Pts',(-0.224843954512892,0.0041869607368055,
-0.0102625319434793));
#46191=CARTESIAN_POINT('Ctrl Pts',(-0.224843308353265,0.00414600493747456,
-0.010366055089662));
#46192=CARTESIAN_POINT('Ctrl Pts',(-0.224732922386792,0.00414683281156139,
-0.010359908500413));
#46193=CARTESIAN_POINT('Ctrl Pts',(-0.224960782705356,0.00611227388836029,
-0.0107818802397));
#46194=CARTESIAN_POINT('Ctrl Pts',(-0.224959834766411,0.00609508919934752,
-0.0108921774109498));
#46195=CARTESIAN_POINT('Ctrl Pts',(-0.224851943717515,0.00610784388063427,
-0.0108832416000841));
#46196=CARTESIAN_POINT('Ctrl Pts',(-0.225134764212758,0.00797670854236963,
-0.0106811162212081));
#46197=CARTESIAN_POINT('Ctrl Pts',(-0.225133867458967,0.00798256516491125,
-0.0107900411429812));
#46198=CARTESIAN_POINT('Ctrl Pts',(-0.225025636845997,0.00799125572483553,
-0.0107791637264416));
#46199=CARTESIAN_POINT('Ctrl Pts',(-0.225092276670026,0.00750489649772228,
-0.01069488405633));
#46200=CARTESIAN_POINT('Ctrl Pts',(-0.225092128720339,0.00750490060436441,
-0.010701428529533));
#46201=CARTESIAN_POINT('Ctrl Pts',(-0.225091336119301,0.00750490447888119,
-0.010707942167662));
#46202=CARTESIAN_POINT('Ctrl Pts',(-0.225088394527797,0.00750491197011461,
-0.0107211259016258));
#46203=CARTESIAN_POINT('Ctrl Pts',(-0.225086170863583,0.00750491553257603,
-0.0107277427406404));
#46204=CARTESIAN_POINT('Ctrl Pts',(-0.225077921390693,0.00750492486451957,
-0.0107457902190495));
#46205=CARTESIAN_POINT('Ctrl Pts',(-0.225070348970769,0.00750492976174552,
-0.0107563581170778));
#46206=CARTESIAN_POINT('Ctrl Pts',(-0.225051612800588,0.00750493867065022,
-0.0107740510630533));
#46207=CARTESIAN_POINT('Ctrl Pts',(-0.225040622831016,0.00750494157171742,
-0.0107810095606538));
#46208=CARTESIAN_POINT('Ctrl Pts',(-0.225011480672544,0.00750496211207701,
-0.0107924079104823));
#46209=CARTESIAN_POINT('Ctrl Pts',(-0.224997203143753,0.00750484457550957,
-0.0107925677269123));
#46210=CARTESIAN_POINT('Ctrl Pts',(-0.22499236923333,0.00750532531593724,
-0.0107926204687227));
#46211=CARTESIAN_POINT('Ctrl Pts',(-0.224991813978919,0.00750541957447757,
-0.0107926197981443));
#46212=CARTESIAN_POINT('Ctrl Pts',(-0.224991176190761,0.00750565492711975,
-0.0107926161397585));
#46213=CARTESIAN_POINT('Ctrl Pts',(-0.224990994648027,0.00750575025996745,
-0.0107926144173287));
#46214=CARTESIAN_POINT('Ctrl Pts',(-0.224990699885213,0.00750599070999525,
-0.0107926109188229));
#46215=CARTESIAN_POINT('Origin',(-0.228248406260441,0.00774941156494066,
-0.00207700075378771));
#46216=CARTESIAN_POINT('Ctrl Pts',(-0.226399236752868,0.00218270468350247,
-0.00908497199103555));
#46217=CARTESIAN_POINT('Ctrl Pts',(-0.226365903759496,0.0022077025998989,
-0.0091023416857952));
#46218=CARTESIAN_POINT('Ctrl Pts',(-0.226347961427136,0.00222302783543612,
-0.00910602669584673));
#46219=CARTESIAN_POINT('Ctrl Pts',(-0.226329441624569,0.00224518588862393,
-0.00910807014497639));
#46220=CARTESIAN_POINT('Ctrl Pts',(-0.226327076128619,0.00224801609077578,
-0.00910833115049321));
#46221=CARTESIAN_POINT('Ctrl Pts',(-0.226324703650294,0.00225098073497979,
-0.00910850424177511));
#46222=CARTESIAN_POINT('Ctrl Pts',(-0.226322290680913,0.00225412156710692,
-0.00910855561276932));
#46223=CARTESIAN_POINT('Ctrl Pts',(-0.226303524544785,0.00227854843457011,
-0.0091089551350667));
#46224=CARTESIAN_POINT('Ctrl Pts',(-0.226281641731344,0.00231268229690328,
-0.00909758541846404));
#46225=CARTESIAN_POINT('Ctrl Pts',(-0.22627679619897,0.0023306356395595,
-0.0090785542339953));
#46226=CARTESIAN_POINT('Ctrl Pts',(-0.226276140780917,0.00233306405071963,
-0.00907598003142816));
#46227=CARTESIAN_POINT('Ctrl Pts',(-0.226275806586992,0.00233523498560651,
-0.00907334009471901));
#46228=CARTESIAN_POINT('Ctrl Pts',(-0.226275854855421,0.00233713586297991,
-0.0090706994431196));
#46229=CARTESIAN_POINT('Ctrl Pts',(-0.225133508843075,0.0070426021535604,
-0.0106822844475311));
#46230=CARTESIAN_POINT('Ctrl Pts',(-0.225132851123412,0.00703714641402199,
-0.0107876109477567));
#46231=CARTESIAN_POINT('Ctrl Pts',(-0.225027954928167,0.00702870940870006,
-0.0107808140229128));
#46232=CARTESIAN_POINT('Ctrl Pts',(-0.22505071331137,0.00795538372590099,
-0.0107280453401897));
#46233=CARTESIAN_POINT('Ctrl Pts',(-0.225050042044769,0.00796099163518786,
-0.0108339164285507));
#46234=CARTESIAN_POINT('Ctrl Pts',(-0.224945248577277,0.00794989075010101,
-0.0108283334006842));
#46235=CARTESIAN_POINT('Ctrl Pts',(-0.224891592789171,0.0098189938545337,
-0.0105337716279733));
#46236=CARTESIAN_POINT('Ctrl Pts',(-0.224890988885346,0.00984605488963252,
-0.0106374837459184));
#46237=CARTESIAN_POINT('Ctrl Pts',(-0.224785486085702,0.00984549125624428,
-0.0106327018871958));
#46238=CARTESIAN_POINT('Ctrl Pts',(-0.225018871785121,0.0115441087398936,
-0.00977372250019193));
#46239=CARTESIAN_POINT('Ctrl Pts',(-0.225018607206713,0.0115921107104299,
-0.0098682361745316));
#46240=CARTESIAN_POINT('Ctrl Pts',(-0.224913292664793,0.01159740002097,
-0.00985985852773063));
#46241=CARTESIAN_POINT('Ctrl Pts',(-0.225178663464904,0.0122963651375774,
-0.00929332951627353));
#46242=CARTESIAN_POINT('Ctrl Pts',(-0.225178596738866,0.0123530193226692,
-0.00938229566958859));
#46243=CARTESIAN_POINT('Ctrl Pts',(-0.225075076993298,0.0123667363075108,
-0.0093669049292091));
#46244=CARTESIAN_POINT('Ctrl Pts',(-0.22500367450264,0.0119594504746824,
-0.00961245894030661));
#46245=CARTESIAN_POINT('Ctrl Pts',(-0.225042476908726,0.0119588072618708,
-0.00961362081736056));
#46246=CARTESIAN_POINT('Ctrl Pts',(-0.225075686348922,0.0119457864636921,
-0.00959384445542012));
#46247=CARTESIAN_POINT('Ctrl Pts',(-0.225090894665548,0.011933491925558,
-0.00957280406153543));
#46248=CARTESIAN_POINT('Ctrl Pts',(-0.225101658275347,0.0119247905278699,
-0.00955791282831388));
#46249=CARTESIAN_POINT('Ctrl Pts',(-0.22510571623242,0.011916204305882,
-0.00954259735527654));
#46250=CARTESIAN_POINT('Ctrl Pts',(-0.225106005940227,0.0119082516245216,
-0.00952863752848153));
#46251=CARTESIAN_POINT('Origin',(-0.226795305644497,0.00512875096591446,
-0.0111302531463925));
#46252=CARTESIAN_POINT('Ctrl Pts',(-0.227126281596587,0.00216860077931266,
-0.00908887685446537));
#46253=CARTESIAN_POINT('Ctrl Pts',(-0.227103468837074,0.00219179982118522,
-0.00910550310580199));
#46254=CARTESIAN_POINT('Ctrl Pts',(-0.22709216978019,0.00220949873293601,
-0.00910753311530889));
#46255=CARTESIAN_POINT('Ctrl Pts',(-0.227080571285647,0.00222769884615225,
-0.00910656554082502));
#46256=CARTESIAN_POINT('Ctrl Pts',(-0.227078774217523,0.00223051876758185,
-0.0091064156250531));
#46257=CARTESIAN_POINT('Ctrl Pts',(-0.227076958950209,0.00223341391934925,
-0.00910611361219578));
#46258=CARTESIAN_POINT('Ctrl Pts',(-0.22707510700407,0.00223645998904377,
-0.00910561814509268));
#46259=CARTESIAN_POINT('Ctrl Pts',(-0.227061302369607,0.00225916576746203,
-0.00910192487232323));
#46260=CARTESIAN_POINT('Ctrl Pts',(-0.22705025226088,0.0022883868956522,
-0.00908773493242626));
#46261=CARTESIAN_POINT('Ctrl Pts',(-0.22705075587212,0.00230593082281523,
-0.00906364037858624));
#46262=CARTESIAN_POINT('Origin',(-0.220737639952009,0.0101645710188458,
-0.00705086064850374));
#46263=CARTESIAN_POINT('Ctrl Pts',(-0.224973343469933,0.0127081065850716,
-0.00901241391075122));
#46264=CARTESIAN_POINT('Ctrl Pts',(-0.224972867526866,0.0127230932238013,
-0.00903178146774925));
#46265=CARTESIAN_POINT('Ctrl Pts',(-0.224954069874002,0.0127463242050564,
-0.00905044998856422));
#46266=CARTESIAN_POINT('Ctrl Pts',(-0.224920022767307,0.0127792324768161,
-0.00905480033347338));
#46267=CARTESIAN_POINT('Ctrl Pts',(-0.224901830748141,0.0127968159947325,
-0.00905712480581916));
#46268=CARTESIAN_POINT('Ctrl Pts',(-0.224878894299268,0.0128172384444568,
-0.00905462517503522));
#46269=CARTESIAN_POINT('Ctrl Pts',(-0.22485135503735,0.0128342630404597,
-0.00904243198075601));
#46270=CARTESIAN_POINT('Ctrl Pts',(-0.227001241570868,0.00180642850357482,
-0.0088047000233499));
#46271=CARTESIAN_POINT('Ctrl Pts',(-0.226900506181097,0.00183019171535291,
-0.00882613840246201));
#46272=CARTESIAN_POINT('Ctrl Pts',(-0.226904412758277,0.00189655459570073,
-0.00874393346586029));
#46273=CARTESIAN_POINT('Ctrl Pts',(-0.227153448032914,0.0022110448391632,
-0.00914043886458957));
#46274=CARTESIAN_POINT('Ctrl Pts',(-0.227049842562979,0.00222790739901197,
-0.00915517224639843));
#46275=CARTESIAN_POINT('Ctrl Pts',(-0.227053893271391,0.00228956405612877,
-0.00906920714343653));
#46276=CARTESIAN_POINT('Ctrl Pts',(-0.227365349818599,0.00297531408401169,
-0.00966050279634506));
#46277=CARTESIAN_POINT('Ctrl Pts',(-0.227267539357192,0.00301108431445871,
-0.00968461017188333));
#46278=CARTESIAN_POINT('Ctrl Pts',(-0.227271547008689,0.00306306528267084,
-0.00959208981312559));
#46279=CARTESIAN_POINT('Ctrl Pts',(-0.228325656075677,0.00449820905690461,
-0.0104150080377229));
#46280=CARTESIAN_POINT('Ctrl Pts',(-0.228240062671686,0.00455763333783317,
-0.0104388268493249));
#46281=CARTESIAN_POINT('Ctrl Pts',(-0.22824408912365,0.00459088144197996,
-0.0103373670073668));
#46282=CARTESIAN_POINT('Ctrl Pts',(-0.229161619106937,0.00554785569106383,
-0.0107000249104784));
#46283=CARTESIAN_POINT('Ctrl Pts',(-0.229078979149685,0.00561257757990715,
-0.0107161200036778));
#46284=CARTESIAN_POINT('Ctrl Pts',(-0.229083451610345,0.00563384010371639,
-0.0106119667335707));
#46285=CARTESIAN_POINT('Ctrl Pts',(-0.229777994677051,0.00626685681131663,
-0.0108152446626343));
#46286=CARTESIAN_POINT('Ctrl Pts',(-0.229697325445588,0.00633494067670393,
-0.0108264360914299));
#46287=CARTESIAN_POINT('Ctrl Pts',(-0.22970183524063,0.00634769058836431,
-0.0107211605684957));
#46288=CARTESIAN_POINT('Ctrl Pts',(-0.229392048724075,0.00598507781155818,
-0.0106610739775155));
#46289=CARTESIAN_POINT('Ctrl Pts',(-0.229390542419233,0.00597321450034639,
-0.0107280577062599));
#46290=CARTESIAN_POINT('Ctrl Pts',(-0.229392105759804,0.00588226597872448,
-0.0107445713598933));
#46291=CARTESIAN_POINT('Ctrl Pts',(-0.229393975477449,0.00581660464796607,
-0.0107320544081558));
#46292=CARTESIAN_POINT('Origin',(-0.225014917424223,0.0121976159450981,
-0.00937785723393056));
#46293=CARTESIAN_POINT('Ctrl Pts',(-0.225267117543399,0.0126690414880847,
-0.00904616167166099));
#46294=CARTESIAN_POINT('Ctrl Pts',(-0.22526707803216,0.0126827612232737,
-0.00906407729233419));
#46295=CARTESIAN_POINT('Ctrl Pts',(-0.225249780251561,0.012753996211984,
-0.00910717479492578));
#46296=CARTESIAN_POINT('Ctrl Pts',(-0.225189992040237,0.012835362403236,
-0.00904829323284222));
#46297=CARTESIAN_POINT('Ctrl Pts',(-0.224396676139726,-0.00142332076525291,
0.00171535545036799));
#46298=CARTESIAN_POINT('Ctrl Pts',(-0.22440262397633,-0.00152767275903206,
0.0017228806849109));
#46299=CARTESIAN_POINT('Ctrl Pts',(-0.224301788788553,-0.00153188245866574,
0.00169183918866943));
#46300=CARTESIAN_POINT('Ctrl Pts',(-0.224886223773115,-0.00150538358571777,
0.000505008790366226));
#46301=CARTESIAN_POINT('Ctrl Pts',(-0.224888895735799,-0.00161018065377861,
0.000505692381198935));
#46302=CARTESIAN_POINT('Ctrl Pts',(-0.224791190497898,-0.00160705300214277,
0.000469981952361821));
#46303=CARTESIAN_POINT('Ctrl Pts',(-0.225312479549641,-0.00146449675102691,
-0.00113756146524579));
#46304=CARTESIAN_POINT('Ctrl Pts',(-0.225317589847797,-0.00156890719457313,
-0.00113693061187638));
#46305=CARTESIAN_POINT('Ctrl Pts',(-0.225215903592698,-0.00157050028691277,
-0.00116612020660587));
#46306=CARTESIAN_POINT('Ctrl Pts',(-0.226180826034794,-0.00134425411844392,
-0.00294330696628029));
#46307=CARTESIAN_POINT('Ctrl Pts',(-0.226184344417459,-0.00144865223190297,
-0.00295560123666401));
#46308=CARTESIAN_POINT('Ctrl Pts',(-0.226091759329284,-0.00144114023446119,
-0.00300491641135075));
#46309=CARTESIAN_POINT('Ctrl Pts',(-0.226933085082599,-0.00110947784190311,
-0.00418900462821542));
#46310=CARTESIAN_POINT('Ctrl Pts',(-0.226935809002347,-0.00121135843081841,
-0.00421601234379386));
#46311=CARTESIAN_POINT('Ctrl Pts',(-0.226849103899972,-0.00119375720027678,
-0.00427331043439446));
#46312=CARTESIAN_POINT('Ctrl Pts',(-0.227852338361138,-0.00071336136482749,
-0.0053200366555796));
#46313=CARTESIAN_POINT('Ctrl Pts',(-0.227854799933957,-0.000811012846727041,
-0.00535991228805838));
#46314=CARTESIAN_POINT('Ctrl Pts',(-0.227774403608196,-0.000782339329089386,
-0.00542196422418219));
#46315=CARTESIAN_POINT('Ctrl Pts',(-0.228870818459826,-0.000230238301254827,
-0.00627315584430081));
#46316=CARTESIAN_POINT('Ctrl Pts',(-0.228872528896894,-0.000322624060608064,
-0.0063238210346253));
#46317=CARTESIAN_POINT('Ctrl Pts',(-0.228798516093321,-0.000283020163498878,
-0.00638754543715099));
#46318=CARTESIAN_POINT('Ctrl Pts',(-0.229685021388832,0.00016983281225574,
-0.00692536606282476));
#46319=CARTESIAN_POINT('Ctrl Pts',(-0.229686436788066,8.18761831818451E-5,
-0.0069834750083683));
#46320=CARTESIAN_POINT('Ctrl Pts',(-0.229616247601761,0.000128826935045281,
-0.00704653030251611));
#46321=CARTESIAN_POINT('Ctrl Pts',(-0.230541713269828,0.000600161250818714,
-0.00751902719524027));
#46322=CARTESIAN_POINT('Ctrl Pts',(-0.230542692670766,0.000516956443363417,
-0.00758381901479241));
#46323=CARTESIAN_POINT('Ctrl Pts',(-0.230474718780796,0.000570314407031533,
-0.00764432333491235));
#46324=CARTESIAN_POINT('Ctrl Pts',(-0.231240730721998,0.00101586856032313,
-0.00800875883378466));
#46325=CARTESIAN_POINT('Ctrl Pts',(-0.231241596006655,0.000937600164170982,
-0.00807926470697491));
#46326=CARTESIAN_POINT('Ctrl Pts',(-0.231167251978618,0.000991127187817129,
-0.00813130972012129));
#46327=CARTESIAN_POINT('Ctrl Pts',(-0.231746311087107,0.00141861438610773,
-0.00842042128462309));
#46328=CARTESIAN_POINT('Ctrl Pts',(-0.231747138074993,0.00134534692439856,
-0.00849585660741608));
#46329=CARTESIAN_POINT('Ctrl Pts',(-0.231664594865682,0.00139585162906457,
-0.0085381855415369));
#46330=CARTESIAN_POINT('Ctrl Pts',(-0.232056074667116,0.00178920573458372,
-0.00876109936472852));
#46331=CARTESIAN_POINT('Ctrl Pts',(-0.232056921580141,0.00172079157747844,
-0.00884057353990152));
#46332=CARTESIAN_POINT('Ctrl Pts',(-0.231958886560654,0.00175583914593751,
-0.00886433751250737));
#46333=CARTESIAN_POINT('Ctrl Pts',(-0.232193077929066,0.0022593348110294,
-0.00913722136145496));
#46334=CARTESIAN_POINT('Ctrl Pts',(-0.232193895416839,0.00219728065587455,
-0.00922146917010263));
#46335=CARTESIAN_POINT('Ctrl Pts',(-0.232086297599378,0.00220194228853664,
-0.00921877403283003));
#46336=CARTESIAN_POINT('Ctrl Pts',(-0.232069159882949,0.00275709221639288,
-0.00947418078662092));
#46337=CARTESIAN_POINT('Ctrl Pts',(-0.232069760611005,0.00270143516070841,
-0.00956299654933791));
#46338=CARTESIAN_POINT('Ctrl Pts',(-0.231971241371772,0.00267077028039009,
-0.00953798268856777));
#46339=CARTESIAN_POINT('Ctrl Pts',(-0.231817071059768,0.00320367822680323,
-0.009733687825506));
#46340=CARTESIAN_POINT('Ctrl Pts',(-0.23181751007782,0.00315337366854661,
-0.00982578095251141));
#46341=CARTESIAN_POINT('Ctrl Pts',(-0.231726075148213,0.00311073478768687,
-0.00979708818873018));
#46342=CARTESIAN_POINT('Ctrl Pts',(-0.231406108401932,0.0037813454740335,
-0.0100253031754078));
#46343=CARTESIAN_POINT('Ctrl Pts',(-0.231406285019437,0.00373820127523732,
-0.0101212130320277));
#46344=CARTESIAN_POINT('Ctrl Pts',(-0.231322534976874,0.00368204180968578,
-0.0100900101324168));
#46345=CARTESIAN_POINT('Ctrl Pts',(-0.230820435181291,0.00445368016899616,
-0.0102948098424759));
#46346=CARTESIAN_POINT('Ctrl Pts',(-0.230820492564017,0.00441870338655471,
-0.0103941115079675));
#46347=CARTESIAN_POINT('Ctrl Pts',(-0.230741020352473,0.00435575367357216,
-0.0103663664226606));
#46348=CARTESIAN_POINT('Ctrl Pts',(-0.229705029163254,0.00565307708557098,
-0.0106446791912509));
#46349=CARTESIAN_POINT('Ctrl Pts',(-0.229704860572995,0.00563255866281126,
-0.0107483485835331));
#46350=CARTESIAN_POINT('Ctrl Pts',(-0.229628571771374,0.00556235013793471,
-0.0107286444532703));
#46351=CARTESIAN_POINT('Ctrl Pts',(-0.22880521178587,0.00660766312397794,
-0.0107567659866438));
#46352=CARTESIAN_POINT('Ctrl Pts',(-0.228805149664529,0.00659816138019425,
-0.0108617688099226));
#46353=CARTESIAN_POINT('Ctrl Pts',(-0.228727395906984,0.00652825978395869,
-0.0108504227547395));
#46354=CARTESIAN_POINT('Ctrl Pts',(-0.228204402529689,0.00728967204301217,
-0.0107607843627637));
#46355=CARTESIAN_POINT('Ctrl Pts',(-0.228204231002405,0.00728845450009763,
-0.0108659909308064));
#46356=CARTESIAN_POINT('Ctrl Pts',(-0.228126736912477,0.00721732932302992,
-0.0108591494756485));
#46357=CARTESIAN_POINT('Ctrl Pts',(-0.225010408220381,-0.001474251923458,
-8.66933507069693E-8));
#46358=CARTESIAN_POINT('Ctrl Pts',(-0.225010513130272,-0.00148096461986653,
-8.60291771540735E-8));
#46359=CARTESIAN_POINT('Ctrl Pts',(-0.2250099051443,-0.00148766394680708,
-8.63326333322152E-8));
#46360=CARTESIAN_POINT('Ctrl Pts',(-0.225007201134807,-0.00150128853343724,
-8.88873034778271E-8));
#46361=CARTESIAN_POINT('Ctrl Pts',(-0.225005016374328,-0.00150814265758981,
-9.12616443811379E-8));
#46362=CARTESIAN_POINT('Ctrl Pts',(-0.224996743541649,-0.0015267190689707,
-1.00688159401524E-7));
#46363=CARTESIAN_POINT('Ctrl Pts',(-0.224989020434532,-0.00153751939434098,
-1.09921160579431E-7));
#46364=CARTESIAN_POINT('Ctrl Pts',(-0.224969774277744,-0.00155577474558815,
-1.32360595393897E-7));
#46365=CARTESIAN_POINT('Ctrl Pts',(-0.224958379470597,-0.00156301015807106,
-1.46031598591108E-7));
#46366=CARTESIAN_POINT('Ctrl Pts',(-0.224932296005058,-0.00157349211018854,
-1.68872337400542E-7));
#46367=CARTESIAN_POINT('Ctrl Pts',(-0.224920543955411,-0.00157502458955791,
-2.06100960647531E-7));
#46368=CARTESIAN_POINT('Ctrl Pts',(-0.224912805021654,-0.00157563989864377,
-1.09230025696975E-7));
#46369=CARTESIAN_POINT('Ctrl Pts',(-0.22491012475841,-0.00157582454580539,
-1.61765696956859E-7));
#46370=CARTESIAN_POINT('Ctrl Pts',(-0.224907438932167,-0.00157589361967845,
-2.25179927914984E-7));
#46371=CARTESIAN_POINT('Ctrl Pts',(-0.22490660358187,-0.00157590691521979,
-2.26286434986113E-7));
#46372=CARTESIAN_POINT('Origin',(-0.226660317458695,0.00720499143128829,
-0.00184762445713072));
#46373=CARTESIAN_POINT('Ctrl Pts',(-0.225309820211856,0.0132780515765434,
-0.00870378491731464));
#46374=CARTESIAN_POINT('Ctrl Pts',(-0.225310270518267,0.0132776177035617,
-0.00870415552087384));
#46375=CARTESIAN_POINT('Ctrl Pts',(-0.225311023382707,0.0132779301043826,
-0.00870389963108353));
#46376=CARTESIAN_POINT('Ctrl Pts',(-0.225311232192588,0.0132772106330284,
-0.00870449657790214));
#46377=CARTESIAN_POINT('Ctrl Pts',(-0.225311553950656,0.0132767496254951,
-0.00870488159341767));
#46378=CARTESIAN_POINT('Ctrl Pts',(-0.225312613380327,0.0132755573730371,
-0.0087058439119948));
#46379=CARTESIAN_POINT('Ctrl Pts',(-0.225313051364385,0.013275092055929,
-0.00870621364083127));
#46380=CARTESIAN_POINT('Ctrl Pts',(-0.225314209362679,0.0132738730043072,
-0.00870716690654188));
#46381=CARTESIAN_POINT('Ctrl Pts',(-0.225315037951984,0.0132730168765924,
-0.00870781670795182));
#46382=CARTESIAN_POINT('Ctrl Pts',(-0.225317483670858,0.0132704706091192,
-0.00870968427436419));
#46383=CARTESIAN_POINT('Ctrl Pts',(-0.225319113893644,0.0132687539642296,
-0.00871086506368553));
#46384=CARTESIAN_POINT('Ctrl Pts',(-0.225323972395015,0.0132635216454238,
-0.00871422988017993));
#46385=CARTESIAN_POINT('Ctrl Pts',(-0.225327194760367,0.0132599069287703,
-0.00871625565991771));
#46386=CARTESIAN_POINT('Ctrl Pts',(-0.225342320259782,0.0132421739271964,
-0.00872479923956172));
#46387=CARTESIAN_POINT('Ctrl Pts',(-0.225353424218474,0.0132268946822168,
-0.00872819403241251));
#46388=CARTESIAN_POINT('Ctrl Pts',(-0.225370281092151,0.0131993265799017,
-0.00872784051699747));
#46389=CARTESIAN_POINT('Ctrl Pts',(-0.22537689223205,0.0131867227470534,
-0.00872543917842188));
#46390=CARTESIAN_POINT('Ctrl Pts',(-0.225385934802891,0.0131647319127703,
-0.00871617296164978));
#46391=CARTESIAN_POINT('Ctrl Pts',(-0.225388851873419,0.013155420922425,
-0.00871039322749511));
#46392=CARTESIAN_POINT('Ctrl Pts',(-0.225390991697131,0.0131433715023081,
-0.0086996018357167));
#46393=CARTESIAN_POINT('Ctrl Pts',(-0.225391353704068,0.0131399272886964,
-0.00869601173353095));
#46394=CARTESIAN_POINT('Ctrl Pts',(-0.225391419217255,0.0131367695105258,
-0.0086921820518181));
#46395=CARTESIAN_POINT('Ctrl Pts',(-0.228163515612994,0.00733515508811961,
0.0107625774342653));
#46396=CARTESIAN_POINT('Ctrl Pts',(-0.228163459199396,0.00733469307617318,
0.0108687650146076));
#46397=CARTESIAN_POINT('Ctrl Pts',(-0.228085015691996,0.0072631586172991,
0.0108613593351734));
#46398=CARTESIAN_POINT('Ctrl Pts',(-0.228743649451567,0.00665278436300879,
0.0107581182094424));
#46399=CARTESIAN_POINT('Ctrl Pts',(-0.228743828274746,0.00664383782840776,
0.0108640874686174));
#46400=CARTESIAN_POINT('Ctrl Pts',(-0.228664959938252,0.00657387845985657,
0.0108524569587656));
#46401=CARTESIAN_POINT('Ctrl Pts',(-0.22963210211456,0.00571569401386139,
0.0106555484427694));
#46402=CARTESIAN_POINT('Ctrl Pts',(-0.229632061465273,0.00569595006967033,
0.0107603333381804));
#46403=CARTESIAN_POINT('Ctrl Pts',(-0.22955520323395,0.00562499939819525,
0.0107401577457921));
#46404=CARTESIAN_POINT('Ctrl Pts',(-0.230724245638906,0.00451099638068745,
0.0103135525699589));
#46405=CARTESIAN_POINT('Ctrl Pts',(-0.230724478352774,0.00447655937784655,
0.010414023536827));
#46406=CARTESIAN_POINT('Ctrl Pts',(-0.230643166808046,0.00441441049208174,
0.0103862385728284));
#46407=CARTESIAN_POINT('Ctrl Pts',(-0.231293450457664,0.0038259590991092,
0.0100434420479585));
#46408=CARTESIAN_POINT('Ctrl Pts',(-0.231293848628935,0.00378306605575638,
0.0101404566930396));
#46409=CARTESIAN_POINT('Ctrl Pts',(-0.23120738031312,0.00372893782348863,
0.0101097087117905));
#46410=CARTESIAN_POINT('Ctrl Pts',(-0.231667282960074,0.00323956433154689,
0.00975046297908365));
#46411=CARTESIAN_POINT('Ctrl Pts',(-0.231667951722417,0.00318932082472952,
0.00984359953359723));
#46412=CARTESIAN_POINT('Ctrl Pts',(-0.23157290806973,0.00315106112455292,
0.0098166551560102));
#46413=CARTESIAN_POINT('Ctrl Pts',(-0.231878171710574,0.00277621374154605,
0.00948262239106185));
#46414=CARTESIAN_POINT('Ctrl Pts',(-0.231879062889777,0.00272020523476094,
0.00957221388849241));
#46415=CARTESIAN_POINT('Ctrl Pts',(-0.231775237663013,0.00269967656492334,
0.0095526871407656));
#46416=CARTESIAN_POINT('Ctrl Pts',(-0.231911081200316,0.0022771945351161,
0.00914372039368585));
#46417=CARTESIAN_POINT('Ctrl Pts',(-0.231912143168076,0.00221451729150512,
0.00922872354247918));
#46418=CARTESIAN_POINT('Ctrl Pts',(-0.23180532211203,0.00223182547592494,
0.0092344894905382));
#46419=CARTESIAN_POINT('Ctrl Pts',(-0.231724190086194,0.00183722198742645,
0.00879379616530824));
#46420=CARTESIAN_POINT('Ctrl Pts',(-0.231725223949959,0.00176861677599736,
0.0088744276874275));
#46421=CARTESIAN_POINT('Ctrl Pts',(-0.231629985856898,0.00180875294582294,
0.00890135004891185));
#46422=CARTESIAN_POINT('Ctrl Pts',(-0.231408286783581,0.00147669052636452,
0.00846836905126042));
#46423=CARTESIAN_POINT('Ctrl Pts',(-0.231409336524876,0.00140344626307841,
0.00854510935254151));
#46424=CARTESIAN_POINT('Ctrl Pts',(-0.231325538660294,0.00145450447662584,
0.00858614430807182));
#46425=CARTESIAN_POINT('Ctrl Pts',(-0.230925990974879,0.0010718808526038,
0.00806298588782171));
#46426=CARTESIAN_POINT('Ctrl Pts',(-0.230927069716664,0.000993566663471985,
0.00813479332567291));
#46427=CARTESIAN_POINT('Ctrl Pts',(-0.230849955200748,0.00104704858832882,
0.0081846698003006));
#46428=CARTESIAN_POINT('Ctrl Pts',(-0.230261991331419,0.000642679936980595,
0.00756775583408155));
#46429=CARTESIAN_POINT('Ctrl Pts',(-0.230263231713554,0.000559265972955093,
0.0076337316989568));
#46430=CARTESIAN_POINT('Ctrl Pts',(-0.230191098868531,0.000612031842833926,
0.00769135709643061));
#46431=CARTESIAN_POINT('Ctrl Pts',(-0.22919233226498,4.57818412561549E-5,
0.0067574639823101));
#46432=CARTESIAN_POINT('Ctrl Pts',(-0.229194129960548,-4.4281278233945E-5,
0.00681420798335808));
#46433=CARTESIAN_POINT('Ctrl Pts',(-0.229119133350779,1.08743265013897E-8,
0.00687532298388693));
#46434=CARTESIAN_POINT('Ctrl Pts',(-0.227932685841537,-0.000625271979417362,
0.00557903136162669));
#46435=CARTESIAN_POINT('Ctrl Pts',(-0.227935460994856,-0.000722688106822415,
0.00562244279410726));
#46436=CARTESIAN_POINT('Ctrl Pts',(-0.227852889082099,-0.000692019389878893,
0.00568252489260457));
#46437=CARTESIAN_POINT('Ctrl Pts',(-0.226870498362358,-0.00111144671474683,
0.00418396327020359));
#46438=CARTESIAN_POINT('Ctrl Pts',(-0.226873447749571,-0.00121426192939155,
0.00421110560023027));
#46439=CARTESIAN_POINT('Ctrl Pts',(-0.226784623034336,-0.00119640615038005,
0.00426665238329828));
#46440=CARTESIAN_POINT('Ctrl Pts',(-0.226141786432928,-0.00134786885158213,
0.00291774568293432));
#46441=CARTESIAN_POINT('Ctrl Pts',(-0.226145556131887,-0.00145321997732708,
0.0029296788274651));
#46442=CARTESIAN_POINT('Ctrl Pts',(-0.226051217691109,-0.00144536866999242,
0.00297752009225177));
#46443=CARTESIAN_POINT('Ctrl Pts',(-0.225309314238018,-0.00146331986333167,
0.00111118276018021));
#46444=CARTESIAN_POINT('Ctrl Pts',(-0.225314574440745,-0.00156865189798677,
0.00111063356664893));
#46445=CARTESIAN_POINT('Ctrl Pts',(-0.225212189039601,-0.00156924905290015,
0.00113991809877219));
#46446=CARTESIAN_POINT('Ctrl Pts',(-0.224886529385567,-0.0015053586236984,
-0.00049391139130483));
#46447=CARTESIAN_POINT('Ctrl Pts',(-0.224889615321908,-0.00161108241616776,
-0.00049465971725397));
#46448=CARTESIAN_POINT('Ctrl Pts',(-0.224790799753559,-0.00160751596957962,
-0.000458880758028573));
#46449=CARTESIAN_POINT('Ctrl Pts',(-0.224413778106133,-0.0014231156766575,
-0.00169196883250104));
#46450=CARTESIAN_POINT('Ctrl Pts',(-0.224419774485945,-0.00152837716757349,
-0.0016996429168911));
#46451=CARTESIAN_POINT('Ctrl Pts',(-0.224318111707952,-0.00153157542826408,
-0.00166863240918668));
#46452=CARTESIAN_POINT('Ctrl Pts',(-0.229322728421253,0.00603936961279809,
0.0106687798113575));
#46453=CARTESIAN_POINT('Ctrl Pts',(-0.229321217780042,0.0060278782329308,
0.0107359585066643));
#46454=CARTESIAN_POINT('Ctrl Pts',(-0.229322620684285,0.00593681079674449,
0.0107528602121019));
#46455=CARTESIAN_POINT('Ctrl Pts',(-0.229324382301549,0.00587096534799219,
0.0107407249786847));
#46456=CARTESIAN_POINT('Origin',(-0.226555118506608,0.0132132840185884,
-0.00865094685306489));
#46457=CARTESIAN_POINT('Ctrl Pts',(-0.226391100214881,0.0131362729098227,
-0.00871148492904484));
#46458=CARTESIAN_POINT('Ctrl Pts',(-0.22639099939902,0.0131408916001344,
-0.00871707599316609));
#46459=CARTESIAN_POINT('Ctrl Pts',(-0.226391877522066,0.0131460464250971,
-0.00872209676525605));
#46460=CARTESIAN_POINT('Ctrl Pts',(-0.226396241089665,0.0131597801495802,
-0.00873297084794114));
#46461=CARTESIAN_POINT('Ctrl Pts',(-0.226400631403011,0.0131684509980104,
-0.00873781356047663));
#46462=CARTESIAN_POINT('Ctrl Pts',(-0.22641373138063,0.0131891685691253,
-0.00874613941805954));
#46463=CARTESIAN_POINT('Ctrl Pts',(-0.226424048697701,0.0132020838590036,
-0.00874865540428968));
#46464=CARTESIAN_POINT('Ctrl Pts',(-0.226454171535271,0.0132336318450819,
-0.00874868449941933));
#46465=CARTESIAN_POINT('Ctrl Pts',(-0.226475314459197,0.0132515451103633,
-0.00874360856911665));
#46466=CARTESIAN_POINT('Ctrl Pts',(-0.226504389347222,0.0132715457543843,
-0.00873146777518632));
#46467=CARTESIAN_POINT('Ctrl Pts',(-0.226509609320238,0.013274891856478,
-0.00872888455161681));
#46468=CARTESIAN_POINT('Ctrl Pts',(-0.226512544837996,0.0132762772382622,
-0.00872782692749136));
#46469=CARTESIAN_POINT('Ctrl Pts',(-0.226512607671518,0.0132767688794727,
-0.00872741805619649));
#46470=CARTESIAN_POINT('Ctrl Pts',(-0.226513565707048,0.0132773985794685,
-0.0087269091281644));
#46471=CARTESIAN_POINT('Ctrl Pts',(-0.22691449864251,0.00188912409957078,
0.00874101187538417));
#46472=CARTESIAN_POINT('Ctrl Pts',(-0.226912882541645,0.00182380187236744,
0.00882075610471368));
#46473=CARTESIAN_POINT('Ctrl Pts',(-0.227011968494547,0.00180258160872482,
0.00880179656685173));
#46474=CARTESIAN_POINT('Ctrl Pts',(-0.227052876055634,0.00228681646168442,
0.00907019845969648));
#46475=CARTESIAN_POINT('Ctrl Pts',(-0.227051157818039,0.00222625156923484,
0.00915378807385768));
#46476=CARTESIAN_POINT('Ctrl Pts',(-0.227152592109862,0.00221147656246655,
0.00914106091400232));
#46477=CARTESIAN_POINT('Ctrl Pts',(-0.227243827191478,0.00306830791249711,
0.00959853048103973));
#46478=CARTESIAN_POINT('Ctrl Pts',(-0.227242027555894,0.00301688618314614,
0.0096883671492618));
#46479=CARTESIAN_POINT('Ctrl Pts',(-0.227338827573701,0.00298480159953571,
0.0096668734289546));
#46480=CARTESIAN_POINT('Ctrl Pts',(-0.228154605500681,0.00459990079405723,
0.0103395772456444));
#46481=CARTESIAN_POINT('Ctrl Pts',(-0.228152531261446,0.00456632614965043,
0.0104381318959621));
#46482=CARTESIAN_POINT('Ctrl Pts',(-0.228237400064536,0.00450986270607348,
0.0104157331075302));
#46483=CARTESIAN_POINT('Ctrl Pts',(-0.228964082156122,0.00562823913086061,
0.0106085667885485));
#46484=CARTESIAN_POINT('Ctrl Pts',(-0.228961542575069,0.00560606514916299,
0.0107098744596661));
#46485=CARTESIAN_POINT('Ctrl Pts',(-0.229042444109394,0.00554326214965241,
0.0106944729792509));
#46486=CARTESIAN_POINT('Ctrl Pts',(-0.229559203666659,0.00631640552755159,
0.0107158903392713));
#46487=CARTESIAN_POINT('Ctrl Pts',(-0.229556533468569,0.00630212175177429,
0.0108183699092633));
#46488=CARTESIAN_POINT('Ctrl Pts',(-0.229635305092869,0.00623583857093286,
0.0108075661196736));
#46489=CARTESIAN_POINT('Ctrl Pts',(-0.227048969078908,0.00230603179210533,
0.00906366400351058));
#46490=CARTESIAN_POINT('Ctrl Pts',(-0.227048487225699,0.00228917960945197,
0.00908680953759018));
#46491=CARTESIAN_POINT('Ctrl Pts',(-0.22705976561457,0.00225915926815955,
0.00910191473859165));
#46492=CARTESIAN_POINT('Ctrl Pts',(-0.227074094125804,0.00223632626390423,
0.00910567066208655));
#46493=CARTESIAN_POINT('Ctrl Pts',(-0.227086502500316,0.00221655306741396,
0.00910892326136944));
#46494=CARTESIAN_POINT('Ctrl Pts',(-0.227096119022736,0.00220123369184519,
0.00910711704019592));
#46495=CARTESIAN_POINT('Ctrl Pts',(-0.227116358685445,0.00217914689185743,
0.00909540149177823));
#46496=CARTESIAN_POINT('Ctrl Pts',(-0.227119490693188,0.00217572904692728,
0.00909358855700337));
#46497=CARTESIAN_POINT('Ctrl Pts',(-0.227122863556042,0.00217221506441309,
0.00909145502818572));
#46498=CARTESIAN_POINT('Ctrl Pts',(-0.227126457702988,0.00216864736443003,
0.00908889965119285));
#46499=CARTESIAN_POINT('Origin',(-0.2278013545925,0.0072019569842425,-0.00186521002294653));
#46500=CARTESIAN_POINT('Ctrl Pts',(-0.22626372473152,0.0126609453232516,
-0.00907137440433446));
#46501=CARTESIAN_POINT('Ctrl Pts',(-0.226263573629508,0.0126654614507829,
-0.00907770987697118));
#46502=CARTESIAN_POINT('Ctrl Pts',(-0.226264580331983,0.0126707561268844,
-0.00908325776756278));
#46503=CARTESIAN_POINT('Ctrl Pts',(-0.226269247059774,0.0126845083276505,
-0.00909440199537926));
#46504=CARTESIAN_POINT('Ctrl Pts',(-0.226273586565231,0.0126930823229516,
-0.00909907503057873));
#46505=CARTESIAN_POINT('Ctrl Pts',(-0.226286568425147,0.0127144805599102,
-0.00910735204035213));
#46506=CARTESIAN_POINT('Ctrl Pts',(-0.226297082359114,0.0127286147065889,
-0.0091097655807238));
#46507=CARTESIAN_POINT('Ctrl Pts',(-0.226334765361614,0.0127720987460258,
-0.00910910869015226));
#46508=CARTESIAN_POINT('Ctrl Pts',(-0.226362067829375,0.012795480515493,
-0.00909854469517186));
#46509=CARTESIAN_POINT('Ctrl Pts',(-0.226381826363649,0.0128112801451954,
-0.00908888771940711));
#46510=CARTESIAN_POINT('Ctrl Pts',(-0.22638412128973,0.0128130883201525,
-0.00908769467773142));
#46511=CARTESIAN_POINT('Ctrl Pts',(-0.226385866678303,0.0128146615116663,
-0.00908662433726843));
#46512=CARTESIAN_POINT('Ctrl Pts',(-0.226386262576521,0.0128150458650998,
-0.00908635898063884));
#46513=CARTESIAN_POINT('Ctrl Pts',(-0.226386768472206,0.0128156694119735,
-0.00908592114511766));
#46514=CARTESIAN_POINT('Ctrl Pts',(-0.22638699037668,0.0128161318494855,
-0.00908558925922971));
#46515=CARTESIAN_POINT('Origin',(-0.226785760559816,0.00535801911423735,
0.0112988545290219));
#46516=CARTESIAN_POINT('Ctrl Pts',(-0.226387677522943,0.00218135007292164,
0.00908374645919642));
#46517=CARTESIAN_POINT('Ctrl Pts',(-0.226387517829732,0.00218169450496916,
0.00908399406881082));
#46518=CARTESIAN_POINT('Ctrl Pts',(-0.226387348413078,0.00218193204633596,
0.00908416247407508));
#46519=CARTESIAN_POINT('Ctrl Pts',(-0.226386693227517,0.00218265984835474,
0.00908467088690384));
#46520=CARTESIAN_POINT('Ctrl Pts',(-0.2263860557642,0.00218323697421753,
0.00908506930642161));
#46521=CARTESIAN_POINT('Ctrl Pts',(-0.226381957964186,0.00218662050727849,
0.00908732217272258));
#46522=CARTESIAN_POINT('Ctrl Pts',(-0.226374795136826,0.00219209340473146,
0.00909086571165971));
#46523=CARTESIAN_POINT('Ctrl Pts',(-0.226342638124601,0.00221913347866911,
0.00910384797271027));
#46524=CARTESIAN_POINT('Ctrl Pts',(-0.226321383091947,0.00224036162316775,
0.00910819378426068));
#46525=CARTESIAN_POINT('Ctrl Pts',(-0.226293023697157,0.00227450048798041,
0.00910644145231066));
#46526=CARTESIAN_POINT('Ctrl Pts',(-0.226283795653164,0.00228749349753115,
0.00910340025700874));
#46527=CARTESIAN_POINT('Ctrl Pts',(-0.226272433519139,0.00230732054682446,
0.00909450550810068));
#46528=CARTESIAN_POINT('Ctrl Pts',(-0.226268703397229,0.00231530414933038,
0.00908960317565377));
#46529=CARTESIAN_POINT('Ctrl Pts',(-0.226265146545548,0.00232737965992297,
0.00907890647267523));
#46530=CARTESIAN_POINT('Ctrl Pts',(-0.226264467950038,0.00233171333312063,
0.00907412667988085));
#46531=CARTESIAN_POINT('Ctrl Pts',(-0.226264593786723,0.00233548626079879,
0.00906884045917144));
#46532=CARTESIAN_POINT('Origin',(-0.226777858818941,0.00989529916463247,
-0.0111105690553547));
#46533=CARTESIAN_POINT('Ctrl Pts',(-0.227006489040078,0.0126931492004507,
-0.00906333669283264));
#46534=CARTESIAN_POINT('Ctrl Pts',(-0.227006359658267,0.0126975068624466,
-0.00906933365124984));
#46535=CARTESIAN_POINT('Ctrl Pts',(-0.227006857270868,0.0127024672528347,
-0.00907482462423548));
#46536=CARTESIAN_POINT('Ctrl Pts',(-0.227009147112344,0.0127138818625653,
-0.00908508685135224));
#46537=CARTESIAN_POINT('Ctrl Pts',(-0.227011034309181,0.0127203292004405,
-0.00908965220311262));
#46538=CARTESIAN_POINT('Ctrl Pts',(-0.227017721423457,0.0127385730039939,
-0.00909978676830201));
#46539=CARTESIAN_POINT('Ctrl Pts',(-0.22702353660833,0.0127506850584017,
-0.0091036725767193));
#46540=CARTESIAN_POINT('Ctrl Pts',(-0.227037909708246,0.0127758982765603,
-0.00910714103478806));
#46541=CARTESIAN_POINT('Ctrl Pts',(-0.227046637460994,0.0127888529052407,
-0.00910619248230766));
#46542=CARTESIAN_POINT('Ctrl Pts',(-0.227064691972426,0.0128122260649919,
-0.00909983643384995));
#46543=CARTESIAN_POINT('Ctrl Pts',(-0.227072059174435,0.0128202275894214,
-0.00909532632992795));
#46544=CARTESIAN_POINT('Ctrl Pts',(-0.22707636600345,0.0128249181393595,
-0.00909243574350203));
#46545=CARTESIAN_POINT('Ctrl Pts',(-0.227078486743332,0.0128270744437461,
-0.00909109745054717));
#46546=CARTESIAN_POINT('Ctrl Pts',(-0.227080622192005,0.0128291400139368,
-0.0090896437656076));
#46547=CARTESIAN_POINT('Ctrl Pts',(-0.227081057780342,0.0128295770214247,
-0.00908933084235787));
#46548=CARTESIAN_POINT('Origin',(-0.227796834054845,0.00779833113437804,
0.001863412373519));
#46549=CARTESIAN_POINT('Ctrl Pts',(-0.226391079628494,0.00186369918642903,
0.00871144032132472));
#46550=CARTESIAN_POINT('Ctrl Pts',(-0.226390978660276,0.00185907532151077,
0.00871703755041187));
#46551=CARTESIAN_POINT('Ctrl Pts',(-0.226391858808544,0.00185391430762597,
0.00872206300839274));
#46552=CARTESIAN_POINT('Ctrl Pts',(-0.226396229435358,0.00184017066974772,
0.00873293975251571));
#46553=CARTESIAN_POINT('Ctrl Pts',(-0.226400623541884,0.00183149690541248,
0.00873778102458434));
#46554=CARTESIAN_POINT('Ctrl Pts',(-0.22641373311484,0.00181077232703316,
0.00874610285334654));
#46555=CARTESIAN_POINT('Ctrl Pts',(-0.226424057461933,0.0017978525598305,
0.00874861517548048));
#46556=CARTESIAN_POINT('Ctrl Pts',(-0.226454202151599,0.00176629171031552,
0.00874863186234132));
#46557=CARTESIAN_POINT('Ctrl Pts',(-0.226475356568348,0.00174837615164434,
0.00874354332882413));
#46558=CARTESIAN_POINT('Ctrl Pts',(-0.226504398614371,0.00172840715421356,
0.00873140694530539));
#46559=CARTESIAN_POINT('Ctrl Pts',(-0.226509593825756,0.00172507720736087,
0.00872883644315529));
#46560=CARTESIAN_POINT('Ctrl Pts',(-0.226512524128562,0.0017236946270086,
0.00872778095183921));
#46561=CARTESIAN_POINT('Ctrl Pts',(-0.226512586716719,0.00172320269411854,
0.00872737181745011));
#46562=CARTESIAN_POINT('Ctrl Pts',(-0.226513544924145,0.00172257286242674,
0.00872686276718726));
#46563=CARTESIAN_POINT('Ctrl Pts',(-0.226844203584844,0.0131107712181138,
-0.00873939524392954));
#46564=CARTESIAN_POINT('Ctrl Pts',(-0.226842621902213,0.0131746060428305,
-0.00881739135542764));
#46565=CARTESIAN_POINT('Ctrl Pts',(-0.226938629422854,0.0131992305333852,
-0.00879836193580715));
#46566=CARTESIAN_POINT('Ctrl Pts',(-0.227013983078059,0.0127097047938499,
-0.00907297714742843));
#46567=CARTESIAN_POINT('Ctrl Pts',(-0.227012239789711,0.0127690078022699,
-0.00915470391965529));
#46568=CARTESIAN_POINT('Ctrl Pts',(-0.227109707645705,0.0127899788532772,
-0.00914054786865483));
#46569=CARTESIAN_POINT('Ctrl Pts',(-0.227247196171394,0.0119136086184864,
-0.00960839126399033));
#46570=CARTESIAN_POINT('Ctrl Pts',(-0.22724548833278,0.0119636176376727,
-0.00969634779479045));
#46571=CARTESIAN_POINT('Ctrl Pts',(-0.227340402437741,0.0119956557482216,
-0.00967769841531056));
#46572=CARTESIAN_POINT('Ctrl Pts',(-0.227934521197248,0.0108226289252953,
-0.0101349612257964));
#46573=CARTESIAN_POINT('Ctrl Pts',(-0.227932339489337,0.0108606492245814,
-0.0102288267212789));
#46574=CARTESIAN_POINT('Ctrl Pts',(-0.228016200220304,0.0109137714728394,
-0.0102076384847793));
#46575=CARTESIAN_POINT('Ctrl Pts',(-0.22871448845887,0.00979872364412934,
-0.0104964529615865));
#46576=CARTESIAN_POINT('Ctrl Pts',(-0.22871201473603,0.00982522763215701,
-0.0105942771404052));
#46577=CARTESIAN_POINT('Ctrl Pts',(-0.228792016848652,0.00988517379494635,
-0.0105788098693705));
#46578=CARTESIAN_POINT('Ctrl Pts',(-0.229293042529654,0.00909568586137089,
-0.0106532464722863));
#46579=CARTESIAN_POINT('Ctrl Pts',(-0.229290470784652,0.00911432520868509,
-0.010752734650283));
#46580=CARTESIAN_POINT('Ctrl Pts',(-0.229369210267429,0.00917698075244273,
-0.0107418335978009));
#46581=CARTESIAN_POINT('Ctrl Pts',(-0.229615819717098,0.00869617259597773,
-0.0107153935627931));
#46582=CARTESIAN_POINT('Ctrl Pts',(-0.229613213780719,0.00871029853769483,
-0.0108155121778463));
#46583=CARTESIAN_POINT('Ctrl Pts',(-0.229692353173153,0.00877277078058718,
-0.0108076154274616));
#46584=CARTESIAN_POINT('Ctrl Pts',(-0.229386006289235,0.00897973788217584,
-0.0106669693656825));
#46585=CARTESIAN_POINT('Ctrl Pts',(-0.229385834316954,0.00898106101767042,
-0.0106746123133356));
#46586=CARTESIAN_POINT('Ctrl Pts',(-0.229385712152104,0.00898372565412568,
-0.0106818666110971));
#46587=CARTESIAN_POINT('Ctrl Pts',(-0.229385551882414,0.00899195445542397,
-0.0106963846629467));
#46588=CARTESIAN_POINT('Ctrl Pts',(-0.229385531656438,0.00899774869796057,
-0.0107032419010174));
#46589=CARTESIAN_POINT('Ctrl Pts',(-0.229385610858662,0.00901508036564382,
-0.0107186785449647));
#46590=CARTESIAN_POINT('Ctrl Pts',(-0.229385792041169,0.00902866472857107,
-0.0107264500956539));
#46591=CARTESIAN_POINT('Ctrl Pts',(-0.229386386722512,0.00905943807325047,
-0.0107374076859636));
#46592=CARTESIAN_POINT('Ctrl Pts',(-0.229386768105326,0.00907540386138489,
-0.0107404657857017));
#46593=CARTESIAN_POINT('Ctrl Pts',(-0.229387633511884,0.00910728634568047,
-0.0107428879162213));
#46594=CARTESIAN_POINT('Ctrl Pts',(-0.229388121567382,0.00912354354792321,
-0.0107422591777074));
#46595=CARTESIAN_POINT('Ctrl Pts',(-0.229388775079068,0.00914282080369923,
-0.0107395367729916));
#46596=CARTESIAN_POINT('Ctrl Pts',(-0.229388881801912,0.00914623216986349,
-0.0107389781526564));
#46597=CARTESIAN_POINT('Ctrl Pts',(-0.229388998216237,0.00914960349487052,
-0.0107383496584743));
#46598=CARTESIAN_POINT('Origin',(-0.226555098762114,0.00178668839685616,
0.00865090131818249));
#46599=CARTESIAN_POINT('Ctrl Pts',(-0.225309797184906,0.00172192161890831,
0.00870374066956656));
#46600=CARTESIAN_POINT('Ctrl Pts',(-0.225310247209972,0.00172235519632964,
0.00870411103008553));
#46601=CARTESIAN_POINT('Ctrl Pts',(-0.225311002611275,0.00172203997768199,
0.00870385280409576));
#46602=CARTESIAN_POINT('Ctrl Pts',(-0.225311208914087,0.0017227600167316,
0.00870445023600111));
#46603=CARTESIAN_POINT('Ctrl Pts',(-0.225311530294346,0.00172322144104357,
0.00870483562786732));
#46604=CARTESIAN_POINT('Ctrl Pts',(-0.225312590214738,0.00172441475890014,
0.00870579884762694));
#46605=CARTESIAN_POINT('Ctrl Pts',(-0.225313028186745,0.0017248801472261,
0.00870616864922502));
#46606=CARTESIAN_POINT('Ctrl Pts',(-0.225314185750255,0.00172609889403774,
0.00870712172336859));
#46607=CARTESIAN_POINT('Ctrl Pts',(-0.225315014254334,0.00172695494933646,
0.00870777150728844));
#46608=CARTESIAN_POINT('Ctrl Pts',(-0.225317459383959,0.00172950059423514,
0.00870963873423945));
#46609=CARTESIAN_POINT('Ctrl Pts',(-0.225319089298796,0.00173121682918185,
0.00871081933948459));
#46610=CARTESIAN_POINT('Ctrl Pts',(-0.225323946891331,0.00173644787754945,
0.00871418366037928));
#46611=CARTESIAN_POINT('Ctrl Pts',(-0.22532716864885,0.00174006163539265,
0.00871620917519089));
#46612=CARTESIAN_POINT('Ctrl Pts',(-0.225342294487028,0.00175779352469263,
0.00872475379468167));
#46613=CARTESIAN_POINT('Ctrl Pts',(-0.225353399479346,0.00177307296761273,
0.00872814969225069));
#46614=CARTESIAN_POINT('Ctrl Pts',(-0.225370257987112,0.00180064171972645,
0.00872779781635509));
#46615=CARTESIAN_POINT('Ctrl Pts',(-0.225376869823117,0.00181324593478133,
0.00872539716034856));
#46616=CARTESIAN_POINT('Ctrl Pts',(-0.225385913454783,0.00183523752526527,
0.00871613199201331));
#46617=CARTESIAN_POINT('Ctrl Pts',(-0.225388830957791,0.00184454886515225,
0.00871035273326283));
#46618=CARTESIAN_POINT('Ctrl Pts',(-0.225390971525641,0.00185659996340586,
0.00869956095985846));
#46619=CARTESIAN_POINT('Ctrl Pts',(-0.225391333711933,0.0018600452739431,
0.00869596993208362));
#46620=CARTESIAN_POINT('Ctrl Pts',(-0.225391399224265,0.00186320399461255,
0.00869213917474686));
#46621=CARTESIAN_POINT('Ctrl Pts',(-0.224314879611255,0.0165309527154701,
0.00169539118491105));
#46622=CARTESIAN_POINT('Ctrl Pts',(-0.224412832453008,0.0165261318210616,
0.0017283511372909));
#46623=CARTESIAN_POINT('Ctrl Pts',(-0.22440807336887,0.0164236964218974,
0.00172137583111113));
#46624=CARTESIAN_POINT('Ctrl Pts',(-0.224796453732221,0.0166076184506538,
0.000471064888113262));
#46625=CARTESIAN_POINT('Ctrl Pts',(-0.224893455689256,0.016609717003541,
0.000502793734545124));
#46626=CARTESIAN_POINT('Ctrl Pts',(-0.224891878603847,0.0165069023284093,
0.000502434681482319));
#46627=CARTESIAN_POINT('Ctrl Pts',(-0.225201428568935,0.0165700272266111,
-0.00117029070511372));
#46628=CARTESIAN_POINT('Ctrl Pts',(-0.225300625050002,0.0165676556420741,
-0.00114004230938044));
#46629=CARTESIAN_POINT('Ctrl Pts',(-0.225296650208344,0.0164651958368812,
-0.00114023248766775));
#46630=CARTESIAN_POINT('Ctrl Pts',(-0.226095507126995,0.0164417448751073,
-0.00299946840558335));
#46631=CARTESIAN_POINT('Ctrl Pts',(-0.226186142905089,0.0164482910388427,
-0.00295072881265121));
#46632=CARTESIAN_POINT('Ctrl Pts',(-0.226183670844414,0.0163459084325657,
-0.00293822423704356));
#46633=CARTESIAN_POINT('Ctrl Pts',(-0.226658272402392,0.016256772552681,
-0.00395106792067057));
#46634=CARTESIAN_POINT('Ctrl Pts',(-0.226745240907684,0.0162705352409148,
-0.00389734512079282));
#46635=CARTESIAN_POINT('Ctrl Pts',(-0.226743379782759,0.0161700948643406,
-0.00387393372333392));
#46636=CARTESIAN_POINT('Ctrl Pts',(-0.227309431860278,0.0159880923504392,
-0.00485196380139293));
#46637=CARTESIAN_POINT('Ctrl Pts',(-0.227391181903299,0.0160099755008125,
-0.00479277052584003));
#46638=CARTESIAN_POINT('Ctrl Pts',(-0.227389517585843,0.015912267948463,
-0.00475943666660673));
#46639=CARTESIAN_POINT('Ctrl Pts',(-0.228028119018682,0.0156603845179188,
-0.00565588952548107));
#46640=CARTESIAN_POINT('Ctrl Pts',(-0.228105108350196,0.0156905302113713,
-0.00559393310834394));
#46641=CARTESIAN_POINT('Ctrl Pts',(-0.228103863210623,0.0155962483295275,
-0.00555167686899847));
#46642=CARTESIAN_POINT('Ctrl Pts',(-0.228802757285458,0.0152823868470796,
-0.00638961457773919));
#46643=CARTESIAN_POINT('Ctrl Pts',(-0.228875533245265,0.0153203957783105,
-0.00632681833521576));
#46644=CARTESIAN_POINT('Ctrl Pts',(-0.228874614212836,0.0152301844971178,
-0.00627636725223939));
#46645=CARTESIAN_POINT('Ctrl Pts',(-0.229627994727228,0.0148670422144861,
-0.00705276295927651));
#46646=CARTESIAN_POINT('Ctrl Pts',(-0.229696602632231,0.0149126078655,-0.00699024645412036));
#46647=CARTESIAN_POINT('Ctrl Pts',(-0.229695993342631,0.0148268265883492,
-0.00693249486514969));
#46648=CARTESIAN_POINT('Ctrl Pts',(-0.230481878170306,0.01442369053443,
-0.00765169618674575));
#46649=CARTESIAN_POINT('Ctrl Pts',(-0.230549279564022,0.0144748984918072,
-0.00759242459387856));
#46650=CARTESIAN_POINT('Ctrl Pts',(-0.230549019547242,0.014393931285933,
-0.00752807881257224));
#46651=CARTESIAN_POINT('Ctrl Pts',(-0.231177467493998,0.014003890473077,
-0.00813697751827833));
#46652=CARTESIAN_POINT('Ctrl Pts',(-0.231249685385162,0.0140565675637169,
-0.00808465444694161));
#46653=CARTESIAN_POINT('Ctrl Pts',(-0.231249658084979,0.0139803452106898,
-0.00801487102447448));
#46654=CARTESIAN_POINT('Ctrl Pts',(-0.231670728309359,0.0135947224063574,
-0.00854712336180957));
#46655=CARTESIAN_POINT('Ctrl Pts',(-0.231752619804048,0.0136426772192251,
-0.00850601156601645));
#46656=CARTESIAN_POINT('Ctrl Pts',(-0.231752693652761,0.0135714697124679,
-0.00843141437557248));
#46657=CARTESIAN_POINT('Ctrl Pts',(-0.231966406597232,0.0132362082644641,
-0.00887116443097536));
#46658=CARTESIAN_POINT('Ctrl Pts',(-0.232062273088291,0.0132709718533777,
-0.00884649553010581));
#46659=CARTESIAN_POINT('Ctrl Pts',(-0.232062481656899,0.0132042914499902,
-0.0087681741575853));
#46660=CARTESIAN_POINT('Ctrl Pts',(-0.232089783925324,0.0127867877948663,
-0.00922721017894486));
#46661=CARTESIAN_POINT('Ctrl Pts',(-0.232195444754471,0.0127888549173578,
-0.00923064524789568));
#46662=CARTESIAN_POINT('Ctrl Pts',(-0.232195795965022,0.0127281581789461,
-0.00914789582704976));
#46663=CARTESIAN_POINT('Ctrl Pts',(-0.231968971356067,0.0123157844703992,
-0.00954672899977835));
#46664=CARTESIAN_POINT('Ctrl Pts',(-0.232065675411668,0.012285771447896,
-0.00957008688076997));
#46665=CARTESIAN_POINT('Ctrl Pts',(-0.232066144322818,0.0122309820328145,
-0.00948309977348297));
#46666=CARTESIAN_POINT('Ctrl Pts',(-0.231720771626718,0.0118689957268499,
-0.00980836544689196));
#46667=CARTESIAN_POINT('Ctrl Pts',(-0.231809935349982,0.0118256369660778,
-0.00983624870656414));
#46668=CARTESIAN_POINT('Ctrl Pts',(-0.231810485252569,0.0117760634407629,
-0.00974603498528647));
#46669=CARTESIAN_POINT('Ctrl Pts',(-0.231315018306534,0.0113053865717837,
-0.0100956259794169));
#46670=CARTESIAN_POINT('Ctrl Pts',(-0.231397271592812,0.0112501747778728,
-0.0101251515102169));
#46671=CARTESIAN_POINT('Ctrl Pts',(-0.23139798144253,0.011207353978372,
-0.0100313194005554));
#46672=CARTESIAN_POINT('Ctrl Pts',(-0.23072504796845,0.010615585256532,
-0.0103774887010382));
#46673=CARTESIAN_POINT('Ctrl Pts',(-0.230803651447536,0.0105540854545879,
-0.0104034766730699));
#46674=CARTESIAN_POINT('Ctrl Pts',(-0.230804445927653,0.0105194090449751,
-0.0103062150531577));
#46675=CARTESIAN_POINT('Ctrl Pts',(-0.229647060853282,0.00942256760179786,
-0.0107297449576376));
#46676=CARTESIAN_POINT('Ctrl Pts',(-0.229722099652704,0.00935373083032424,
-0.0107480730605707));
#46677=CARTESIAN_POINT('Ctrl Pts',(-0.229723102517257,0.00933302452585627,
-0.0106465471042351));
#46678=CARTESIAN_POINT('Ctrl Pts',(-0.228778830421403,0.00850199841465629,
-0.0108449553313066));
#46679=CARTESIAN_POINT('Ctrl Pts',(-0.228855210405385,0.00843344082546064,
-0.0108554634871318));
#46680=CARTESIAN_POINT('Ctrl Pts',(-0.228856077356639,0.00842299482164084,
-0.0107526226063158));
#46681=CARTESIAN_POINT('Ctrl Pts',(-0.228206393600378,0.00780936869860245,
-0.0108644994342279));
#46682=CARTESIAN_POINT('Ctrl Pts',(-0.228284049039534,0.00774147764959962,
-0.0108702768244508));
#46683=CARTESIAN_POINT('Ctrl Pts',(-0.228285021567739,0.00773913782172368,
-0.010767089034139));
#46684=CARTESIAN_POINT('Ctrl Pts',(-0.225009750798511,0.0164742919676833,
-2.94234935793932E-7));
#46685=CARTESIAN_POINT('Ctrl Pts',(-0.225009853509087,0.0164809894657856,
-2.94108435594111E-7));
#46686=CARTESIAN_POINT('Ctrl Pts',(-0.225009248162902,0.0164876738465301,
-2.94985003331512E-7));
#46687=CARTESIAN_POINT('Ctrl Pts',(-0.225006557138774,0.0165012782295379,
-2.98820133665149E-7));
#46688=CARTESIAN_POINT('Ctrl Pts',(-0.225004381157442,0.0165081277083827,
-3.01905547296842E-7));
#46689=CARTESIAN_POINT('Ctrl Pts',(-0.224996139283575,0.0165266941161087,
-3.13528887012115E-7));
#46690=CARTESIAN_POINT('Ctrl Pts',(-0.224988442162309,0.0165374948473636,
-3.24342008419143E-7));
#46691=CARTESIAN_POINT('Ctrl Pts',(-0.224969252270092,0.016555753366864,
-3.5089401941877E-7));
#46692=CARTESIAN_POINT('Ctrl Pts',(-0.224957889791733,0.0165629935330378,
-3.66636042736974E-7));
#46693=CARTESIAN_POINT('Ctrl Pts',(-0.224933916678097,0.0165726615164696,
-3.97335259411207E-7));
#46694=CARTESIAN_POINT('Ctrl Pts',(-0.224922798675663,0.0165748188773007,
-4.30993709014285E-7));
#46695=CARTESIAN_POINT('Ctrl Pts',(-0.224910907505475,0.0165757632925934,
-3.97281805675274E-7));
#46696=CARTESIAN_POINT('Ctrl Pts',(-0.224908458936007,0.0165758792333304,
-4.40024533364447E-7));
#46697=CARTESIAN_POINT('Ctrl Pts',(-0.224906181933197,0.0165759154128579,
-4.43226285311814E-7));
#46698=CARTESIAN_POINT('Origin',(-0.226648799791358,0.00779550107807324,
0.0018430762351178));
#46699=CARTESIAN_POINT('Ctrl Pts',(-0.225192864155308,0.00215336583509703,
0.00904010670453624));
#46700=CARTESIAN_POINT('Ctrl Pts',(-0.225204706288654,0.00216933111886313,
0.00905188432053952));
#46701=CARTESIAN_POINT('Ctrl Pts',(-0.225224728767847,0.00220285845149844,
0.00906873009866757));
#46702=CARTESIAN_POINT('Ctrl Pts',(-0.225240738467706,0.00223802863421344,
0.00907116763090578));
#46703=CARTESIAN_POINT('Ctrl Pts',(-0.22525674809356,0.00227319865435349,
0.00907360515187645));
#46704=CARTESIAN_POINT('Ctrl Pts',(-0.225269616920643,0.00230901002534829,
0.00906077332273702));
#46705=CARTESIAN_POINT('Ctrl Pts',(-0.225269618511371,0.00232397812765925,
0.00904117190417335));
#46706=CARTESIAN_POINT('Ctrl Pts',(-0.224423102415366,0.0164240572405408,
-0.0017009526594877));
#46707=CARTESIAN_POINT('Ctrl Pts',(-0.22442753931816,0.0165274809959018,
-0.00170826230446446));
#46708=CARTESIAN_POINT('Ctrl Pts',(-0.224328623267926,0.0165310813381061,
-0.00167531627545616));
#46709=CARTESIAN_POINT('Ctrl Pts',(-0.224888576396618,0.0165068622639915,
-0.000507779096031469));
#46710=CARTESIAN_POINT('Ctrl Pts',(-0.224890080375599,0.0166106061384932,
-0.000507850690853431));
#46711=CARTESIAN_POINT('Ctrl Pts',(-0.224792054255541,0.0166074069025231,
-0.000476013916690959));
#46712=CARTESIAN_POINT('Ctrl Pts',(-0.225297934651115,0.0164656143571788,
0.00113605080611901));
#46713=CARTESIAN_POINT('Ctrl Pts',(-0.22530166511579,0.0165690618324774,
0.00113577106828663));
#46714=CARTESIAN_POINT('Ctrl Pts',(-0.225201608773796,0.0165702170608381,
0.00116603472722438));
#46715=CARTESIAN_POINT('Ctrl Pts',(-0.226160156840923,0.0163464165517524,
0.00293824900518469));
#46716=CARTESIAN_POINT('Ctrl Pts',(-0.226162443178585,0.0164497276877427,
0.00295095984804816));
#46717=CARTESIAN_POINT('Ctrl Pts',(-0.226070274722855,0.0164421273393253,
0.00299861916200696));
#46718=CARTESIAN_POINT('Ctrl Pts',(-0.226875182678137,0.0161110455835552,
0.00419057100130972));
#46719=CARTESIAN_POINT('Ctrl Pts',(-0.226876732829769,0.0162117033653627,
0.00421805256419852));
#46720=CARTESIAN_POINT('Ctrl Pts',(-0.226788904849661,0.016194807216906,
0.00427157151275447));
#46721=CARTESIAN_POINT('Ctrl Pts',(-0.227956254663923,0.0156144693913653,
0.00560704096080674));
#46722=CARTESIAN_POINT('Ctrl Pts',(-0.227957828737694,0.0157095212737186,
0.00565098557902036));
#46723=CARTESIAN_POINT('Ctrl Pts',(-0.227877264381436,0.0156793865260549,
0.00571072697276061));
#46724=CARTESIAN_POINT('Ctrl Pts',(-0.229210309208534,0.0149506460476673,
0.00676589468964074));
#46725=CARTESIAN_POINT('Ctrl Pts',(-0.229210872891863,0.0150384255713987,
0.00682253731830502));
#46726=CARTESIAN_POINT('Ctrl Pts',(-0.229137956318801,0.0149947728795728,
0.00688320487905378));
#46727=CARTESIAN_POINT('Ctrl Pts',(-0.230287556148017,0.0143461956309686,
0.00758447983064182));
#46728=CARTESIAN_POINT('Ctrl Pts',(-0.230287717729031,0.01442714587865,
0.0076503219879991));
#46729=CARTESIAN_POINT('Ctrl Pts',(-0.23021627985812,0.0143760462362006,
0.00770647349494255));
#46730=CARTESIAN_POINT('Ctrl Pts',(-0.230951348226825,0.0139153574913946,
0.00807928185038737));
#46731=CARTESIAN_POINT('Ctrl Pts',(-0.230951233983676,0.0139913315871583,
0.00815069361700217));
#46732=CARTESIAN_POINT('Ctrl Pts',(-0.230876037824531,0.0139384580487563,
0.00820029147724192));
#46733=CARTESIAN_POINT('Ctrl Pts',(-0.231432809970025,0.0135059184053885,
0.00848700995994168));
#46734=CARTESIAN_POINT('Ctrl Pts',(-0.231432584554041,0.0135768401502669,
0.00856317562692272));
#46735=CARTESIAN_POINT('Ctrl Pts',(-0.231349537669097,0.0135278627464521,
0.00860273139657538));
#46736=CARTESIAN_POINT('Ctrl Pts',(-0.231745465211004,0.0131461000136674,
0.00881019374563095));
#46737=CARTESIAN_POINT('Ctrl Pts',(-0.231745063580486,0.013212670154277,
0.00888993882945493));
#46738=CARTESIAN_POINT('Ctrl Pts',(-0.231651625200096,0.0131728945446976,
0.00891695333527741));
#46739=CARTESIAN_POINT('Ctrl Pts',(-0.231924372807378,0.0126958161713031,
0.0091657531528894));
#46740=CARTESIAN_POINT('Ctrl Pts',(-0.231923809183617,0.0127567627508423,
0.00924952970467843));
#46741=CARTESIAN_POINT('Ctrl Pts',(-0.231818227394473,0.0127436564621929,
0.00925272722690912));
#46742=CARTESIAN_POINT('Ctrl Pts',(-0.231871582732807,0.0121954486342374,
0.00950210157316456));
#46743=CARTESIAN_POINT('Ctrl Pts',(-0.231870910432785,0.012250396442285,
0.00959002308213435));
#46744=CARTESIAN_POINT('Ctrl Pts',(-0.231769686742723,0.012271888694355,
0.00957067213786439));
#46745=CARTESIAN_POINT('Ctrl Pts',(-0.231655490809696,0.0117298373815043,
0.00976870709561953));
#46746=CARTESIAN_POINT('Ctrl Pts',(-0.231654730412008,0.0117793811745959,
0.00985996820273655));
#46747=CARTESIAN_POINT('Ctrl Pts',(-0.231561990926401,0.0118183205410903,
0.00983340751634403));
#46748=CARTESIAN_POINT('Ctrl Pts',(-0.231272911021964,0.0111462630541763,
0.0100571125220447));
#46749=CARTESIAN_POINT('Ctrl Pts',(-0.231272010484576,0.011188849482947,
0.0101520756394755));
#46750=CARTESIAN_POINT('Ctrl Pts',(-0.23118753117075,0.0112425848166589,
0.0101223341433138));
#46751=CARTESIAN_POINT('Ctrl Pts',(-0.230703596413716,0.0104641706532134,
0.010323445088338));
#46752=CARTESIAN_POINT('Ctrl Pts',(-0.230702628925254,0.0104986298412639,
0.0104217843528756));
#46753=CARTESIAN_POINT('Ctrl Pts',(-0.230622791844109,0.0105598058105489,
0.0103951096952851));
#46754=CARTESIAN_POINT('Ctrl Pts',(-0.229654376601397,0.00928919713295885,
0.0106537304156924));
#46755=CARTESIAN_POINT('Ctrl Pts',(-0.229653231650024,0.00930975120703328,
0.0107562426244593));
#46756=CARTESIAN_POINT('Ctrl Pts',(-0.229576535600367,0.00937798854178594,
0.0107371719305779));
#46757=CARTESIAN_POINT('Ctrl Pts',(-0.22880130602491,0.00837465238807093,
0.0107570024335721));
#46758=CARTESIAN_POINT('Ctrl Pts',(-0.228800187139004,0.00838466046235115,
0.0108608767335588));
#46759=CARTESIAN_POINT('Ctrl Pts',(-0.228723594842368,0.00845424764654016,
0.0108493022767735));
#46760=CARTESIAN_POINT('Ctrl Pts',(-0.228220153777608,0.00770395662147991,
0.010764867331218));
#46761=CARTESIAN_POINT('Ctrl Pts',(-0.228219244623913,0.00770629588168661,
0.0108689369194601));
#46762=CARTESIAN_POINT('Ctrl Pts',(-0.228139692445573,0.00777347521877263,
0.0108625950646913));
#46763=CARTESIAN_POINT('Ctrl Pts',(-0.229319785018526,0.00893281966668023,
0.0106733205234826));
#46764=CARTESIAN_POINT('Ctrl Pts',(-0.229318259485533,0.00894418630796205,
0.0107410766231035));
#46765=CARTESIAN_POINT('Ctrl Pts',(-0.229320209696457,0.00903641302211148,
0.0107575141350037));
#46766=CARTESIAN_POINT('Ctrl Pts',(-0.229322271958198,0.00910280340307577,
0.0107454877379686));
#46767=CARTESIAN_POINT('Origin',(-0.22504807827475,0.00267369066304345,
0.00928633187534054));
#46768=CARTESIAN_POINT('Ctrl Pts',(-0.224893951312673,0.00215954182917785,
0.00903842305818316));
#46769=CARTESIAN_POINT('Ctrl Pts',(-0.224911141103877,0.00216992176564713,
0.00904603151524389));
#46770=CARTESIAN_POINT('Ctrl Pts',(-0.224951134219812,0.00219064274957742,
0.0090535915278308));
#46771=CARTESIAN_POINT('Ctrl Pts',(-0.22497913921113,0.00221947895890837,
0.00904507092145141));
#46772=CARTESIAN_POINT('Ctrl Pts',(-0.225002380419073,0.00224340999069353,
0.00903799971109383));
#46773=CARTESIAN_POINT('Ctrl Pts',(-0.225014260642788,0.00227143120128385,
0.00902261128732804));
#46774=CARTESIAN_POINT('Ctrl Pts',(-0.225014720871232,0.00228334524727118,
0.0090072968842552));
#46775=CARTESIAN_POINT('Ctrl Pts',(-0.229620207397339,0.00855813827595884,
0.0107332969856487));
#46776=CARTESIAN_POINT('Ctrl Pts',(-0.229616538665817,0.00857090518029757,
0.0108412348410576));
#46777=CARTESIAN_POINT('Ctrl Pts',(-0.229701615329559,0.00863731696429406,
0.0108269786528085));
#46778=CARTESIAN_POINT('Ctrl Pts',(-0.22903299248322,0.00930406829717384,
0.0106244444186668));
#46779=CARTESIAN_POINT('Ctrl Pts',(-0.229029268207648,0.00932610885666542,
0.0107311427610987));
#46780=CARTESIAN_POINT('Ctrl Pts',(-0.229113325739694,0.00939167115900597,
0.0107118574650714));
#46781=CARTESIAN_POINT('Ctrl Pts',(-0.228116908040458,0.0103192133070879,
0.0103716166304235));
#46782=CARTESIAN_POINT('Ctrl Pts',(-0.228113961793712,0.010352440661458,
0.0104760412785541));
#46783=CARTESIAN_POINT('Ctrl Pts',(-0.228201379265707,0.0104150729421031,
0.0104460896936027));
#46784=CARTESIAN_POINT('Ctrl Pts',(-0.22728197906512,0.0119325496639152,
0.00959955446290684));
#46785=CARTESIAN_POINT('Ctrl Pts',(-0.227279031174141,0.0119862717024164,
0.00969406047754389));
#46786=CARTESIAN_POINT('Ctrl Pts',(-0.227383186150131,0.0120112033292314,
0.00967194223499914));
#46787=CARTESIAN_POINT('Ctrl Pts',(-0.227034169568235,0.0127020208624721,
0.00907567277747115));
#46788=CARTESIAN_POINT('Ctrl Pts',(-0.227031194864248,0.0127655060260149,
0.00916367976789601));
#46789=CARTESIAN_POINT('Ctrl Pts',(-0.227134428282106,0.0127877316141476,
0.00914076544299377));
#46790=CARTESIAN_POINT('Ctrl Pts',(-0.226856974623676,0.0131107264396041,
0.00873962932632364));
#46791=CARTESIAN_POINT('Ctrl Pts',(-0.226854228559386,0.013178989557894,
0.00882371307415828));
#46792=CARTESIAN_POINT('Ctrl Pts',(-0.226957558425783,0.0132004200200363,
0.00879837917996526));
#46793=CARTESIAN_POINT('Ctrl Pts',(-0.22709761102,0.0128296959531864,0.00908953899803701));
#46794=CARTESIAN_POINT('Ctrl Pts',(-0.227097896903337,0.0128293463272935,
0.00908980452749194));
#46795=CARTESIAN_POINT('Ctrl Pts',(-0.227097980985701,0.0128291697025301,
0.00908993637037429));
#46796=CARTESIAN_POINT('Ctrl Pts',(-0.22709798906973,0.0128291516969385,
0.00908994979281978));
#46797=CARTESIAN_POINT('Ctrl Pts',(-0.227097999108598,0.0128291278282252,
0.0090899675611068));
#46798=CARTESIAN_POINT('Ctrl Pts',(-0.227098001470723,0.012829122091011,
0.00908997183012093));
#46799=CARTESIAN_POINT('Ctrl Pts',(-0.227098006026732,0.0128291107783129,
0.0090899802440751));
#46800=CARTESIAN_POINT('Ctrl Pts',(-0.2270980082234,0.0128291052041497,
0.00908998438815479));
#46801=CARTESIAN_POINT('Ctrl Pts',(-0.227098013190528,0.0128290923132555,
0.00908999396767163));
#46802=CARTESIAN_POINT('Ctrl Pts',(-0.227098015929209,0.0128290849890549,
0.00908999940738772));
#46803=CARTESIAN_POINT('Ctrl Pts',(-0.227098021113615,0.0128290706815099,
0.00909001002758949));
#46804=CARTESIAN_POINT('Ctrl Pts',(-0.227098023566733,0.0128290637014166,
0.00909001520597644));
#46805=CARTESIAN_POINT('Ctrl Pts',(-0.227098030839428,0.0128290423360304,
0.00909003104784491));
#46806=CARTESIAN_POINT('Ctrl Pts',(-0.227098035427359,0.01282902790273,
0.00909004173781594));
#46807=CARTESIAN_POINT('Ctrl Pts',(-0.227098087132581,0.012828852541214,
0.00909017147004589));
#46808=CARTESIAN_POINT('Ctrl Pts',(-0.227098092975546,0.012828693757072,
0.00909028745450568));
#46809=CARTESIAN_POINT('Ctrl Pts',(-0.227098036381531,0.0128283795127757,
0.00909051412772828));
#46810=CARTESIAN_POINT('Ctrl Pts',(-0.227097981119594,0.0128282316182478,
0.00909061957142001));
#46811=CARTESIAN_POINT('Ctrl Pts',(-0.22709781509159,0.0128278855864363,
0.00909086411088216));
#46812=CARTESIAN_POINT('Ctrl Pts',(-0.22709768022983,0.0128276751102533,
0.00909101080013109));
#46813=CARTESIAN_POINT('Ctrl Pts',(-0.227097330399864,0.0128271776743247,
0.00909135402846317));
#46814=CARTESIAN_POINT('Ctrl Pts',(-0.22709706096517,0.0128268448743511,
0.00909157963435271));
#46815=CARTESIAN_POINT('Ctrl Pts',(-0.227096353084741,0.0128260014481448,
0.00909214351272337));
#46816=CARTESIAN_POINT('Ctrl Pts',(-0.227095796735987,0.0128253813011885,
0.00909254670859746));
#46817=CARTESIAN_POINT('Ctrl Pts',(-0.227093819503803,0.0128231928490514,
0.00909393301778212));
#46818=CARTESIAN_POINT('Ctrl Pts',(-0.227092192667826,0.0128214263144734,
0.00909497481582912));
#46819=CARTESIAN_POINT('Ctrl Pts',(-0.22708508832393,0.0128134962161041,
0.00909924848525208));
#46820=CARTESIAN_POINT('Ctrl Pts',(-0.227079680338992,0.0128070270610738,
0.00910182504888053));
#46821=CARTESIAN_POINT('Ctrl Pts',(-0.227065324825336,0.0127883677251284,
0.00910683477824836));
#46822=CARTESIAN_POINT('Ctrl Pts',(-0.22705668742453,0.0127754892527389,
0.0091077276220021));
#46823=CARTESIAN_POINT('Ctrl Pts',(-0.227042441902929,0.0127503795925126,
0.00910418707108994));
#46824=CARTESIAN_POINT('Ctrl Pts',(-0.227036677809703,0.0127382988866502,
0.00910026136023822));
#46825=CARTESIAN_POINT('Ctrl Pts',(-0.227030063463232,0.012720118593403,
0.00909009366612189));
#46826=CARTESIAN_POINT('Ctrl Pts',(-0.227028200856115,0.0127136996055961,
0.00908552597126478));
#46827=CARTESIAN_POINT('Ctrl Pts',(-0.227025944415882,0.012702340715504,
0.00907528610289493));
#46828=CARTESIAN_POINT('Ctrl Pts',(-0.227025454709595,0.0126974045244964,
0.00906981769686516));
#46829=CARTESIAN_POINT('Ctrl Pts',(-0.22702558160064,0.0126930625462286,
0.0090638516120818));
#46830=CARTESIAN_POINT('Origin',(-0.221493379745634,0.00394271703026399,
0.00803042653342771));
#46831=CARTESIAN_POINT('Ctrl Pts',(-0.225016038306626,0.00296527640567411,
0.00956936262132929));
#46832=CARTESIAN_POINT('Ctrl Pts',(-0.225054837504787,0.00296676909900014,
0.0095710276794746));
#46833=CARTESIAN_POINT('Ctrl Pts',(-0.225088091302381,0.00298068453682126,
0.0095516424980561));
#46834=CARTESIAN_POINT('Ctrl Pts',(-0.225103269221005,0.00299367647273647,
0.0095306661184691));
#46835=CARTESIAN_POINT('Ctrl Pts',(-0.225113739935693,0.00300263915448291,
0.00951619524856506));
#46836=CARTESIAN_POINT('Ctrl Pts',(-0.225117785239288,0.00301142193691076,
0.00950115649627434));
#46837=CARTESIAN_POINT('Ctrl Pts',(-0.225118071269482,0.00301949283818061,
0.00948729957575529));
#46838=CARTESIAN_POINT('Origin',(-0.226780511856133,0.0100405374416167,
0.0110051741771939));
#46839=CARTESIAN_POINT('Ctrl Pts',(-0.226273558818709,0.0126615507097427,
0.00907157974325745));
#46840=CARTESIAN_POINT('Ctrl Pts',(-0.226273018871854,0.0126830229129793,
0.00910141756778122));
#46841=CARTESIAN_POINT('Ctrl Pts',(-0.226298864402728,0.0127209315695524,
0.00910908677761961));
#46842=CARTESIAN_POINT('Ctrl Pts',(-0.226321295777411,0.0127454310152486,
0.00910934848928192));
#46843=CARTESIAN_POINT('Ctrl Pts',(-0.226340598417199,0.0127665132708808,
0.00910957369732274));
#46844=CARTESIAN_POINT('Ctrl Pts',(-0.226353873932747,0.0127801920629709,
0.00910660552022882));
#46845=CARTESIAN_POINT('Ctrl Pts',(-0.226383304101992,0.0128042931570195,
0.0090932051586158));
#46846=CARTESIAN_POINT('Ctrl Pts',(-0.22638807437404,0.0128081996508736,
0.00909103312318123));
#46847=CARTESIAN_POINT('Ctrl Pts',(-0.226393292302312,0.0128123158788516,
0.0090885067005233));
#46848=CARTESIAN_POINT('Ctrl Pts',(-0.226399047297907,0.0128166255196227,
0.00908546833389411));
#46849=CARTESIAN_POINT('Ctrl Pts',(-0.225133546245736,0.0079572727413433,
0.0106839114428361));
#46850=CARTESIAN_POINT('Ctrl Pts',(-0.225131202582991,0.00796280010051278,
0.0107879669222465));
#46851=CARTESIAN_POINT('Ctrl Pts',(-0.225027565196397,0.00797114141935883,
0.0107807941497949));
#46852=CARTESIAN_POINT('Ctrl Pts',(-0.225049122764504,0.00703055902368649,
0.0107304119903276));
#46853=CARTESIAN_POINT('Ctrl Pts',(-0.225046767464602,0.00702503046949575,
0.0108350360113988));
#46854=CARTESIAN_POINT('Ctrl Pts',(-0.224943244930424,0.00703596129787379,
0.0108290232843219));
#46855=CARTESIAN_POINT('Ctrl Pts',(-0.224889836960112,0.00513717572956065,
0.0105283887484728));
#46856=CARTESIAN_POINT('Ctrl Pts',(-0.224887538335525,0.00510991286636644,
0.0106307975956611));
#46857=CARTESIAN_POINT('Ctrl Pts',(-0.224783218214591,0.0051108634611282,
0.0106258911999091));
#46858=CARTESIAN_POINT('Ctrl Pts',(-0.225023719104184,0.00339280049023757,
0.00974486159724177));
#46859=CARTESIAN_POINT('Ctrl Pts',(-0.225021774812465,0.00334449320283454,
0.00983783365658757));
#46860=CARTESIAN_POINT('Ctrl Pts',(-0.224917880936671,0.0033382150606942,
0.00982841550280784));
#46861=CARTESIAN_POINT('Ctrl Pts',(-0.225194501068205,0.00263332843217836,
0.00925026456232951));
#46862=CARTESIAN_POINT('Ctrl Pts',(-0.225192783985461,0.00257626916693201,
0.00933748070290354));
#46863=CARTESIAN_POINT('Ctrl Pts',(-0.22509059122008,0.00256284175228321,
0.00932156835961672));
#46864=CARTESIAN_POINT('Ctrl Pts',(-0.225092271993048,0.0074950696415353,
0.0106948847060478));
#46865=CARTESIAN_POINT('Ctrl Pts',(-0.225092124042334,0.00749506551951806,
0.0107014292645462));
#46866=CARTESIAN_POINT('Ctrl Pts',(-0.225091331424227,0.00749506162327073,
0.0107079429871891));
#46867=CARTESIAN_POINT('Ctrl Pts',(-0.225088389756039,0.00749505407695255,
0.0107211269286868));
#46868=CARTESIAN_POINT('Ctrl Pts',(-0.225086166021754,0.00749505048060983,
0.0107277438866657));
#46869=CARTESIAN_POINT('Ctrl Pts',(-0.225077916451027,0.00749504104297401,
0.0107457912927371));
#46870=CARTESIAN_POINT('Ctrl Pts',(-0.225070344089698,0.00749503606449245,
0.0107563590318577));
#46871=CARTESIAN_POINT('Ctrl Pts',(-0.225051607693862,0.00749502702891778,
0.0107740521520703));
#46872=CARTESIAN_POINT('Ctrl Pts',(-0.225040617287013,0.0074950240544077,
0.0107810108087723));
#46873=CARTESIAN_POINT('Ctrl Pts',(-0.225011582445515,0.00749500389423601,
0.0107923667013775));
#46874=CARTESIAN_POINT('Ctrl Pts',(-0.224997392673719,0.00749510403851621,
0.0107925601345168));
#46875=CARTESIAN_POINT('Ctrl Pts',(-0.224992643923633,0.00749468154582047,
0.010792618809641));
#46876=CARTESIAN_POINT('Ctrl Pts',(-0.224992118552164,0.00749461327975819,
0.0107926204901728));
#46877=CARTESIAN_POINT('Ctrl Pts',(-0.224991378287202,0.00749441910071412,
0.0107926185236326));
#46878=CARTESIAN_POINT('Ctrl Pts',(-0.224991133735545,0.00749431857707768,
0.0107926165100084));
#46879=CARTESIAN_POINT('Ctrl Pts',(-0.224990604703868,0.00749391093596826,
0.0107926104063756));
#46880=CARTESIAN_POINT('Origin',(-0.227808378362649,0.00719112862353373,
0.00185696123111253));
#46881=CARTESIAN_POINT('Ctrl Pts',(-0.226520627867466,0.0132597435976571,
0.00874175744832851));
#46882=CARTESIAN_POINT('Ctrl Pts',(-0.226487176491317,0.0132389482725006,
0.0087584114230379));
#46883=CARTESIAN_POINT('Ctrl Pts',(-0.226470495664087,0.0132231203056123,
0.00876329055696138));
#46884=CARTESIAN_POINT('Ctrl Pts',(-0.226449937155245,0.0132037737465187,
0.00876353000619182));
#46885=CARTESIAN_POINT('Ctrl Pts',(-0.226447721306919,0.0132016885252163,
0.00876355581463836));
#46886=CARTESIAN_POINT('Ctrl Pts',(-0.226445475166781,0.0131995315973307,
0.00876349525475088));
#46887=CARTESIAN_POINT('Ctrl Pts',(-0.226443190924595,0.0131972703049045,
0.0087633363683377));
#46888=CARTESIAN_POINT('Ctrl Pts',(-0.226421963144674,0.013176255800291,
0.00876185981483047));
#46889=CARTESIAN_POINT('Ctrl Pts',(-0.226400801825894,0.0131437796706972,
0.00875009709576872));
#46890=CARTESIAN_POINT('Ctrl Pts',(-0.226398183046263,0.0131243802924447,
0.008731911942556));
#46891=CARTESIAN_POINT('Ctrl Pts',(-0.226397905532036,0.0131223245244056,
0.00872998484694108));
#46892=CARTESIAN_POINT('Ctrl Pts',(-0.226397790265506,0.013120436131916,
0.00872799650275696));
#46893=CARTESIAN_POINT('Ctrl Pts',(-0.226397825284883,0.0131187534369297,
0.00872595188639632));
#46894=CARTESIAN_POINT('Ctrl Pts',(-0.225190041859337,0.0123109312972237,
0.00928452960023628));
#46895=CARTESIAN_POINT('Ctrl Pts',(-0.225189716453424,0.0123699621157433,
0.00937667255010711));
#46896=CARTESIAN_POINT('Ctrl Pts',(-0.225082687608397,0.012381811054789,
0.00935700919890517));
#46897=CARTESIAN_POINT('Ctrl Pts',(-0.224849534335206,0.0107686015790774,
0.0102729844456006));
#46898=CARTESIAN_POINT('Ctrl Pts',(-0.224848828147693,0.0108091195061921,
0.0103769377881753));
#46899=CARTESIAN_POINT('Ctrl Pts',(-0.224738109563861,0.0108069665241362,
0.0103708724457372));
#46900=CARTESIAN_POINT('Ctrl Pts',(-0.224962173305664,0.00887287258771333,
0.0107780555327175));
#46901=CARTESIAN_POINT('Ctrl Pts',(-0.224961178899313,0.00888991514828659,
0.0108886125707888));
#46902=CARTESIAN_POINT('Ctrl Pts',(-0.224853022929204,0.00887733942185127,
0.0108791940235274));
#46903=CARTESIAN_POINT('Ctrl Pts',(-0.225133451501574,0.00703771621441337,
0.0106819139847117));
#46904=CARTESIAN_POINT('Ctrl Pts',(-0.225132505084545,0.00703201791455483,
0.0107911553449083));
#46905=CARTESIAN_POINT('Ctrl Pts',(-0.225024003315464,0.00702327394296394,
0.0107799226729097));
#46906=CARTESIAN_POINT('Ctrl Pts',(-0.22511470191617,0.0119224377252866,
0.00952072100618005));
#46907=CARTESIAN_POINT('Ctrl Pts',(-0.225114237492274,0.0119352596408989,
0.00954312606581834));
#46908=CARTESIAN_POINT('Ctrl Pts',(-0.2251037365202,0.011950952820735,0.00957078918542189));
#46909=CARTESIAN_POINT('Ctrl Pts',(-0.225072256833985,0.0119632244350986,
0.00958934476625811));
#46910=CARTESIAN_POINT('Ctrl Pts',(-0.225056268536952,0.0119694570961923,
0.00959876900689375));
#46911=CARTESIAN_POINT('Ctrl Pts',(-0.225034719043819,0.0119741726577803,
0.00960469177404778));
#46912=CARTESIAN_POINT('Ctrl Pts',(-0.225012478416595,0.0119747498425115,
0.00960390435316071));
#46913=CARTESIAN_POINT('Origin',(-0.225236894197425,0.0131978724148554,
0.00863903100067282));
#46914=CARTESIAN_POINT('Ctrl Pts',(-0.225398010193384,0.013120318400212,
0.00870574369815946));
#46915=CARTESIAN_POINT('Ctrl Pts',(-0.22539764807259,0.0131371343383082,
0.00872622181582472));
#46916=CARTESIAN_POINT('Ctrl Pts',(-0.225383644932907,0.0131694250657152,
0.00874116107965085));
#46917=CARTESIAN_POINT('Ctrl Pts',(-0.225369785250098,0.0131944797608948,
0.00874167639760945));
#46918=CARTESIAN_POINT('Ctrl Pts',(-0.225357073815439,0.0132174587226127,
0.00874214902246313));
#46919=CARTESIAN_POINT('Ctrl Pts',(-0.225344323092837,0.0132335688478599,
0.00873837016524198));
#46920=CARTESIAN_POINT('Ctrl Pts',(-0.225322671626811,0.0132555887805521,
0.00872233569144969));
#46921=CARTESIAN_POINT('Ctrl Pts',(-0.225320715789482,0.0132575779025037,
0.00872088725269888));
#46922=CARTESIAN_POINT('Ctrl Pts',(-0.225318687903922,0.0132595961215726,
0.0087193083418805));
#46923=CARTESIAN_POINT('Ctrl Pts',(-0.225316581766884,0.0132616346613913,
0.00871757524912672));
#46924=CARTESIAN_POINT('Origin',(-0.22097494585212,0.0105087759000406,0.00743958985954961));
#46925=CARTESIAN_POINT('Ctrl Pts',(-0.224871009513959,0.0128386119989575,
0.00903955781216604));
#46926=CARTESIAN_POINT('Ctrl Pts',(-0.224916241833165,0.0128120209719476,
0.00906116586928584));
#46927=CARTESIAN_POINT('Ctrl Pts',(-0.224949040953459,0.0127765826465377,
0.00905521952879191));
#46928=CARTESIAN_POINT('Ctrl Pts',(-0.224969134043051,0.0127528695470433,
0.00904336442625093));
#46929=CARTESIAN_POINT('Ctrl Pts',(-0.224983890367304,0.0127354546948581,
0.00903465806298362));
#46930=CARTESIAN_POINT('Ctrl Pts',(-0.224992190595086,0.0127224256089223,
0.0090226133050689));
#46931=CARTESIAN_POINT('Ctrl Pts',(-0.22499258838655,0.0127125317992707,
0.00900988833309594));
#46932=CARTESIAN_POINT('Origin',(-0.226669448078697,0.00719407473391473,
0.00184050621984594));
#46933=CARTESIAN_POINT('Ctrl Pts',(-0.225275995996774,0.0126688942355271,
0.00904667010172663));
#46934=CARTESIAN_POINT('Ctrl Pts',(-0.225275996142043,0.0126847257901777,
0.00906724967341423));
#46935=CARTESIAN_POINT('Ctrl Pts',(-0.225262378782242,0.0127238511465841,
0.00907909399293944));
#46936=CARTESIAN_POINT('Ctrl Pts',(-0.225248326149835,0.0127563741278717,
0.00907641831404782));
#46937=CARTESIAN_POINT('Ctrl Pts',(-0.225234256379279,0.012788936773166,
0.00907373937198225));
#46938=CARTESIAN_POINT('Ctrl Pts',(-0.225217670901798,0.0128145451972767,
0.00906372431565276));
#46939=CARTESIAN_POINT('Ctrl Pts',(-0.225201030506077,0.0128404758197692,
0.0090447303940509));
#46940=CARTESIAN_POINT('Origin',(-0.225040472131482,0.0123086179887162,
0.00929799673594919));
#46941=CARTESIAN_POINT('Ctrl Pts',(-0.226460323864687,0.0164849848685168,
-0.00182542491256227));
#46942=CARTESIAN_POINT('Ctrl Pts',(-0.226357855404146,0.0164899166391132,
-0.00178775040261278));
#46943=CARTESIAN_POINT('Ctrl Pts',(-0.22636169061375,0.0163828437721616,
-0.00178569503389344));
#46944=CARTESIAN_POINT('Ctrl Pts',(-0.226928626615793,0.0165540683490847,
-0.000945327665866397));
#46945=CARTESIAN_POINT('Ctrl Pts',(-0.226829588972375,0.0165622085538829,
-0.00090622765606428));
#46946=CARTESIAN_POINT('Ctrl Pts',(-0.2268300202053,0.0164544928037623,
-0.000903811545142425));
#46947=CARTESIAN_POINT('Ctrl Pts',(-0.22732376166117,0.0165471381897995,
0.000459404657520975));
#46948=CARTESIAN_POINT('Ctrl Pts',(-0.227219857669224,0.0165519175322698,
0.00049097703221346));
#46949=CARTESIAN_POINT('Ctrl Pts',(-0.22722202781326,0.0164443490933984,
0.00048688368879839));
#46950=CARTESIAN_POINT('Ctrl Pts',(-0.228087003030431,0.0164796571711842,
0.00211169858914439));
#46951=CARTESIAN_POINT('Ctrl Pts',(-0.227992577930613,0.0164840917454652,
0.00216345181702484));
#46952=CARTESIAN_POINT('Ctrl Pts',(-0.227993997265494,0.0163765955727232,
0.00215882659204883));
#46953=CARTESIAN_POINT('Ctrl Pts',(-0.228710023259209,0.0164019593689328,
0.00316442782941463));
#46954=CARTESIAN_POINT('Ctrl Pts',(-0.228619671146624,0.0163991049219305,
0.0032241214340768));
#46955=CARTESIAN_POINT('Ctrl Pts',(-0.228621805321824,0.0162921981879355,
0.00320625921131432));
#46956=CARTESIAN_POINT('Ctrl Pts',(-0.229657567732581,0.0161254558637834,
0.0044874505494743));
#46957=CARTESIAN_POINT('Ctrl Pts',(-0.229574718139383,0.0161107313516101,
0.00455611627440692));
#46958=CARTESIAN_POINT('Ctrl Pts',(-0.229577504909484,0.016007399298503,
0.0045232489857868));
#46959=CARTESIAN_POINT('Ctrl Pts',(-0.230782492911356,0.0157135844815065,
0.00559630641179901));
#46960=CARTESIAN_POINT('Ctrl Pts',(-0.230706701936257,0.0156864648997765,
0.00566911350638642));
#46961=CARTESIAN_POINT('Ctrl Pts',(-0.230709555108569,0.0155883751293595,
0.00562241066007922));
#46962=CARTESIAN_POINT('Ctrl Pts',(-0.231954884548777,0.0151726511086173,
0.00661364144351075));
#46963=CARTESIAN_POINT('Ctrl Pts',(-0.231879927645458,0.0151359104217408,
0.00668269343885589));
#46964=CARTESIAN_POINT('Ctrl Pts',(-0.231883490729645,0.0150444879907642,
0.00662454319409727));
#46965=CARTESIAN_POINT('Ctrl Pts',(-0.232812135329546,0.0146956231411079,
0.00734628897413812));
#46966=CARTESIAN_POINT('Ctrl Pts',(-0.232730280256018,0.0146560965832439,
0.00740574769828582));
#46967=CARTESIAN_POINT('Ctrl Pts',(-0.23273445915703,0.0145703447276702,
0.00733970090416684));
#46968=CARTESIAN_POINT('Ctrl Pts',(-0.233526760469644,0.014056171381814,
0.00814319080840423));
#46969=CARTESIAN_POINT('Ctrl Pts',(-0.233430966824543,0.0140223502084935,
0.00818325695970401));
#46970=CARTESIAN_POINT('Ctrl Pts',(-0.233435828983806,0.0139438644997202,
0.00810904310707394));
#46971=CARTESIAN_POINT('Ctrl Pts',(-0.233963240632296,0.0132087652045752,
0.00896223768026468));
#46972=CARTESIAN_POINT('Ctrl Pts',(-0.233855630854944,0.0131932739624839,
0.00897664245241558));
#46973=CARTESIAN_POINT('Ctrl Pts',(-0.233860658240855,0.0131247144347458,
0.0088934990969508));
#46974=CARTESIAN_POINT('Ctrl Pts',(-0.233990673499441,0.0121849661189448,
0.00969801941997673));
#46975=CARTESIAN_POINT('Ctrl Pts',(-0.233882385854836,0.01219960051827,
0.00969004641588171));
#46976=CARTESIAN_POINT('Ctrl Pts',(-0.233887663559822,0.0121428785160235,
0.00959846506542782));
#46977=CARTESIAN_POINT('Ctrl Pts',(-0.233608550440856,0.0111179473338957,
0.0102465362016285));
#46978=CARTESIAN_POINT('Ctrl Pts',(-0.233510341012519,0.0111613510123303,
0.0102290029036576));
#46979=CARTESIAN_POINT('Ctrl Pts',(-0.233515957859729,0.0111166032784907,
0.0101308151772016));
#46980=CARTESIAN_POINT('Ctrl Pts',(-0.232973388139519,0.010116162533787,
0.0106005529114346));
#46981=CARTESIAN_POINT('Ctrl Pts',(-0.232885165283324,0.0101768275513439,
0.0105844086579605));
#46982=CARTESIAN_POINT('Ctrl Pts',(-0.232890700139198,0.0101433743507589,
0.0104816507674126));
#46983=CARTESIAN_POINT('Ctrl Pts',(-0.23159038031528,0.00836951725233097,
0.0109948951822117));
#46984=CARTESIAN_POINT('Ctrl Pts',(-0.231511257002863,0.00844418452103866,
0.0109893103432351));
#46985=CARTESIAN_POINT('Ctrl Pts',(-0.231517202802167,0.0084315211648833,
0.0108808883898792));
#46986=CARTESIAN_POINT('Ctrl Pts',(-0.230293417632758,0.00705158142584348,
0.0109556442486425));
#46987=CARTESIAN_POINT('Ctrl Pts',(-0.230215203379315,0.00712643592335552,
0.0109628407060781));
#46988=CARTESIAN_POINT('Ctrl Pts',(-0.230220372577151,0.00712874403259708,
0.010854144651623));
#46989=CARTESIAN_POINT('Ctrl Pts',(-0.229386810800953,0.0059251590909317,
0.0107665255249345));
#46990=CARTESIAN_POINT('Ctrl Pts',(-0.229301654948061,0.00599069017573065,
0.0107812705223676));
#46991=CARTESIAN_POINT('Ctrl Pts',(-0.229306186219208,0.00600670522370337,
0.0106743424323745));
#46992=CARTESIAN_POINT('Ctrl Pts',(-0.227105547431042,0.0164416356533416,
-1.96367242225517E-8));
#46993=CARTESIAN_POINT('Ctrl Pts',(-0.227106271411155,0.0164869558406628,
-1.56753936214819E-8));
#46994=CARTESIAN_POINT('Ctrl Pts',(-0.227142754365489,0.0165269328020988,
-7.87961297604824E-8));
#46995=CARTESIAN_POINT('Ctrl Pts',(-0.227186338350779,0.0165370366065652,
1.51447635016797E-7));
#46996=CARTESIAN_POINT('Ctrl Pts',(-0.227195260295749,0.0165391049256242,
1.9858013530413E-7));
#46997=CARTESIAN_POINT('Ctrl Pts',(-0.22720444130248,0.0165400702997432,
2.43952579346465E-7));
#46998=CARTESIAN_POINT('Ctrl Pts',(-0.22721356409307,0.0165399273072623,
2.64138495236366E-7));
#46999=CARTESIAN_POINT('Ctrl Pts',(-0.23059831458869,0.00749150590459184,
0.0108190894733326));
#47000=CARTESIAN_POINT('Ctrl Pts',(-0.230598147360955,0.00749149939828456,
0.0108265200709065));
#47001=CARTESIAN_POINT('Ctrl Pts',(-0.230599102175073,0.00749149541385465,
0.0108338813048351));
#47002=CARTESIAN_POINT('Ctrl Pts',(-0.230603304621065,0.00749149238562031,
0.0108489776967078));
#47003=CARTESIAN_POINT('Ctrl Pts',(-0.230606737271225,0.00749149395180183,
0.0108564893413419));
#47004=CARTESIAN_POINT('Ctrl Pts',(-0.230618362153178,0.00749150550463007,
0.0108749535226858));
#47005=CARTESIAN_POINT('Ctrl Pts',(-0.230628423413568,0.00749152031944393,
0.0108853640995515));
#47006=CARTESIAN_POINT('Ctrl Pts',(-0.23065496699676,0.00749157064776889,
0.0109041826329793));
#47007=CARTESIAN_POINT('Ctrl Pts',(-0.230671138540069,0.00749160344961521,
0.0109114284322365));
#47008=CARTESIAN_POINT('Ctrl Pts',(-0.230694761031536,0.00749168275194574,
0.0109179699756364));
#47009=CARTESIAN_POINT('Ctrl Pts',(-0.230701775839829,0.00749170704004545,
0.0109194442755902));
#47010=CARTESIAN_POINT('Ctrl Pts',(-0.230712384818665,0.00749178450294742,
0.0109210202406609));
#47011=CARTESIAN_POINT('Ctrl Pts',(-0.230715905182152,0.00749181293946376,
0.010921433226754));
#47012=CARTESIAN_POINT('Ctrl Pts',(-0.230721064742677,0.0074919198014703,
0.0109218917459213));
#47013=CARTESIAN_POINT('Ctrl Pts',(-0.230722841815142,0.0074919663207982,
0.0109220228385434));
#47014=CARTESIAN_POINT('Ctrl Pts',(-0.230725231630399,0.00749210732536436,
0.0109221676238527));
#47015=CARTESIAN_POINT('Ctrl Pts',(-0.23072618476541,0.00749217893940242,
0.0109222187380797));
#47016=CARTESIAN_POINT('Ctrl Pts',(-0.230727492126692,0.00749237315537678,
0.0109222792098174));
#47017=CARTESIAN_POINT('Ctrl Pts',(-0.230727934235603,0.00749246408382049,
0.0109222975651963));
#47018=CARTESIAN_POINT('Ctrl Pts',(-0.230728668324687,0.00749269378485217,
0.0109223256573981));
#47019=CARTESIAN_POINT('Ctrl Pts',(-0.230728965398421,0.00749282531917022,
0.0109223358742854));
#47020=CARTESIAN_POINT('Ctrl Pts',(-0.230729583032033,0.00749328310367994,
0.0109223542496217));
#47021=CARTESIAN_POINT('Ctrl Pts',(-0.22939971429741,0.00902231898868095,
0.0107696055271206));
#47022=CARTESIAN_POINT('Ctrl Pts',(-0.229317236826403,0.0089464276852763,
0.0107826523435916));
#47023=CARTESIAN_POINT('Ctrl Pts',(-0.229327136398156,0.00893435685226059,
0.0106710273104172));
#47024=CARTESIAN_POINT('Ctrl Pts',(-0.23028282524575,0.00794079935763272,
0.0109577498892055));
#47025=CARTESIAN_POINT('Ctrl Pts',(-0.230198785803285,0.00786578121681689,
0.010963523886201));
#47026=CARTESIAN_POINT('Ctrl Pts',(-0.230208806930841,0.00786787364958645,
0.0108505771393227));
#47027=CARTESIAN_POINT('Ctrl Pts',(-0.231597063345844,0.00661001185322147,
0.0109902582614569));
#47028=CARTESIAN_POINT('Ctrl Pts',(-0.231516131837863,0.00653048941558155,
0.0109820740545611));
#47029=CARTESIAN_POINT('Ctrl Pts',(-0.231526964171442,0.00654839740201362,
0.0108702093496403));
#47030=CARTESIAN_POINT('Ctrl Pts',(-0.232965808562566,0.00488992308630332,
0.0106020892738249));
#47031=CARTESIAN_POINT('Ctrl Pts',(-0.232873579300101,0.00482771019810843,
0.0105836762826241));
#47032=CARTESIAN_POINT('Ctrl Pts',(-0.232884605773775,0.00486582449374799,
0.0104782074384069));
#47033=CARTESIAN_POINT('Ctrl Pts',(-0.233605220528918,0.0038840291080987,
0.0102473328805686));
#47034=CARTESIAN_POINT('Ctrl Pts',(-0.233503283699538,0.00383871726872211,
0.0102270182108335));
#47035=CARTESIAN_POINT('Ctrl Pts',(-0.233514916837305,0.0038876872738603,
0.0101264028421645));
#47036=CARTESIAN_POINT('Ctrl Pts',(-0.233980537332444,0.00282437387879693,
0.0097033931294933));
#47037=CARTESIAN_POINT('Ctrl Pts',(-0.233867530792116,0.0028108286421166,
0.00969394810388323));
#47038=CARTESIAN_POINT('Ctrl Pts',(-0.233879460305132,0.00287024877252639,
0.009599479752749));
#47039=CARTESIAN_POINT('Ctrl Pts',(-0.23395842524631,0.00179682516051009,
0.00896703580133416));
#47040=CARTESIAN_POINT('Ctrl Pts',(-0.233846367591842,0.00181382176323882,
0.00898039582417626));
#47041=CARTESIAN_POINT('Ctrl Pts',(-0.233857974495682,0.00188386343549592,
0.00889339615048512));
#47042=CARTESIAN_POINT('Ctrl Pts',(-0.233525319503738,0.000950916333047615,
0.00815049547091419));
#47043=CARTESIAN_POINT('Ctrl Pts',(-0.233425241575143,0.000987309445839432,
0.00819063695809306));
#47044=CARTESIAN_POINT('Ctrl Pts',(-0.233436000330147,0.00106648365210777,
0.00811134827503141));
#47045=CARTESIAN_POINT('Ctrl Pts',(-0.232815357496005,0.000312535379510872,
0.00735780536508385));
#47046=CARTESIAN_POINT('Ctrl Pts',(-0.232729912996603,0.000355240759461433,
0.00741848169680565));
#47047=CARTESIAN_POINT('Ctrl Pts',(-0.232739152296681,0.000441578432710503,
0.00734645441856656));
#47048=CARTESIAN_POINT('Ctrl Pts',(-0.231951736654993,-0.000171158652928347,
0.0066165523630098));
#47049=CARTESIAN_POINT('Ctrl Pts',(-0.23187366145612,-0.000131220286198218,
0.00668759534496474));
#47050=CARTESIAN_POINT('Ctrl Pts',(-0.231881821261106,-3.87834252174242E-5,
0.00662323404316121));
#47051=CARTESIAN_POINT('Ctrl Pts',(-0.230785589044538,-0.000709423264214162,
0.00560435737523353));
#47052=CARTESIAN_POINT('Ctrl Pts',(-0.230706537242168,-0.000679412943678259,
0.0056793959267812));
#47053=CARTESIAN_POINT('Ctrl Pts',(-0.230714035519574,-0.00057952778959745,
0.00562665136337194));
#47054=CARTESIAN_POINT('Ctrl Pts',(-0.229659631065858,-0.00112259134770437,
0.00450042681701567));
#47055=CARTESIAN_POINT('Ctrl Pts',(-0.229573488553691,-0.00110522274085626,
0.00457169571489191));
#47056=CARTESIAN_POINT('Ctrl Pts',(-0.229581284792486,-0.000999176418349601,
0.00453324254178003));
#47057=CARTESIAN_POINT('Ctrl Pts',(-0.228704830832439,-0.00140318368076378,
0.00315941395843816));
#47058=CARTESIAN_POINT('Ctrl Pts',(-0.228610654986378,-0.00139852405540933,
0.00322143708123328));
#47059=CARTESIAN_POINT('Ctrl Pts',(-0.228618237517232,-0.0012879748082025,
0.00319964145512532));
#47060=CARTESIAN_POINT('Ctrl Pts',(-0.227556561243924,-0.00154241565951436,
0.0012329595537125));
#47061=CARTESIAN_POINT('Ctrl Pts',(-0.227456077166232,-0.00155052303720059,
0.00128236480914283));
#47062=CARTESIAN_POINT('Ctrl Pts',(-0.227460355524764,-0.0014385066227586,
0.00128071762255347));
#47063=CARTESIAN_POINT('Ctrl Pts',(-0.227067475401737,-0.00156364911782018,
-0.000543776460822949));
#47064=CARTESIAN_POINT('Ctrl Pts',(-0.226954628187393,-0.00156468311793233,
-0.000524073299869157));
#47065=CARTESIAN_POINT('Ctrl Pts',(-0.226966244999462,-0.00145297979334359,
-0.000526745240384302));
#47066=CARTESIAN_POINT('Ctrl Pts',(-0.226499467790203,-0.00150465501127181,
-0.00186941076976256));
#47067=CARTESIAN_POINT('Ctrl Pts',(-0.226406444017648,-0.00151556901664699,
-0.00180216089269515));
#47068=CARTESIAN_POINT('Ctrl Pts',(-0.226407377277794,-0.00140350174937455,
-0.001803497060247));
#47069=CARTESIAN_POINT('Ctrl Pts',(-0.227106039951076,-0.00144162797772285,
-1.96352411817887E-8));
#47070=CARTESIAN_POINT('Ctrl Pts',(-0.227106764003939,-0.00148696123572356,
-1.58531560466822E-8));
#47071=CARTESIAN_POINT('Ctrl Pts',(-0.227143294427859,-0.00152691654689948,
-1.05861461769103E-7));
#47072=CARTESIAN_POINT('Ctrl Pts',(-0.22718689352733,-0.00153702230304076,
8.6620036555294E-8));
#47073=CARTESIAN_POINT('Ctrl Pts',(-0.227195833594342,-0.00153909450494876,
1.26088684176056E-7));
#47074=CARTESIAN_POINT('Ctrl Pts',(-0.227205033194746,-0.00154006152936436,
1.63587269727728E-7));
#47075=CARTESIAN_POINT('Ctrl Pts',(-0.227214174219929,-0.00153991824305303,
1.76093623814383E-7));
#47076=CARTESIAN_POINT('Ctrl Pts',(-0.226392113206532,0.0163918999727596,
0.00168503949271779));
#47077=CARTESIAN_POINT('Ctrl Pts',(-0.226391019396591,0.0164937656877913,
0.00168965763500863));
#47078=CARTESIAN_POINT('Ctrl Pts',(-0.226488180900027,0.0164909418855625,
0.00172671497106663));
#47079=CARTESIAN_POINT('Ctrl Pts',(-0.226852777892721,0.0164582707631305,
0.000831312067351));
#47080=CARTESIAN_POINT('Ctrl Pts',(-0.226855540364924,0.0165604646886994,
0.00083395588090366));
#47081=CARTESIAN_POINT('Ctrl Pts',(-0.226949543911946,0.0165548900333955,
0.00087119979331494));
#47082=CARTESIAN_POINT('Ctrl Pts',(-0.227237968586075,0.0164450763319647,
-0.000539645166208353));
#47083=CARTESIAN_POINT('Ctrl Pts',(-0.227238798227237,0.0165473213837703,
-0.000542455601089969));
#47084=CARTESIAN_POINT('Ctrl Pts',(-0.227337590667714,0.0165449321176619,
-0.000511810717256663));
#47085=CARTESIAN_POINT('Ctrl Pts',(-0.228035000539669,0.0163790222318258,
-0.00217959547214826));
#47086=CARTESIAN_POINT('Ctrl Pts',(-0.228036534639494,0.016481137218235,
-0.00218239346647812));
#47087=CARTESIAN_POINT('Ctrl Pts',(-0.22812497432452,0.0164790173149829,
-0.00213090379182275));
#47088=CARTESIAN_POINT('Ctrl Pts',(-0.228708921333346,0.0162902569986761,
-0.00323431581776797));
#47089=CARTESIAN_POINT('Ctrl Pts',(-0.22870963661687,0.0163920559157401,
-0.00325001291976414));
#47090=CARTESIAN_POINT('Ctrl Pts',(-0.228793564308444,0.0163974242481985,
-0.00319058715685894));
#47091=CARTESIAN_POINT('Ctrl Pts',(-0.229730987265362,0.0160079041094603,
-0.00452203445052858));
#47092=CARTESIAN_POINT('Ctrl Pts',(-0.229730769949974,0.01610670436963,
-0.00455111205785709));
#47093=CARTESIAN_POINT('Ctrl Pts',(-0.229805911713532,0.0161237707411685,
-0.00448235671725372));
#47094=CARTESIAN_POINT('Ctrl Pts',(-0.230935134430229,0.0156120089346621,
-0.00557070752495235));
#47095=CARTESIAN_POINT('Ctrl Pts',(-0.230934670361149,0.0157064984816925,
-0.00561229511004819));
#47096=CARTESIAN_POINT('Ctrl Pts',(-0.231002371233807,0.0157353050227464,
-0.00554004179593496));
#47097=CARTESIAN_POINT('Ctrl Pts',(-0.232177744180245,0.0151028200699603,
-0.00653547490843776));
#47098=CARTESIAN_POINT('Ctrl Pts',(-0.232176588665142,0.0151916192466989,
-0.00658760783579178));
#47099=CARTESIAN_POINT('Ctrl Pts',(-0.232244981206936,0.0152287657678068,
-0.00652027966165211));
#47100=CARTESIAN_POINT('Ctrl Pts',(-0.233054633763043,0.0146485714867585,
-0.00724293745904123));
#47101=CARTESIAN_POINT('Ctrl Pts',(-0.233053075526623,0.0147322907208735,
-0.00730274052660402));
#47102=CARTESIAN_POINT('Ctrl Pts',(-0.233129281923515,0.0147718879604937,
-0.00724522074812763));
#47103=CARTESIAN_POINT('Ctrl Pts',(-0.233780549323432,0.0140296693618124,
-0.00802833810437384));
#47104=CARTESIAN_POINT('Ctrl Pts',(-0.233778793651804,0.0141064055513379,
-0.00809659254281335));
#47105=CARTESIAN_POINT('Ctrl Pts',(-0.233870885754837,0.0141387792230417,
-0.00806053199685345));
#47106=CARTESIAN_POINT('Ctrl Pts',(-0.23417681319712,0.0131895359915029,
-0.00885217079243862));
#47107=CARTESIAN_POINT('Ctrl Pts',(-0.234175306972833,0.0132559030196369,
-0.00893028824280225));
#47108=CARTESIAN_POINT('Ctrl Pts',(-0.234278422455447,0.0132689423938031,
-0.00892070199865507));
#47109=CARTESIAN_POINT('Ctrl Pts',(-0.234152670783076,0.0121914679424191,
-0.00957792241659341));
#47110=CARTESIAN_POINT('Ctrl Pts',(-0.23415083916279,0.0122454565740586,
-0.00966504377078786));
#47111=CARTESIAN_POINT('Ctrl Pts',(-0.23425279196153,0.0122284519300089,
-0.00967704060679076));
#47112=CARTESIAN_POINT('Ctrl Pts',(-0.233726044807365,0.0111642828582113,
-0.0101174976232404));
#47113=CARTESIAN_POINT('Ctrl Pts',(-0.233723596210825,0.0112061357531395,
-0.0102112243167655));
#47114=CARTESIAN_POINT('Ctrl Pts',(-0.233815358570609,0.0111632233286248,
-0.0102310405426672));
#47115=CARTESIAN_POINT('Ctrl Pts',(-0.233061858989254,0.0101827622716988,
-0.0104764728820601));
#47116=CARTESIAN_POINT('Ctrl Pts',(-0.233059226207355,0.0102132546913798,
-0.0105746029191505));
#47117=CARTESIAN_POINT('Ctrl Pts',(-0.23314194681633,0.0101548706247753,
-0.0105925793018587));
#47118=CARTESIAN_POINT('Ctrl Pts',(-0.231683602236085,0.00851585290564029,
-0.0108729492449486));
#47119=CARTESIAN_POINT('Ctrl Pts',(-0.231680434000005,0.00852679029691534,
-0.0109760864334407));
#47120=CARTESIAN_POINT('Ctrl Pts',(-0.231755479841859,0.0084561911036003,
-0.0109838889155731));
#47121=CARTESIAN_POINT('Ctrl Pts',(-0.230418420088248,0.00719112093427334,
-0.0108666061778807));
#47122=CARTESIAN_POINT('Ctrl Pts',(-0.230415842999401,0.00718736729446149,
-0.0109698519447955));
#47123=CARTESIAN_POINT('Ctrl Pts',(-0.230492085334579,0.00711822388992815,
-0.0109659055259879));
#47124=CARTESIAN_POINT('Ctrl Pts',(-0.229525698879995,0.00614771790123177,
-0.0106946346144635));
#47125=CARTESIAN_POINT('Ctrl Pts',(-0.22952334834197,0.00613160474304804,
-0.0107960792076886));
#47126=CARTESIAN_POINT('Ctrl Pts',(-0.229599955864645,0.00606416878077252,
-0.0107848368047938));
#47127=CARTESIAN_POINT('Ctrl Pts',(-0.230713742406189,0.00748906369436089,
-0.010821683971079));
#47128=CARTESIAN_POINT('Ctrl Pts',(-0.230713574584272,0.00748905436859433,
-0.0108291148800308));
#47129=CARTESIAN_POINT('Ctrl Pts',(-0.230714527471167,0.00748904745953601,
-0.0108364768338736));
#47130=CARTESIAN_POINT('Ctrl Pts',(-0.23071872359061,0.00748903792811973,
-0.0108515735632303));
#47131=CARTESIAN_POINT('Ctrl Pts',(-0.230722151247374,0.0074890359577174,
-0.0108590855100948));
#47132=CARTESIAN_POINT('Ctrl Pts',(-0.23073376178249,0.00748903765108982,
-0.0108775512731657));
#47133=CARTESIAN_POINT('Ctrl Pts',(-0.230743810553506,0.0074890458653673,
-0.0108879615646477));
#47134=CARTESIAN_POINT('Ctrl Pts',(-0.230770302348385,0.00748907690128229,
-0.0109067656321191));
#47135=CARTESIAN_POINT('Ctrl Pts',(-0.230786433005652,0.00748910168902196,
-0.0109140058410522));
#47136=CARTESIAN_POINT('Ctrl Pts',(-0.230810323644408,0.00748913267026307,
-0.0109206355722776));
#47137=CARTESIAN_POINT('Ctrl Pts',(-0.230817653411284,0.00748914304852623,
-0.0109221578060995));
#47138=CARTESIAN_POINT('Ctrl Pts',(-0.230828641240643,0.00748914067964123,
-0.0109237318478977));
#47139=CARTESIAN_POINT('Ctrl Pts',(-0.23083224030065,0.00748914000390417,
-0.0109241347209408));
#47140=CARTESIAN_POINT('Ctrl Pts',(-0.230837645742019,0.00748910265615934,
-0.010924578658873));
#47141=CARTESIAN_POINT('Ctrl Pts',(-0.230839444858523,0.0074890863471106,
-0.0109246969586367));
#47142=CARTESIAN_POINT('Ctrl Pts',(-0.23084194199522,0.00748900478020963,
-0.0109248290895748));
#47143=CARTESIAN_POINT('Ctrl Pts',(-0.230842846341935,0.00748896132912684,
-0.0109248694996749));
#47144=CARTESIAN_POINT('Ctrl Pts',(-0.230844078640512,0.00748881721420382,
-0.0109249173915236));
#47145=CARTESIAN_POINT('Ctrl Pts',(-0.230844469751936,0.00748873856186406,
-0.0109249304395881));
#47146=CARTESIAN_POINT('Ctrl Pts',(-0.230845032959145,0.00748854352309953,
-0.0109249479600377));
#47147=CARTESIAN_POINT('Ctrl Pts',(-0.230845459445073,0.00748823871023351,
-0.0109249589743604));
#47148=CARTESIAN_POINT('Ctrl Pts',(-0.226417776006695,-0.00148225140227062,
0.00185960662666182));
#47149=CARTESIAN_POINT('Ctrl Pts',(-0.226315901794499,-0.00148400327446099,
0.0018271058249673));
#47150=CARTESIAN_POINT('Ctrl Pts',(-0.226321596488582,-0.00138004225740634,
0.00182063316556843));
#47151=CARTESIAN_POINT('Ctrl Pts',(-0.226922704220666,-0.00155536550330681,
0.000950761709448938));
#47152=CARTESIAN_POINT('Ctrl Pts',(-0.226827971984197,-0.00156047124551848,
0.000910041917077747));
#47153=CARTESIAN_POINT('Ctrl Pts',(-0.226827215374829,-0.00145621045917323,
0.000908994318720162));
#47154=CARTESIAN_POINT('Ctrl Pts',(-0.22731937189759,-0.00154668628306353,
-0.000461986142874138));
#47155=CARTESIAN_POINT('Ctrl Pts',(-0.227217889493944,-0.00154838350965434,
-0.000491876202524546));
#47156=CARTESIAN_POINT('Ctrl Pts',(-0.227220115021664,-0.0014440291172182,
-0.000488620476369189));
#47157=CARTESIAN_POINT('Ctrl Pts',(-0.228125390529573,-0.00147896673645822,
-0.00213882311461267));
#47158=CARTESIAN_POINT('Ctrl Pts',(-0.228035127544321,-0.00148038441206057,
-0.00219126104933539));
#47159=CARTESIAN_POINT('Ctrl Pts',(-0.228035985439426,-0.00137628011913535,
-0.0021870094782073));
#47160=CARTESIAN_POINT('Ctrl Pts',(-0.228800442741132,-0.00139591234854455,
-0.00319848657186414));
#47161=CARTESIAN_POINT('Ctrl Pts',(-0.228714988735678,-0.00138956022407906,
-0.00325932429238547));
#47162=CARTESIAN_POINT('Ctrl Pts',(-0.228716584232433,-0.00128596080771844,
-0.00324145656436105));
#47163=CARTESIAN_POINT('Ctrl Pts',(-0.229802414559229,-0.00112488746796975,
-0.00447866062824715));
#47164=CARTESIAN_POINT('Ctrl Pts',(-0.22972550890945,-0.00110682459306145,
-0.00454832175455453));
#47165=CARTESIAN_POINT('Ctrl Pts',(-0.229727909135064,-0.0010065759274476,
-0.00451693236917198));
#47166=CARTESIAN_POINT('Ctrl Pts',(-0.23102492508135,-0.000727133402331402,
-0.00555987995846644));
#47167=CARTESIAN_POINT('Ctrl Pts',(-0.230955989651605,-0.000696808628886392,
-0.00563338908879835));
#47168=CARTESIAN_POINT('Ctrl Pts',(-0.230958341272015,-0.000601417291620782,
-0.00558870908358806));
#47169=CARTESIAN_POINT('Ctrl Pts',(-0.2322669550296,-0.000219169508655132,
-0.00653742651569375));
#47170=CARTESIAN_POINT('Ctrl Pts',(-0.232197149845059,-0.000180431312386987,
-0.00660566366607625));
#47171=CARTESIAN_POINT('Ctrl Pts',(-0.232200275963735,-9.10743939232668E-5,
-0.00655046594115202));
#47172=CARTESIAN_POINT('Ctrl Pts',(-0.233168284464011,0.000250847815714136,
-0.00727854722407495));
#47173=CARTESIAN_POINT('Ctrl Pts',(-0.233089769094286,0.00029173553377382,
-0.00733597722321239));
#47174=CARTESIAN_POINT('Ctrl Pts',(-0.233093540799596,0.000375715453733222,
-0.00727309367766053));
#47175=CARTESIAN_POINT('Ctrl Pts',(-0.233887901163237,0.00088893249295194,
-0.00809090747094352));
#47176=CARTESIAN_POINT('Ctrl Pts',(-0.233793447168666,0.000921951025758477,
-0.00812622297247575));
#47177=CARTESIAN_POINT('Ctrl Pts',(-0.233797813695556,0.000998937702461697,
-0.00805531832094409));
#47178=CARTESIAN_POINT('Ctrl Pts',(-0.2342833231198,0.00175231486175419,
-0.00893805236514278));
#47179=CARTESIAN_POINT('Ctrl Pts',(-0.234178058148385,0.00176584924761954,
-0.00894697349444574));
#47180=CARTESIAN_POINT('Ctrl Pts',(-0.234182479893669,0.00183287667611329,
-0.00886686230220629));
#47181=CARTESIAN_POINT('Ctrl Pts',(-0.234239736026175,0.00278957126582501,
-0.00968761331434967));
#47182=CARTESIAN_POINT('Ctrl Pts',(-0.234135862048126,0.0027716261589432,
-0.0096741294278813));
#47183=CARTESIAN_POINT('Ctrl Pts',(-0.234140599754382,0.00282694337281929,
-0.00958554148882367));
#47184=CARTESIAN_POINT('Ctrl Pts',(-0.233800163603698,0.00384612493495253,
-0.0102343465381826));
#47185=CARTESIAN_POINT('Ctrl Pts',(-0.233707082011014,0.00380181276785467,
-0.010213200060769));
#47186=CARTESIAN_POINT('Ctrl Pts',(-0.233712136747671,0.00384561342082835,
-0.010118178596806));
#47187=CARTESIAN_POINT('Ctrl Pts',(-0.233127412811296,0.0048454443045241,
-0.0105921689340489));
#47188=CARTESIAN_POINT('Ctrl Pts',(-0.233042619310187,0.00478663294724717,
-0.0105732614730382));
#47189=CARTESIAN_POINT('Ctrl Pts',(-0.233047623062891,0.00481933284931598,
-0.0104737473815675));
#47190=CARTESIAN_POINT('Ctrl Pts',(-0.23171980787036,0.00658675750707835,
-0.0109937670799221));
#47191=CARTESIAN_POINT('Ctrl Pts',(-0.231644109187706,0.00651358566164336,
-0.0109850576705971));
#47192=CARTESIAN_POINT('Ctrl Pts',(-0.231649556960457,0.00652610632374098,
-0.0108799788430654));
#47193=CARTESIAN_POINT('Ctrl Pts',(-0.230396057458204,0.00794487415788723,
-0.0109626141392042));
#47194=CARTESIAN_POINT('Ctrl Pts',(-0.230317899932501,0.00787480750145839,
-0.0109666566144382));
#47195=CARTESIAN_POINT('Ctrl Pts',(-0.230322554500073,0.00787234081934371,
-0.0108613201128976));
#47196=CARTESIAN_POINT('Ctrl Pts',(-0.229489510910491,0.00904713179573227,
-0.0107675268815905));
#47197=CARTESIAN_POINT('Ctrl Pts',(-0.229412653084916,0.00897672311594609,
-0.0107789166455273));
#47198=CARTESIAN_POINT('Ctrl Pts',(-0.229417095976447,0.00896089386946676,
-0.010675313992194));
#47199=CARTESIAN_POINT('',(0.,0.,0.));
#47200=CARTESIAN_POINT('Ctrl Pts',(-0.00380975858063242,-0.00881478413029403,
-0.00183246684420301));
#47201=CARTESIAN_POINT('Ctrl Pts',(-0.00390993294014545,-0.00881478413029403,
-0.00183246684420301));
#47202=CARTESIAN_POINT('Ctrl Pts',(-0.00390975842889103,-0.00882512165273333,
-0.00173282745701358));
#47203=CARTESIAN_POINT('Ctrl Pts',(-0.00380975858063242,-0.00929465142715738,
-0.0018806998537358));
#47204=CARTESIAN_POINT('Ctrl Pts',(-0.00390993294014545,-0.00929465142715738,
-0.0018806998537358));
#47205=CARTESIAN_POINT('Ctrl Pts',(-0.00390975842889103,-0.00927906675289324,
-0.00177836203380147));
#47206=CARTESIAN_POINT('Ctrl Pts',(-0.00380975858063242,-0.0102936387094841,
-0.00158253456509613));
#47207=CARTESIAN_POINT('Ctrl Pts',(-0.00390993294014546,-0.0102936387094841,
-0.00158253456509614));
#47208=CARTESIAN_POINT('Ctrl Pts',(-0.00390975842889104,-0.0102241270617854,
-0.00149607241763065));
#47209=CARTESIAN_POINT('Ctrl Pts',(-0.00380975858063242,-0.0110403459009329,
-0.000207601983482724));
#47210=CARTESIAN_POINT('Ctrl Pts',(-0.00390993294014544,-0.0110403459009329,
-0.000207601983482722));
#47211=CARTESIAN_POINT('Ctrl Pts',(-0.00390975842889102,-0.0109298209858678,
-0.00019577210929604));
#47212=CARTESIAN_POINT('Ctrl Pts',(-0.00380975858063243,-0.010585488822892,
0.00129440175744357));
#47213=CARTESIAN_POINT('Ctrl Pts',(-0.00390993294014546,-0.010585488822892,
0.00129440175744357));
#47214=CARTESIAN_POINT('Ctrl Pts',(-0.00390975842889104,-0.0104994209642949,
0.0012241417666484));
#47215=CARTESIAN_POINT('Ctrl Pts',(-0.00380975858063242,-0.00920314460986179,
0.00202990873817867));
#47216=CARTESIAN_POINT('Ctrl Pts',(-0.00390993294014544,-0.00920314460986179,
0.00202990873817867));
#47217=CARTESIAN_POINT('Ctrl Pts',(-0.00390975842889102,-0.00919187984963056,
0.00191958960744435));
#47218=CARTESIAN_POINT('Ctrl Pts',(-0.00380975858063242,-0.00770446035061261,
0.0015817160659287));
#47219=CARTESIAN_POINT('Ctrl Pts',(-0.00390993294014545,-0.00770446035061261,
0.0015817160659287));
#47220=CARTESIAN_POINT('Ctrl Pts',(-0.00390975842889103,-0.00777409310458325,
0.00149536140507255));
#47221=CARTESIAN_POINT('Ctrl Pts',(-0.00380975858063242,-0.00695993177951074,
0.000203870131802003));
#47222=CARTESIAN_POINT('Ctrl Pts',(-0.00390993294014545,-0.00695993177951073,
0.000203870131802006));
#47223=CARTESIAN_POINT('Ctrl Pts',(-0.00390975842889103,-0.00707045087524681,
0.000192132115288156));
#47224=CARTESIAN_POINT('Ctrl Pts',(-0.00380975858063242,-0.00741443492830406,
-0.00129313650789938));
#47225=CARTESIAN_POINT('Ctrl Pts',(-0.00390993294014545,-0.00741443492830407,
-0.00129313650789939));
#47226=CARTESIAN_POINT('Ctrl Pts',(-0.00390975842889103,-0.00750045646082591,
-0.00122286495690331));
#47227=CARTESIAN_POINT('Ctrl Pts',(-0.00380975858063242,-0.00833491683343068,
-0.00178423383467021));
#47228=CARTESIAN_POINT('Ctrl Pts',(-0.00390993294014545,-0.00833491683343068,
-0.00178423383467021));
#47229=CARTESIAN_POINT('Ctrl Pts',(-0.00390975842889103,-0.00837117655257341,
-0.00168729288022569));
#47230=CARTESIAN_POINT('Ctrl Pts',(-0.00380975858063242,-0.00881478413029403,
-0.00183246684420301));
#47231=CARTESIAN_POINT('Ctrl Pts',(-0.00390993294014545,-0.00881478413029403,
-0.00183246684420301));
#47232=CARTESIAN_POINT('Ctrl Pts',(-0.00390975842889103,-0.00882512165273333,
-0.00173282745701358));
#47233=CARTESIAN_POINT('',(-0.00390975858063242,-0.00882510339125232,-0.00173300347273605));
#47234=CARTESIAN_POINT('',(-0.00380975858063243,-0.00881478413029403,-0.00183246684420301));
#47235=CARTESIAN_POINT('Ctrl Pts',(-0.00390975857180975,-0.00882509934044699,
-0.00173304251652624));
#47236=CARTESIAN_POINT('Ctrl Pts',(-0.0039097165831011,-0.00881478413029403,
-0.00183246684420301));
#47237=CARTESIAN_POINT('Ctrl Pts',(-0.00380975858063242,-0.00881478413029403,
-0.00183246684420301));
#47238=CARTESIAN_POINT('',(-0.00390975858063242,-0.00900031988990579,-0.00174210523730213));
#47239=CARTESIAN_POINT('Ctrl Pts',(-0.00390975858063242,-0.0090003198899058,
-0.00174210523730213));
#47240=CARTESIAN_POINT('Ctrl Pts',(-0.00390975858063242,-0.00945687992322838,
-0.00174202447630927));
#47241=CARTESIAN_POINT('Ctrl Pts',(-0.00390975858063242,-0.0103697614232141,
-0.00136637602002286));
#47242=CARTESIAN_POINT('Ctrl Pts',(-0.00390975858063242,-0.0109405594065751,
-2.90486592512132E-7));
#47243=CARTESIAN_POINT('Ctrl Pts',(-0.00390975858063242,-0.0103680426596137,
0.00136935520820644));
#47244=CARTESIAN_POINT('Ctrl Pts',(-0.00390975858063243,-0.00899628845176151,
0.00192951445904318));
#47245=CARTESIAN_POINT('Ctrl Pts',(-0.00390975858063241,-0.00762974915067706,
0.00136520476073566));
#47246=CARTESIAN_POINT('Ctrl Pts',(-0.00390975858063243,-0.00706013247825494,
8.11459216446678E-7));
#47247=CARTESIAN_POINT('Ctrl Pts',(-0.00390975858063242,-0.00760544730692673,
-0.00130817127168898));
#47248=CARTESIAN_POINT('Ctrl Pts',(-0.00390975858063242,-0.00842870221548062,
-0.00169187672673672));
#47249=CARTESIAN_POINT('Ctrl Pts',(-0.00390975858063242,-0.00882510339125232,
-0.00173300347273605));
#47250=CARTESIAN_POINT('',(-0.00380975858063243,-0.00899998937218426,-0.00184137848958098));
#47251=CARTESIAN_POINT('Ctrl Pts',(-0.00390975606002064,-0.00900031988985028,
-0.00174210521939449));
#47252=CARTESIAN_POINT('Ctrl Pts',(-0.00390905107214187,-0.00899998937218426,
-0.00184137848958098));
#47253=CARTESIAN_POINT('Ctrl Pts',(-0.00380975858063242,-0.00899998937218426,
-0.00184137848958098));
#47254=CARTESIAN_POINT('',(-0.00380975858063243,-0.00900001212691424,0.00184141020097112));
#47255=CARTESIAN_POINT('Ctrl Pts',(-0.00380975858063243,-0.00900001212691424,
0.00184141020097112));
#47256=CARTESIAN_POINT('Ctrl Pts',(-0.00380975858063243,-0.00906142348782768,
0.00184161153465334));
#47257=CARTESIAN_POINT('Ctrl Pts',(-0.00380975858063243,-0.00912270322366649,
0.00183871389074159));
#47258=CARTESIAN_POINT('Ctrl Pts',(-0.00380975858063243,-0.00918375460215863,
0.00183262546268116));
#47259=CARTESIAN_POINT('Ctrl Pts',(-0.00380975858063243,-0.00966332758164447,
0.00178479942406512));
#47260=CARTESIAN_POINT('Ctrl Pts',(-0.00380975858063243,-0.0101244136873442,
0.00153992848358091));
#47261=CARTESIAN_POINT('Ctrl Pts',(-0.00380975858063243,-0.0104309076337271,
0.0011666522974117));
#47262=CARTESIAN_POINT('Ctrl Pts',(-0.00380975858063243,-0.0107366396990011,
0.000794303999306896));
#47263=CARTESIAN_POINT('Ctrl Pts',(-0.00380975858063243,-0.0108887999330076,
0.000293786106230727));
#47264=CARTESIAN_POINT('Ctrl Pts',(-0.00380975858063243,-0.0108400851893513,
-0.000186423456930577));
#47265=CARTESIAN_POINT('Ctrl Pts',(-0.00380975858063243,-0.0107914327883849,
-0.000666018471935143));
#47266=CARTESIAN_POINT('Ctrl Pts',(-0.00380975858063243,-0.0105418163288552,
-0.00112481192963245));
#47267=CARTESIAN_POINT('Ctrl Pts',(-0.00380975858063243,-0.0101683430874772,
-0.00142792045698715));
#47268=CARTESIAN_POINT('Ctrl Pts',(-0.00380975858063243,-0.00984183803121622,
-0.00169290990151061));
#47269=CARTESIAN_POINT('Ctrl Pts',(-0.00380975858063243,-0.00941977782130047,
-0.00183994022345956));
#47270=CARTESIAN_POINT('Ctrl Pts',(-0.00380975858063243,-0.00899998937218426,
-0.00184137848958098));
#47271=CARTESIAN_POINT('Ctrl Pts',(-0.00380975858063243,-0.00881478413029403,
-0.00183246684420301));
#47272=CARTESIAN_POINT('Ctrl Pts',(-0.00380975858063243,-0.00833564521297648,
-0.00178430704644731));
#47273=CARTESIAN_POINT('Ctrl Pts',(-0.00380975858063243,-0.00787521215159384,
-0.00153933786611053));
#47274=CARTESIAN_POINT('Ctrl Pts',(-0.00380975858063243,-0.00756880487978684,
-0.0011664097329752));
#47275=CARTESIAN_POINT('Ctrl Pts',(-0.00380975858063243,-0.00726345873171947,
-0.000794773092998356));
#47276=CARTESIAN_POINT('Ctrl Pts',(-0.00380975858063243,-0.00711142381370158,
-0.000295221445893798));
#47277=CARTESIAN_POINT('Ctrl Pts',(-0.00380975858063243,-0.00715977039949327,
0.000184010014206217));
#47278=CARTESIAN_POINT('Ctrl Pts',(-0.00380975858063243,-0.00720817502841981,
0.000663816821992245));
#47279=CARTESIAN_POINT('Ctrl Pts',(-0.00380975858063243,-0.00745702122447455,
0.0011230340789884));
#47280=CARTESIAN_POINT('Ctrl Pts',(-0.00380975858063243,-0.00783015296530383,
0.00142677385561591));
#47281=CARTESIAN_POINT('Ctrl Pts',(-0.00380975858063243,-0.00815677065544411,
0.00169264988113258));
#47282=CARTESIAN_POINT('Ctrl Pts',(-0.00380975858063243,-0.00857913028022675,
0.00184003036358083));
#47283=CARTESIAN_POINT('Ctrl Pts',(-0.00380975858063243,-0.00900001212691424,
0.00184141020097112));
#47284=CARTESIAN_POINT('Ctrl Pts',(-0.0035392791351489,-0.00858849912814965,
-0.00179466521288696));
#47285=CARTESIAN_POINT('Ctrl Pts',(-0.00342573153923465,-0.00859176400850957,
-0.00179333404984997));
#47286=CARTESIAN_POINT('Ctrl Pts',(-0.00343811948343117,-0.00856602524158671,
-0.00190328650635992));
#47287=CARTESIAN_POINT('Ctrl Pts',(-0.00355142559943888,-0.00905859136078448,
-0.00190144952999438));
#47288=CARTESIAN_POINT('Ctrl Pts',(-0.00343722171108695,-0.00906840205799737,
-0.00190374929419889));
#47289=CARTESIAN_POINT('Ctrl Pts',(-0.0034503400565124,-0.00906157284819796,
-0.0020166590821151));
#47290=CARTESIAN_POINT('Ctrl Pts',(-0.00352537010396588,-0.0100884377158575,
-0.00172789987787408));
#47291=CARTESIAN_POINT('Ctrl Pts',(-0.0034151603753512,-0.0100497091309754,
-0.00174559426658833));
#47292=CARTESIAN_POINT('Ctrl Pts',(-0.00342416641781692,-0.0101460057925454,
-0.00183316467220812));
#47293=CARTESIAN_POINT('Ctrl Pts',(-0.00341335748290235,-0.0109970962519671,
-0.000457281663563109));
#47294=CARTESIAN_POINT('Ctrl Pts',(-0.00331425963473675,-0.010996887331939,
-0.000476856829642387));
#47295=CARTESIAN_POINT('Ctrl Pts',(-0.0033115684832145,-0.0111050748119872,
-0.000486036946141634));
#47296=CARTESIAN_POINT('Ctrl Pts',(-0.00345233946123927,-0.0107338060170907,
0.00108652455487473));
#47297=CARTESIAN_POINT('Ctrl Pts',(-0.00335032457735252,-0.0107129565277369,
0.00112100474052161));
#47298=CARTESIAN_POINT('Ctrl Pts',(-0.00335076613415529,-0.0108274712600009,
0.00115282043607336));
#47299=CARTESIAN_POINT('Ctrl Pts',(-0.00356449374860163,-0.00945621932640169,
0.00198829625682747));
#47300=CARTESIAN_POINT('Ctrl Pts',(-0.00344854884364189,-0.00943365667565594,
0.00198475236629158));
#47301=CARTESIAN_POINT('Ctrl Pts',(-0.0034634722557383,-0.00948068538942303,
0.00210854197031486));
#47302=CARTESIAN_POINT('Ctrl Pts',(-0.00352531374816938,-0.00791032423527775,
0.00172792526671951));
#47303=CARTESIAN_POINT('Ctrl Pts',(-0.00341511348123987,-0.00794907951679388,
0.00174568140804206));
#47304=CARTESIAN_POINT('Ctrl Pts',(-0.00342410980697788,-0.0078526998577211,
0.00183315731298699));
#47305=CARTESIAN_POINT('Ctrl Pts',(-0.00341328178572483,-0.00700287546046352,
0.000454633913679566));
#47306=CARTESIAN_POINT('Ctrl Pts',(-0.00331419107940177,-0.00700305969526376,
0.000474177195847323));
#47307=CARTESIAN_POINT('Ctrl Pts',(-0.00331149240063511,-0.00689487285927746,
0.000483300740605997));
#47308=CARTESIAN_POINT('Ctrl Pts',(-0.00345241595160808,-0.00726632486312327,
-0.00108656836792835));
#47309=CARTESIAN_POINT('Ctrl Pts',(-0.00335038976344317,-0.00728717254733531,
-0.00112102914438496));
#47310=CARTESIAN_POINT('Ctrl Pts',(-0.00335084297932956,-0.00717272015287796,
-0.00115292921767708));
#47311=CARTESIAN_POINT('Ctrl Pts',(-0.00352712997637068,-0.00811830261348138,
-0.00168785720747976));
#47312=CARTESIAN_POINT('Ctrl Pts',(-0.00341440081056064,-0.00812174001897434,
-0.00168445098079964));
#47313=CARTESIAN_POINT('Ctrl Pts',(-0.00342589891034995,-0.00807047763497546,
-0.00178991393060475));
#47314=CARTESIAN_POINT('Ctrl Pts',(-0.0035392791351489,-0.00858849912814965,
-0.00179466521288696));
#47315=CARTESIAN_POINT('Ctrl Pts',(-0.00342573153923465,-0.00859176400850957,
-0.00179333404984997));
#47316=CARTESIAN_POINT('Ctrl Pts',(-0.00343811948343117,-0.00856602524158671,
-0.00190328650635992));
#47317=CARTESIAN_POINT('',(-0.00353642309488705,-0.00858783002638803,-0.00179790810359568));
#47318=CARTESIAN_POINT('',(-0.00343811948343117,-0.00856602524158671,-0.00190328650635992));
#47319=CARTESIAN_POINT('Ctrl Pts',(-0.00353638626969755,-0.00858857287636746,
-0.0017946721002847));
#47320=CARTESIAN_POINT('Ctrl Pts',(-0.00342608713477122,-0.00859102517803947,
-0.00179649023154958));
#47321=CARTESIAN_POINT('Ctrl Pts',(-0.00343811948343117,-0.00856602524158671,
-0.00190328650635992));
#47322=CARTESIAN_POINT('',(-0.00346348111810162,-0.00743152690402934,-0.000970909650152327));
#47323=CARTESIAN_POINT('Ctrl Pts',(-0.00346348111810161,-0.00743152690402934,
-0.000970909650152327));
#47324=CARTESIAN_POINT('Ctrl Pts',(-0.00346891490008736,-0.00748743871269397,
-0.00106078753922695));
#47325=CARTESIAN_POINT('Ctrl Pts',(-0.00347494633059866,-0.00755249303664913,
-0.0011489837185329));
#47326=CARTESIAN_POINT('Ctrl Pts',(-0.00348147326192271,-0.00762799489769548,
-0.00123298157944914));
#47327=CARTESIAN_POINT('Ctrl Pts',(-0.00349040136462214,-0.00773127289097472,
-0.00134788113814814));
#47328=CARTESIAN_POINT('Ctrl Pts',(-0.00350025660587228,-0.00785531577230295,
-0.00145410062115423));
#47329=CARTESIAN_POINT('Ctrl Pts',(-0.00350830630757828,-0.00797937744348274,
-0.00153649554303844));
#47330=CARTESIAN_POINT('Ctrl Pts',(-0.00351635600928428,-0.00810343911466254,
-0.00161889046492264));
#47331=CARTESIAN_POINT('Ctrl Pts',(-0.00352260017144614,-0.00822631358203606,
-0.00167942932986295));
#47332=CARTESIAN_POINT('Ctrl Pts',(-0.00352769155837584,-0.0083470181408938,
-0.00172511126229019));
#47333=CARTESIAN_POINT('Ctrl Pts',(-0.00353115476696423,-0.00842912250079946,
-0.00175618453621361));
#47334=CARTESIAN_POINT('Ctrl Pts',(-0.00353408460414614,-0.00851028574239199,
-0.0017800585327765));
#47335=CARTESIAN_POINT('Ctrl Pts',(-0.00353642309488705,-0.00858783002638803,
-0.00179790810359568));
#47336=CARTESIAN_POINT('',(-0.00351047268888782,-0.00801620582113018,0.00156083213605469));
#47337=CARTESIAN_POINT('Ctrl Pts',(-0.00351047268888782,-0.00801620582113018,
0.00156083213605469));
#47338=CARTESIAN_POINT('Ctrl Pts',(-0.00350519018615136,-0.00792957352973586,
0.0015060133715871));
#47339=CARTESIAN_POINT('Ctrl Pts',(-0.0034993421679523,-0.00784462670554804,
0.00144258322748745));
#47340=CARTESIAN_POINT('Ctrl Pts',(-0.00349300905755829,-0.00776351543005723,
0.00136932733695487));
#47341=CARTESIAN_POINT('Ctrl Pts',(-0.00348450377901836,-0.00765458412334417,
0.00127094570219624));
#47342=CARTESIAN_POINT('Ctrl Pts',(-0.00347512358267887,-0.00755333188928983,
0.0011538009990632));
#47343=CARTESIAN_POINT('Ctrl Pts',(-0.00346735993405672,-0.00747341176998912,
0.00103600768938707));
#47344=CARTESIAN_POINT('Ctrl Pts',(-0.00345959628543458,-0.00739349165068841,
0.000918214379710948));
#47345=CARTESIAN_POINT('Ctrl Pts',(-0.0034534491845298,-0.00733336819546107,
0.000800677106835236));
#47346=CARTESIAN_POINT('Ctrl Pts',(-0.00344838046399713,-0.00728767396264777,
0.000686692944772953));
#47347=CARTESIAN_POINT('Ctrl Pts',(-0.00343824302293181,-0.00719628549702117,
0.00045872462064838));
#47348=CARTESIAN_POINT('Ctrl Pts',(-0.00343241910335498,-0.00716194741939409,
0.00024557134629273));
#47349=CARTESIAN_POINT('Ctrl Pts',(-0.00343139975819657,-0.00715609923797259,
5.76277457690076E-5));
#47350=CARTESIAN_POINT('Ctrl Pts',(-0.0034308900856098,-0.00715317514721843,
-3.63440558877464E-5));
#47351=CARTESIAN_POINT('Ctrl Pts',(-0.00343158155666329,-0.00715675113122004,
-0.000123973903842955));
#47352=CARTESIAN_POINT('Ctrl Pts',(-0.0034334038173975,-0.00716863494412438,
-0.000221928606050654));
#47353=CARTESIAN_POINT('Ctrl Pts',(-0.00343522607813171,-0.00718051875702871,
-0.000319883308258354));
#47354=CARTESIAN_POINT('Ctrl Pts',(-0.00343817912854665,-0.00720169129494195,
-0.000428004954841905));
#47355=CARTESIAN_POINT('Ctrl Pts',(-0.00344241723298215,-0.0072364971068012,
-0.000541338231156834));
#47356=CARTESIAN_POINT('Ctrl Pts',(-0.00344763208804926,-0.00727932457061238,
-0.00068079128599747));
#47357=CARTESIAN_POINT('Ctrl Pts',(-0.00345479258345437,-0.00734336632775489,
-0.000827815016986945));
#47358=CARTESIAN_POINT('Ctrl Pts',(-0.00346348111810161,-0.00743152690402934,
-0.000970909650152327));
#47359=CARTESIAN_POINT('',(-0.00354320482548136,-0.00900000021011351,0.00184504509674603));
#47360=CARTESIAN_POINT('Ctrl Pts',(-0.00354320482548136,-0.00900000021011351,
0.00184504509674603));
#47361=CARTESIAN_POINT('Ctrl Pts',(-0.00354322509066825,-0.00892539297133586,
0.00184524864599605));
#47362=CARTESIAN_POINT('Ctrl Pts',(-0.00354247918437561,-0.00885283033216195,
0.00184089127245303));
#47363=CARTESIAN_POINT('Ctrl Pts',(-0.00354100586630036,-0.00877374298082574,
0.00183111770926393));
#47364=CARTESIAN_POINT('Ctrl Pts',(-0.0035391715477079,-0.00867527721065587,
0.00181894937374049));
#47365=CARTESIAN_POINT('Ctrl Pts',(-0.00353620967645606,-0.00856685861537494,
0.00179739568288771));
#47366=CARTESIAN_POINT('Ctrl Pts',(-0.00353198328180325,-0.00845354303295786,
0.00176225261832798));
#47367=CARTESIAN_POINT('Ctrl Pts',(-0.00352667750664014,-0.00831128774158746,
0.0017181343533731));
#47368=CARTESIAN_POINT('Ctrl Pts',(-0.00351937883628627,-0.00816158475318592,
0.0016521136331202));
#47369=CARTESIAN_POINT('Ctrl Pts',(-0.00351047268888782,-0.00801620582113018,
0.00156083213605469));
#47370=CARTESIAN_POINT('',(-0.0034634765427239,-0.0105683977214321,0.000971535379578606));
#47371=CARTESIAN_POINT('Ctrl Pts',(-0.0034634765427239,-0.0105683977214321,
0.000971535379578606));
#47372=CARTESIAN_POINT('Ctrl Pts',(-0.00346890409325003,-0.0105125988361509,
0.00106128251009728));
#47373=CARTESIAN_POINT('Ctrl Pts',(-0.00347493845705885,-0.010447588087778,
0.00114939417218175));
#47374=CARTESIAN_POINT('Ctrl Pts',(-0.00348148957894286,-0.0103720280455907,
0.0012334598492987));
#47375=CARTESIAN_POINT('Ctrl Pts',(-0.00349000372301041,-0.0102738266846141,
0.00134271553081146));
#47376=CARTESIAN_POINT('Ctrl Pts',(-0.00349939071363248,-0.0101567628383621,
0.00144438106450357));
#47377=CARTESIAN_POINT('Ctrl Pts',(-0.00350715691927826,-0.0100388897777746,
0.00152470936290966));
#47378=CARTESIAN_POINT('Ctrl Pts',(-0.00351492312492403,-0.0099210167171871,
0.00160503766131575));
#47379=CARTESIAN_POINT('Ctrl Pts',(-0.0035210685455935,-0.00980324920461495,
0.00166556629660723));
#47380=CARTESIAN_POINT('Ctrl Pts',(-0.00352613224855201,-0.00968880590963078,
0.00171162816198026));
#47381=CARTESIAN_POINT('Ctrl Pts',(-0.00353625965446902,-0.00945991931966244,
0.00180375189272631));
#47382=CARTESIAN_POINT('Ctrl Pts',(-0.00354206018954218,-0.00924486720432927,
0.00183852795183029));
#47383=CARTESIAN_POINT('Ctrl Pts',(-0.00354305136176962,-0.00905532986970067,
0.00184421517727053));
#47384=CARTESIAN_POINT('Ctrl Pts',(-0.00354314889548398,-0.00903667894330822,
0.00184477481383644));
#47385=CARTESIAN_POINT('Ctrl Pts',(-0.00354319985999355,-0.00901827657119821,
0.00184507818656813));
#47386=CARTESIAN_POINT('Ctrl Pts',(-0.00354320482548136,-0.00900000021011351,
0.00184504509674603));
#47387=CARTESIAN_POINT('',(-0.00351041058117098,-0.00998279412709383,-0.00156095906068015));
#47388=CARTESIAN_POINT('Ctrl Pts',(-0.00351041058117098,-0.00998279412709383,
-0.00156095906068015));
#47389=CARTESIAN_POINT('Ctrl Pts',(-0.00350503565073693,-0.0100712857860722,
-0.00150479333735148));
#47390=CARTESIAN_POINT('Ctrl Pts',(-0.00349908543560267,-0.0101583121039841,
-0.00143987313134139));
#47391=CARTESIAN_POINT('Ctrl Pts',(-0.00349265305418288,-0.0102406671409818,
-0.00136503525702602));
#47392=CARTESIAN_POINT('Ctrl Pts',(-0.00348415640625082,-0.0103494513857482,
-0.0012661805672085));
#47393=CARTESIAN_POINT('Ctrl Pts',(-0.0034748184629296,-0.010449817819995,
-0.00114927353402808));
#47394=CARTESIAN_POINT('Ctrl Pts',(-0.00346709473226563,-0.010529157575455,
-0.00103170790983867));
#47395=CARTESIAN_POINT('Ctrl Pts',(-0.00345937100160166,-0.0106084973309151,
-0.000914142285649252));
#47396=CARTESIAN_POINT('Ctrl Pts',(-0.00345326148359495,-0.0106682116915477,
-0.000796826453053891));
#47397=CARTESIAN_POINT('Ctrl Pts',(-0.00344822616196539,-0.0107135768056789,
-0.00068306236416258));
#47398=CARTESIAN_POINT('Ctrl Pts',(-0.00343815551870626,-0.0108043070339414,
-0.000455534186379958));
#47399=CARTESIAN_POINT('Ctrl Pts',(-0.00343238166095573,-0.010838317159131,
-0.000242698364579505));
#47400=CARTESIAN_POINT('Ctrl Pts',(-0.0034313904685574,-0.010843958746556,
-5.52436125775062E-5));
#47401=CARTESIAN_POINT('Ctrl Pts',(-0.00343089369236729,-0.010846786256444,
3.87069238425434E-5));
#47402=CARTESIAN_POINT('Ctrl Pts',(-0.0034315982829426,-0.0108431244209408,
0.000126235007852828));
#47403=CARTESIAN_POINT('Ctrl Pts',(-0.0034334326877276,-0.0108311652892733,
0.000224075842000479));
#47404=CARTESIAN_POINT('Ctrl Pts',(-0.00343526709251259,-0.0108192061576057,
0.00032191667614813));
#47405=CARTESIAN_POINT('Ctrl Pts',(-0.00343823131150726,-0.0107979583547719,
0.00042991273046499));
#47406=CARTESIAN_POINT('Ctrl Pts',(-0.00344246340899626,-0.0107631486692495,
0.000542994992638243));
#47407=CARTESIAN_POINT('Ctrl Pts',(-0.00344767087270343,-0.0107203164390168,
0.000682139182421738));
#47408=CARTESIAN_POINT('Ctrl Pts',(-0.00345479797208566,-0.0106564757789345,
0.000828721308141272));
#47409=CARTESIAN_POINT('Ctrl Pts',(-0.0034634765427239,-0.0105683977214321,
0.000971535379578606));
#47410=CARTESIAN_POINT('',(-0.00354320118263476,-0.00900000021011351,-0.00184454176892424));
#47411=CARTESIAN_POINT('Ctrl Pts',(-0.00354320118263475,-0.00900000021011351,
-0.00184454176892423));
#47412=CARTESIAN_POINT('Ctrl Pts',(-0.00354322235846656,-0.00918058010367667,
-0.00184454176892423));
#47413=CARTESIAN_POINT('Ctrl Pts',(-0.0035391615244012,-0.00936903830252743,
-0.00182124852647729));
#47414=CARTESIAN_POINT('Ctrl Pts',(-0.00353056522115507,-0.00958285903313648,
-0.00175004499730282));
#47415=CARTESIAN_POINT('Ctrl Pts',(-0.00352538552624717,-0.00971169652500126,
-0.00170714137385795));
#47416=CARTESIAN_POINT('Ctrl Pts',(-0.00351855915924712,-0.00984886947693798,
-0.00164452038017344));
#47417=CARTESIAN_POINT('Ctrl Pts',(-0.00351041058117098,-0.00998279412709383,
-0.00156095906068015));
#47418=CARTESIAN_POINT('',(-0.00344269829706477,-0.00899998224949465,-0.0019508416734421));
#47419=CARTESIAN_POINT('Ctrl Pts',(-0.0035430763752057,-0.00899997871652083,
-0.00183940200010974));
#47420=CARTESIAN_POINT('Ctrl Pts',(-0.00343036413387564,-0.00900359568068924,
-0.00184212383138552));
#47421=CARTESIAN_POINT('Ctrl Pts',(-0.00344269760915441,-0.00899966251490034,
-0.00195083018299261));
#47422=CARTESIAN_POINT('Ctrl Pts',(-0.00343811948343117,-0.00856602524158671,
-0.00190328650635992));
#47423=CARTESIAN_POINT('Ctrl Pts',(-0.00342588491711595,-0.00806991020548021,
-0.00178978411271727));
#47424=CARTESIAN_POINT('Ctrl Pts',(-0.00338833186763894,-0.0076211810804679,
-0.00147075499299911));
#47425=CARTESIAN_POINT('Ctrl Pts',(-0.00336304853230225,-0.00735085164113558,
-0.0010394704028618));
#47426=CARTESIAN_POINT('Ctrl Pts',(-0.00333770359226152,-0.007079863524264,
-0.000607134956135401));
#47427=CARTESIAN_POINT('Ctrl Pts',(-0.00332461392794817,-0.00698753194456297,
-6.19190052309529E-5));
#47428=CARTESIAN_POINT('Ctrl Pts',(-0.00333682039814131,-0.00710081857461815,
0.000435571842955638));
#47429=CARTESIAN_POINT('Ctrl Pts',(-0.00334902702020896,-0.0072141066142004,
0.00093306888098847));
#47430=CARTESIAN_POINT('Ctrl Pts',(-0.00338655269909503,-0.00753311840533425,
0.00138301292867687));
#47431=CARTESIAN_POINT('Ctrl Pts',(-0.00341190064738082,-0.00796439294659748,
0.00165407866047813));
#47432=CARTESIAN_POINT('Ctrl Pts',(-0.00343719647682001,-0.008394780728451,
0.00192458704408161));
#47433=CARTESIAN_POINT('Ctrl Pts',(-0.0034503670171907,-0.00893739172396015,
0.00201689158354413));
#47434=CARTESIAN_POINT('Ctrl Pts',(-0.00343812749401439,-0.00943381877923568,
0.0019033576050533));
#47435=CARTESIAN_POINT('Ctrl Pts',(-0.0034258863648898,-0.00993031097072339,
0.00178980872976497));
#47436=CARTESIAN_POINT('Ctrl Pts',(-0.00338827163289001,-0.0103792185588139,
0.00147031465433104));
#47437=CARTESIAN_POINT('Ctrl Pts',(-0.00336301754592899,-0.0106492742069023,
0.00103896446141111));
#47438=CARTESIAN_POINT('Ctrl Pts',(-0.00333768686130201,-0.0109201489553746,
0.000606305948849976));
#47439=CARTESIAN_POINT('Ctrl Pts',(-0.00332462452155332,-0.0110126317008106,
6.0649363322396E-5));
#47440=CARTESIAN_POINT('Ctrl Pts',(-0.0033368677474717,-0.0108989627167492,
-0.000437415336783552));
#47441=CARTESIAN_POINT('Ctrl Pts',(-0.00334908127026236,-0.0107855695034998,
-0.000934271688738113));
#47442=CARTESIAN_POINT('Ctrl Pts',(-0.00338659264096821,-0.0104663958268669,
-0.00138368266598467));
#47443=CARTESIAN_POINT('Ctrl Pts',(-0.00341194350505705,-0.0100347423930322,
-0.00165451698700712));
#47444=CARTESIAN_POINT('Ctrl Pts',(-0.00342998476581804,-0.00972755080654826,
-0.00184725963244392));
#47445=CARTESIAN_POINT('Ctrl Pts',(-0.00344182965882166,-0.00936349053257669,
-0.00194935387765926));
#47446=CARTESIAN_POINT('Ctrl Pts',(-0.00344269801735234,-0.00900009946290338,
-0.00195084119718763));
#47447=CARTESIAN_POINT('Ctrl Pts',(-0.00344269811071666,-0.00900006039175898,
-0.00195084135710151));
#47448=CARTESIAN_POINT('Ctrl Pts',(-0.00344269820395414,-0.00900002132062265,
-0.001950841515853));
#47449=CARTESIAN_POINT('Ctrl Pts',(-0.00344269829706477,-0.00899998224949465,
-0.0019508416734421));
#47450=CARTESIAN_POINT('Ctrl Pts',(-0.00326780102756652,-0.00830776627881815,
-0.0010397814251779));
#47451=CARTESIAN_POINT('Ctrl Pts',(-0.0033697381364207,-0.00830650974827726,
-0.00103678809623668));
#47452=CARTESIAN_POINT('Ctrl Pts',(-0.00336771328390501,-0.00824815804099986,
-0.00112260420442851));
#47453=CARTESIAN_POINT('Ctrl Pts',(-0.00326464920350823,-0.00823890453247449,
-0.000994386776895733));
#47454=CARTESIAN_POINT('Ctrl Pts',(-0.00336706234466192,-0.00823684759055849,
-0.000991078081392678));
#47455=CARTESIAN_POINT('Ctrl Pts',(-0.0033645459846626,-0.00817342874147058,
-0.00107361247034106));
#47456=CARTESIAN_POINT('Ctrl Pts',(-0.00324793746847567,-0.00791953227740259,
-0.00073567091108549));
#47457=CARTESIAN_POINT('Ctrl Pts',(-0.00335277774940962,-0.00791087001891881,
-0.000729341170399936));
#47458=CARTESIAN_POINT('Ctrl Pts',(-0.00334776231449907,-0.00782709178377431,
-0.000794513134553083));
#47459=CARTESIAN_POINT('Ctrl Pts',(-0.00321793190913946,-0.0076149676140644,
-1.54083867402206E-6));
#47460=CARTESIAN_POINT('Ctrl Pts',(-0.00332799412930291,-0.00761878655976351,
-1.51388930652299E-6));
#47461=CARTESIAN_POINT('Ctrl Pts',(-0.00331757760893123,-0.00749558137023603,
-1.66483058764779E-6));
#47462=CARTESIAN_POINT('Ctrl Pts',(-0.00325780785275684,-0.008019466089899,
0.000978742800856142));
#47463=CARTESIAN_POINT('Ctrl Pts',(-0.00336067162260847,-0.00800363754489395,
0.000962724449561964));
#47464=CARTESIAN_POINT('Ctrl Pts',(-0.0033577150665097,-0.00793612611646283,
0.0010576437152649));
#47465=CARTESIAN_POINT('Ctrl Pts',(-0.00329800025932114,-0.00899946420378033,
0.00138546387197374));
#47466=CARTESIAN_POINT('Ctrl Pts',(-0.0033953190356324,-0.00899944782531834,
0.00138926904137042));
#47467=CARTESIAN_POINT('Ctrl Pts',(-0.00339807408715874,-0.00899941917617344,
0.00149541593485778));
#47468=CARTESIAN_POINT('Ctrl Pts',(-0.00325786406347626,-0.00997987109426551,
0.000979401186339539));
#47469=CARTESIAN_POINT('Ctrl Pts',(-0.00336071891445555,-0.00999571441285378,
0.000963399852332962));
#47470=CARTESIAN_POINT('Ctrl Pts',(-0.00335777157893346,-0.010063153048397,
0.00105835340798998));
#47471=CARTESIAN_POINT('Ctrl Pts',(-0.00321793255865113,-0.0103850227343342,
-4.38299481707064E-7));
#47472=CARTESIAN_POINT('Ctrl Pts',(-0.00332799471446149,-0.0103812033852223,
-4.47410730017003E-7));
#47473=CARTESIAN_POINT('Ctrl Pts',(-0.00331757825861524,-0.0105044081817788,
-4.72359875001561E-7));
#47474=CARTESIAN_POINT('Ctrl Pts',(-0.00325784210153424,-0.00998003788779652,
-0.000978747541355083));
#47475=CARTESIAN_POINT('Ctrl Pts',(-0.00336070043689,-0.00999586177973733,
-0.00096275163289535));
#47476=CARTESIAN_POINT('Ctrl Pts',(-0.00335774949912804,-0.0100633355839779,
-0.00105764734367712));
#47477=CARTESIAN_POINT('Ctrl Pts',(-0.00328460231345262,-0.00932704381043793,
-0.00124988324087735));
#47478=CARTESIAN_POINT('Ctrl Pts',(-0.00338399728153908,-0.00932579560598706,
-0.00124988491617768));
#47479=CARTESIAN_POINT('Ctrl Pts',(-0.00338460037758513,-0.00935537209178598,
-0.00134926500141788));
#47480=CARTESIAN_POINT('Ctrl Pts',(-0.00328461215845628,-0.00900048192889801,
-0.00124999990709781));
#47481=CARTESIAN_POINT('Ctrl Pts',(-0.00338400522957233,-0.00900048496365769,
-0.00124999990592778));
#47482=CARTESIAN_POINT('Ctrl Pts',(-0.00338461030538419,-0.00900052330173693,
-0.00134939112791716));
#47483=CARTESIAN_POINT('Ctrl Pts',(-0.003284619521066,-0.00875626183863264,
-0.001250087156212));
#47484=CARTESIAN_POINT('Ctrl Pts',(-0.0033840111734513,-0.00875720376069227,
-0.00125008590017788));
#47485=CARTESIAN_POINT('Ctrl Pts',(-0.00338461772991996,-0.00873514851728435,
-0.00134948545201661));
#47486=CARTESIAN_POINT('Ctrl Pts',(-0.0032771491209721,-0.00851200548284287,
-0.00117441883018739));
#47487=CARTESIAN_POINT('Ctrl Pts',(-0.00337760001855469,-0.00851118773616096,
-0.00117109105455409));
#47488=CARTESIAN_POINT('Ctrl Pts',(-0.00337711394211846,-0.0084699572931819,
-0.00126801343550846));
#47489=CARTESIAN_POINT('Ctrl Pts',(-0.00326780102756652,-0.00830776627881815,
-0.0010397814251779));
#47490=CARTESIAN_POINT('Ctrl Pts',(-0.0033697381364207,-0.00830650974827726,
-0.00103678809623668));
#47491=CARTESIAN_POINT('Ctrl Pts',(-0.00336771328390501,-0.00824815804099986,
-0.00112260420442851));
#47492=CARTESIAN_POINT('',(-0.00338450873183093,-0.00900052178030338,-0.00134545296373893));
#47493=CARTESIAN_POINT('',(-0.00328461216640222,-0.00900000000000097,-0.00124999998094225));
#47494=CARTESIAN_POINT('Ctrl Pts',(-0.00338450873198576,-0.0090005217803047,
-0.00134545296714054));
#47495=CARTESIAN_POINT('Ctrl Pts',(-0.00338016405263189,-0.00900048484637538,
-0.001249999905973));
#47496=CARTESIAN_POINT('Ctrl Pts',(-0.00328461215845628,-0.00900048192889801,
-0.00124999990709781));
#47497=CARTESIAN_POINT('',(-0.00336798809794631,-0.00974865428221822,-0.00111800482524904));
#47498=CARTESIAN_POINT('Ctrl Pts',(-0.00338450873183093,-0.00900052178030331,
-0.00134545296373893));
#47499=CARTESIAN_POINT('Ctrl Pts',(-0.00338450865110421,-0.00900327476401382,
-0.00134545189664552));
#47500=CARTESIAN_POINT('Ctrl Pts',(-0.00338450777831145,-0.00900602772712384,
-0.00134544238252916));
#47501=CARTESIAN_POINT('Ctrl Pts',(-0.00338450330004073,-0.00901345676316639,
-0.0013453939127586));
#47502=CARTESIAN_POINT('Ctrl Pts',(-0.00338449821153448,-0.00901813267771828,
-0.00134533903309341));
#47503=CARTESIAN_POINT('Ctrl Pts',(-0.00338444973233171,-0.00904904765956048,
-0.00134481503658746));
#47504=CARTESIAN_POINT('Ctrl Pts',(-0.00338433794923329,-0.00907526822596815,
-0.00134360289963365));
#47505=CARTESIAN_POINT('Ctrl Pts',(-0.00338369809843344,-0.0091694579286069,
-0.00133648353622328));
#47506=CARTESIAN_POINT('Ctrl Pts',(-0.00338279100650046,-0.00923698523823002,
-0.00132617824733123));
#47507=CARTESIAN_POINT('Ctrl Pts',(-0.00338117494196493,-0.00932185601914471,
-0.00130653740876165));
#47508=CARTESIAN_POINT('Ctrl Pts',(-0.00338079683170026,-0.00934018495676536,
-0.00130188671281531));
#47509=CARTESIAN_POINT('Ctrl Pts',(-0.00338022254096741,-0.00936612142649954,
-0.00129472079666794));
#47510=CARTESIAN_POINT('Ctrl Pts',(-0.00338004723694626,-0.00937381430467724,
-0.00129252132910337));
#47511=CARTESIAN_POINT('Ctrl Pts',(-0.00337853814796015,-0.0094382488903721,
-0.00127347571440452));
#47512=CARTESIAN_POINT('Ctrl Pts',(-0.00337697029016163,-0.00949383715135224,
-0.00125297317161244));
#47513=CARTESIAN_POINT('Ctrl Pts',(-0.00337295941941667,-0.00961784810662058,
-0.00119770077189597));
#47514=CARTESIAN_POINT('Ctrl Pts',(-0.00337040139297908,-0.0096850095454096,
-0.00116060817391342));
#47515=CARTESIAN_POINT('Ctrl Pts',(-0.0033676724655748,-0.00974864493507495,
-0.00111801108221903));
#47516=CARTESIAN_POINT('',(-0.00335782220510489,-0.00995293472304761,-0.000949979974017949));
#47517=CARTESIAN_POINT('Origin',(-0.00336290519953541,-0.00899804839933691,
2.75513276777065E-6));
#47518=CARTESIAN_POINT('',(-0.0033395154778931,-0.0102443751187985,0.000513026049606027));
#47519=CARTESIAN_POINT('Ctrl Pts',(-0.00333951547892669,-0.0102443751214304,
0.000513026050658624));
#47520=CARTESIAN_POINT('Ctrl Pts',(-0.00333720158736698,-0.0102754775655337,
0.00043752897741956));
#47521=CARTESIAN_POINT('Ctrl Pts',(-0.00333524185476234,-0.0102996487655498,
0.000359348111851545));
#47522=CARTESIAN_POINT('Ctrl Pts',(-0.00333219371656032,-0.0103353522363518,
0.000190907331342745));
#47523=CARTESIAN_POINT('Ctrl Pts',(-0.00333122867855846,-0.0103451419971487,
0.000100686070978564));
#47524=CARTESIAN_POINT('Ctrl Pts',(-0.00333114619591799,-0.0103458982369924,
-3.36368651573786E-6));
#47525=CARTESIAN_POINT('Ctrl Pts',(-0.00333115576494018,-0.0103457925958847,
-1.68909191838913E-5));
#47526=CARTESIAN_POINT('Ctrl Pts',(-0.00333120143442851,-0.0103453098793274,
-3.79805317566844E-5));
#47527=CARTESIAN_POINT('Ctrl Pts',(-0.00333122396405323,-0.010345072876226,
-4.5545203362486E-5));
#47528=CARTESIAN_POINT('Ctrl Pts',(-0.00333134781289938,-0.010343766788362,
-7.83812280955537E-5));
#47529=CARTESIAN_POINT('Ctrl Pts',(-0.00333151003988135,-0.010342049212991,
-0.000103621277838774));
#47530=CARTESIAN_POINT('Ctrl Pts',(-0.00333213219199593,-0.0103352897395069,
-0.000173718461075599));
#47531=CARTESIAN_POINT('Ctrl Pts',(-0.00333272515882828,-0.0103287014280872,
-0.000218391262500524));
#47532=CARTESIAN_POINT('Ctrl Pts',(-0.00333561490513267,-0.0102950073937465,
-0.000387468756320592));
#47533=CARTESIAN_POINT('Ctrl Pts',(-0.00333902150429297,-0.0102525546405954,
-0.000508114028806056));
#47534=CARTESIAN_POINT('Ctrl Pts',(-0.00334530384177048,-0.010162122328243,
-0.000681861044479222));
#47535=CARTESIAN_POINT('Ctrl Pts',(-0.00334769471416655,-0.0101258236197889,
-0.000740228332633532));
#47536=CARTESIAN_POINT('Ctrl Pts',(-0.00335265664561079,-0.010045090781357,
-0.000850303231101744));
#47537=CARTESIAN_POINT('Ctrl Pts',(-0.00335521909692295,-0.0100008637934157,
-0.000901921239805929));
#47538=CARTESIAN_POINT('Ctrl Pts',(-0.00335779790172574,-0.00995293407100622,
-0.000949980627823781));
#47539=CARTESIAN_POINT('',(-0.00338454060301105,-0.00900002810628826,0.00134621762248316));
#47540=CARTESIAN_POINT('Ctrl Pts',(-0.00338454060675955,-0.0090000281062885,
0.00134621763156711));
#47541=CARTESIAN_POINT('Ctrl Pts',(-0.00338454054544131,-0.00900662374474969,
0.00134621749439546));
#47542=CARTESIAN_POINT('Ctrl Pts',(-0.00338453591899628,-0.00901321923754373,
0.0013461688717259));
#47543=CARTESIAN_POINT('Ctrl Pts',(-0.00338451628347078,-0.00902742516719074,
0.00134595970333058));
#47544=CARTESIAN_POINT('Ctrl Pts',(-0.00338449978460471,-0.00903503515915829,
0.00134578306823355));
#47545=CARTESIAN_POINT('Ctrl Pts',(-0.00338443289937514,-0.00905779189537234,
0.00134506165343333));
#47546=CARTESIAN_POINT('Ctrl Pts',(-0.00338436513907917,-0.00907293127221901,
0.00134432556283098));
#47547=CARTESIAN_POINT('Ctrl Pts',(-0.00338409618593173,-0.0091180888868096,
0.00134136466489044));
#47548=CARTESIAN_POINT('Ctrl Pts',(-0.00338382938092011,-0.00914804765314941,
0.00133838846566736));
#47549=CARTESIAN_POINT('Ctrl Pts',(-0.00338278037558188,-0.00923814805753341,
0.0013263743961517));
#47550=CARTESIAN_POINT('Ctrl Pts',(-0.00338175141220183,-0.00929779697665544,
0.00131426408186406));
#47551=CARTESIAN_POINT('Ctrl Pts',(-0.00338028716191064,-0.00936421426237214,
0.00129602352001954));
#47552=CARTESIAN_POINT('Ctrl Pts',(-0.0033801106422181,-0.00937199137910707,
0.00129381208644705));
#47553=CARTESIAN_POINT('Ctrl Pts',(-0.00337973723180336,-0.00938799351482061,
0.00128910559654723));
#47554=CARTESIAN_POINT('Ctrl Pts',(-0.00337953976697067,-0.00939621550146254,
0.00128660155700354));
#47555=CARTESIAN_POINT('Ctrl Pts',(-0.00337872702498143,-0.00942914195675233,
0.00127622800099797));
#47556=CARTESIAN_POINT('Ctrl Pts',(-0.0033780724469702,-0.0094536398055474,
0.00126772435961022));
#47557=CARTESIAN_POINT('Ctrl Pts',(-0.00337621160674814,-0.00951863915914454,
0.00124303578009676));
#47558=CARTESIAN_POINT('Ctrl Pts',(-0.00337493469975409,-0.00955862344005493,
0.00122558171909746));
#47559=CARTESIAN_POINT('Ctrl Pts',(-0.00337148711508259,-0.0096573552598843,
0.00117664413953565));
#47560=CARTESIAN_POINT('Ctrl Pts',(-0.00336920456265393,-0.0097147409601528,
0.00114268340946798));
#47561=CARTESIAN_POINT('Ctrl Pts',(-0.00336263194246688,-0.00986438322421787,
0.00103842072052163));
#47562=CARTESIAN_POINT('Ctrl Pts',(-0.00335813345016562,-0.00995045109400686,
0.000960238410779958));
#47563=CARTESIAN_POINT('Ctrl Pts',(-0.0033511420936047,-0.0100714232924326,
0.000817918363258607));
#47564=CARTESIAN_POINT('Ctrl Pts',(-0.00334855089328028,-0.0101130526115715,
0.000760269195348086));
#47565=CARTESIAN_POINT('Ctrl Pts',(-0.00334372576596367,-0.0101862077048872,
0.000639957996819968));
#47566=CARTESIAN_POINT('Ctrl Pts',(-0.00334149390895866,-0.0102177818226984,
0.000577577769343556));
#47567=CARTESIAN_POINT('Ctrl Pts',(-0.00333951547892579,-0.0102443751214424,
0.000513026050629553));
#47568=CARTESIAN_POINT('',(-0.00333951973713618,-0.00775564716847025,0.0005130795639787));
#47569=CARTESIAN_POINT('Ctrl Pts',(-0.00333951974170471,-0.00775564716011877,
0.000513079567279669));
#47570=CARTESIAN_POINT('Ctrl Pts',(-0.00334149417117988,-0.00778219525425979,
0.000577513689473508));
#47571=CARTESIAN_POINT('Ctrl Pts',(-0.00334372094979989,-0.00781370628872191,
0.000639784345303221));
#47572=CARTESIAN_POINT('Ctrl Pts',(-0.00334854033125506,-0.00788678174994642,
0.000760028693420967));
#47573=CARTESIAN_POINT('Ctrl Pts',(-0.00335113155174353,-0.00792841497623692,
0.000817708394398717));
#47574=CARTESIAN_POINT('Ctrl Pts',(-0.00335812613437231,-0.00804944390357773,
0.000960146213641191));
#47575=CARTESIAN_POINT('Ctrl Pts',(-0.00336262891395931,-0.00813558116512314,
0.00103840197563686));
#47576=CARTESIAN_POINT('Ctrl Pts',(-0.00336914360363133,-0.00828388637151784,
0.00114172335762287));
#47577=CARTESIAN_POINT('Ctrl Pts',(-0.00337137024002632,-0.0083397105219415,
0.00117490230676323));
#47578=CARTESIAN_POINT('Ctrl Pts',(-0.00337479463125309,-0.00843708313587216,
0.001223630170499));
#47579=CARTESIAN_POINT('Ctrl Pts',(-0.00337609125760534,-0.00847739854758708,
0.0012413895470228));
#47580=CARTESIAN_POINT('Ctrl Pts',(-0.00337798033922486,-0.00854293077009745,
0.0012664960464477));
#47581=CARTESIAN_POINT('Ctrl Pts',(-0.00337864447915115,-0.00856761559147129,
0.00127513723333758));
#47582=CARTESIAN_POINT('Ctrl Pts',(-0.00337946877993396,-0.00860078220827126,
0.00128567317765247));
#47583=CARTESIAN_POINT('Ctrl Pts',(-0.00337966877160793,-0.00860905215495234,
0.00128821275223784));
#47584=CARTESIAN_POINT('Ctrl Pts',(-0.00338023165440961,-0.00863300704057187,
0.00129531691606092));
#47585=CARTESIAN_POINT('Ctrl Pts',(-0.00338058140838721,-0.00864875161229656,
0.00129967598971537));
#47586=CARTESIAN_POINT('Ctrl Pts',(-0.00338206491416227,-0.0087198150702577,
0.00131796455658876));
#47587=CARTESIAN_POINT('Ctrl Pts',(-0.00338297907469519,-0.00877591025581751,
0.00132865611872142));
#47588=CARTESIAN_POINT('Ctrl Pts',(-0.00338391060684845,-0.00886062949802715,
0.00133928156763364));
#47589=CARTESIAN_POINT('Ctrl Pts',(-0.00338414750987857,-0.00888884576435987,
0.00134191880644743));
#47590=CARTESIAN_POINT('Ctrl Pts',(-0.00338438590382474,-0.00893136516583988,
0.00134454209115992));
#47591=CARTESIAN_POINT('Ctrl Pts',(-0.00338444586200037,-0.00894561869572669,
0.00134519417029263));
#47592=CARTESIAN_POINT('Ctrl Pts',(-0.00338450489567835,-0.00896703848358398,
0.00134583299070457));
#47593=CARTESIAN_POINT('Ctrl Pts',(-0.00338451941982857,-0.00897419859695921,
0.00134598934228585));
#47594=CARTESIAN_POINT('Ctrl Pts',(-0.00338453325841651,-0.00898494452379937,
0.00134613819300853));
#47595=CARTESIAN_POINT('Ctrl Pts',(-0.00338453654617301,-0.00898852960715314,
0.00134617352521678));
#47596=CARTESIAN_POINT('Ctrl Pts',(-0.00338453992474177,-0.0089947519580479,
0.00134620998295414));
#47597=CARTESIAN_POINT('Ctrl Pts',(-0.00338454063097428,-0.00899738915780249,
0.00134621768306205));
#47598=CARTESIAN_POINT('Ctrl Pts',(-0.00338454060677552,-0.00900002637780627,
0.00134621763160195));
#47599=CARTESIAN_POINT('',(-0.00335781975105043,-0.0080470214493883,-0.000949935792125509));
#47600=CARTESIAN_POINT('Ctrl Pts',(-0.00335779717912834,-0.00804702205697391,
-0.00094993640141179));
#47601=CARTESIAN_POINT('Ctrl Pts',(-0.00335522018045496,-0.00799912930709866,
-0.000901909628323764));
#47602=CARTESIAN_POINT('Ctrl Pts',(-0.00335265916585628,-0.00795493403683286,
-0.000850329509246332));
#47603=CARTESIAN_POINT('Ctrl Pts',(-0.0033476987953991,-0.00787424156296798,
-0.000740324203404496));
#47604=CARTESIAN_POINT('Ctrl Pts',(-0.00334530809252378,-0.00783795350784308,
-0.000681986711934992));
#47605=CARTESIAN_POINT('Ctrl Pts',(-0.00333902318351723,-0.00774750315184934,
-0.000508260877900045));
#47606=CARTESIAN_POINT('Ctrl Pts',(-0.00333561409435754,-0.00770503036771147,
-0.000387600728429948));
#47607=CARTESIAN_POINT('Ctrl Pts',(-0.00333272868774576,-0.00767137842777274,
-0.000218810613518203));
#47608=CARTESIAN_POINT('Ctrl Pts',(-0.00333213872536355,-0.00766481632598804,
-0.000174448386311072));
#47609=CARTESIAN_POINT('Ctrl Pts',(-0.00333151671899573,-0.00765804482743786,
-0.000104793834325934));
#47610=CARTESIAN_POINT('Ctrl Pts',(-0.00333135366625433,-0.00765631286321025,
-7.96840624127513E-5));
#47611=CARTESIAN_POINT('Ctrl Pts',(-0.00333122767584969,-0.00765497703325505,
-4.69777802509182E-5));
#47612=CARTESIAN_POINT('Ctrl Pts',(-0.00333120453567573,-0.00765473195936074,
-3.9412892698668E-5));
#47613=CARTESIAN_POINT('Ctrl Pts',(-0.00333118003267711,-0.00765447067095878,
-2.85048715363367E-5));
#47614=CARTESIAN_POINT('Ctrl Pts',(-0.0033311737247941,-0.00765440307861096,
-2.51631309465576E-5));
#47615=CARTESIAN_POINT('Ctrl Pts',(-0.00333115945419868,-0.00765424868323619,
-1.58059170859384E-5));
#47616=CARTESIAN_POINT('Ctrl Pts',(-0.00333115420416645,-0.00765418976528437,
-9.79006205307497E-6));
#47617=CARTESIAN_POINT('Ctrl Pts',(-0.00333113514184231,-0.00765390670655867,
8.18657661644229E-5));
#47618=CARTESIAN_POINT('Ctrl Pts',(-0.00333192890168699,-0.00766181744535084,
0.000167330559431246));
#47619=CARTESIAN_POINT('Ctrl Pts',(-0.0033347928732721,-0.00769481203868999,
0.00034108911925425));
#47620=CARTESIAN_POINT('Ctrl Pts',(-0.0033369356378662,-0.00772090137562988,
0.000428749383032905));
#47621=CARTESIAN_POINT('Ctrl Pts',(-0.00333951979241417,-0.00775564784195628,
0.00051308122214492));
#47622=CARTESIAN_POINT('',(-0.00336798575526351,-0.00825128999511177,-0.0011179673661904));
#47623=CARTESIAN_POINT('Origin',(-0.00336290275316926,-0.00900195197300184,
2.75506903634454E-6));
#47624=CARTESIAN_POINT('',(-0.00326780067323885,-0.00830775851653247,-0.00103977630810674));
#47625=CARTESIAN_POINT('Ctrl Pts',(-0.0033676712709598,-0.00825129322272922,
-0.00111798268825413));
#47626=CARTESIAN_POINT('Ctrl Pts',(-0.00336429022081308,-0.00830656906493108,
-0.00103694292107723));
#47627=CARTESIAN_POINT('Ctrl Pts',(-0.00326780067212508,-0.00830775851309429,
-0.00103977630586051));
#47628=CARTESIAN_POINT('',(-0.00325791983579602,-0.00811636346334185,-0.000884130347337319));
#47629=CARTESIAN_POINT('Ctrl Pts',(-0.00325791983579602,-0.00811636346334185,
-0.000884130347337319));
#47630=CARTESIAN_POINT('Ctrl Pts',(-0.00326128379583907,-0.0081745896155171,
-0.000942286360207792));
#47631=CARTESIAN_POINT('Ctrl Pts',(-0.00326464894774107,-0.00823889962784297,
-0.000994382814554614));
#47632=CARTESIAN_POINT('Ctrl Pts',(-0.00326780067323886,-0.00830775851653247,
-0.00103977630810674));
#47633=CARTESIAN_POINT('',(-0.003257865684124,-0.00811545508239479,0.000883221550452495));
#47634=CARTESIAN_POINT('Ctrl Pts',(-0.003257865684124,-0.00811545508239479,
0.000883221550452495));
#47635=CARTESIAN_POINT('Ctrl Pts',(-0.00324452625828876,-0.00788477670656564,
0.000652165360404284));
#47636=CARTESIAN_POINT('Ctrl Pts',(-0.00323123706542317,-0.00774993409998482,
0.000325577072709837));
#47637=CARTESIAN_POINT('Ctrl Pts',(-0.00323124079846264,-0.0077500003261204,
-6.59450910766848E-7));
#47638=CARTESIAN_POINT('Ctrl Pts',(-0.00323124453297722,-0.00775006657842525,
-0.000327024886920311));
#47639=CARTESIAN_POINT('Ctrl Pts',(-0.00324455815677214,-0.00788518359895288,
-0.000653038877261263));
#47640=CARTESIAN_POINT('Ctrl Pts',(-0.00325789992482187,-0.00811601889883439,
-0.000883786056135089));
#47641=CARTESIAN_POINT('',(-0.00328461358329975,-0.00900001820654589,0.00124999997585377));
#47642=CARTESIAN_POINT('Ctrl Pts',(-0.00328461358329975,-0.00900001820654589,
0.00124999997585377));
#47643=CARTESIAN_POINT('Ctrl Pts',(-0.00328461606383265,-0.00867328446293999,
0.00125002453056291));
#47644=CARTESIAN_POINT('Ctrl Pts',(-0.00327122623192912,-0.00834657387630014,
0.00111456735937024));
#47645=CARTESIAN_POINT('Ctrl Pts',(-0.00325788149737239,-0.00811572858503246,
0.000883495411303269));
#47646=CARTESIAN_POINT('',(-0.00325789817864836,-0.00988399521919616,0.000883771719641636));
#47647=CARTESIAN_POINT('Ctrl Pts',(-0.00325789817864836,-0.00988399521919616,
0.000883771719641636));
#47648=CARTESIAN_POINT('Ctrl Pts',(-0.00327123613082152,-0.00965318416122461,
0.0011146399923813));
#47649=CARTESIAN_POINT('Ctrl Pts',(-0.00328461110399896,-0.00932658965853997,
0.00124997543334117));
#47650=CARTESIAN_POINT('Ctrl Pts',(-0.00328461358329975,-0.00900001820654589,
0.00124999997585377));
#47651=CARTESIAN_POINT('',(-0.00325788569625234,-0.00988421312102252,-0.000883553669847396));
#47652=CARTESIAN_POINT('Ctrl Pts',(-0.00325788569625234,-0.00988421312102252,
-0.000883553669847396));
#47653=CARTESIAN_POINT('Ctrl Pts',(-0.00324454916963038,-0.0101148915861028,
-0.000652826446188782));
#47654=CARTESIAN_POINT('Ctrl Pts',(-0.00323124877940481,-0.0102498954446246,
-0.000326895092343441));
#47655=CARTESIAN_POINT('Ctrl Pts',(-0.0032312407867353,-0.0102499999301743,
-6.63048329690229E-7));
#47656=CARTESIAN_POINT('Ctrl Pts',(-0.00323123279101768,-0.0102501044555711,
0.000325693408701394));
#47657=CARTESIAN_POINT('Ctrl Pts',(-0.00324453375313502,-0.0101151697465547,
0.000652349462123238));
#47658=CARTESIAN_POINT('Ctrl Pts',(-0.00325787829355509,-0.00988433925695948,
0.000883427454797046));
#47659=CARTESIAN_POINT('Ctrl Pts',(-0.00328461216640222,-0.00900000000000097,
-0.00124999998094225));
#47660=CARTESIAN_POINT('Ctrl Pts',(-0.00328461546930389,-0.00932656366198307,
-0.00125001656791605));
#47661=CARTESIAN_POINT('Ctrl Pts',(-0.00327124259279507,-0.00965310972898778,
-0.00111456015950205));
#47662=CARTESIAN_POINT('Ctrl Pts',(-0.00325790095446365,-0.00988394916218192,
-0.000883817601168605));
#47663=CARTESIAN_POINT('Origin',(2.6675363272169E-19,-0.002,0.));
#47664=CARTESIAN_POINT('',(0.0055,-0.002,-6.73555739531044E-19));
#47665=CARTESIAN_POINT('Origin',(2.6675363272169E-19,-0.002,0.));
#47666=CARTESIAN_POINT('',(0.0036018008897227,-0.002,0.00302090833547154));
#47667=CARTESIAN_POINT('',(0.00360180088972267,-0.002,-0.00302090833547154));
#47668=CARTESIAN_POINT('Origin',(0.0203312393987904,-0.002,-7.17008776061679E-17));
#47669=CARTESIAN_POINT('',(0.00302090833547152,-0.002,-0.00360180088972268));
#47670=CARTESIAN_POINT('Origin',(0.00310975858063245,-0.002,-0.00310975858063246));
#47671=CARTESIAN_POINT('',(-0.00302090833547157,-0.002,-0.00360180088972269));
#47672=CARTESIAN_POINT('Origin',(-4.47981017017182E-19,-0.002,-0.0203312393987904));
#47673=CARTESIAN_POINT('',(-0.00360180088972273,-0.002,-0.00302090833547154));
#47674=CARTESIAN_POINT('Origin',(-0.0031097585806325,-0.002,-0.00310975858063247));
#47675=CARTESIAN_POINT('',(-0.00360180088972265,-0.002,0.00302090833547154));
#47676=CARTESIAN_POINT('Origin',(-0.0203312393987904,-0.002,2.13673163519026E-16));
#47677=CARTESIAN_POINT('',(-0.00302090833547149,-0.002,0.00360180088972268));
#47678=CARTESIAN_POINT('Origin',(-0.00310975858063242,-0.002,0.00310975858063246));
#47679=CARTESIAN_POINT('',(0.00302090833547155,-0.002,0.00360180088972269));
#47680=CARTESIAN_POINT('Origin',(9.81488282460562E-19,-0.002,0.0203312393987904));
#47681=CARTESIAN_POINT('Origin',(0.00310975858063248,-0.002,0.00310975858063246));
#47682=CARTESIAN_POINT('Origin',(2.6675363272169E-19,-0.002,0.));
#47683=CARTESIAN_POINT('',(0.0055,0.014,-6.73555739531044E-19));
#47684=CARTESIAN_POINT('Origin',(-1.86727542905182E-18,0.014,0.));
#47685=CARTESIAN_POINT('',(0.0055,-0.002,-6.73555739531044E-19));
#47686=CARTESIAN_POINT('Origin',(-2.00065224541267E-18,0.015,0.));
#47687=CARTESIAN_POINT('',(0.0045,0.015,-5.51091059616309E-19));
#47688=CARTESIAN_POINT('Origin',(-2.00065224541267E-18,0.015,0.));
#47689=CARTESIAN_POINT('Origin',(1.96519507615456E-18,-0.015,0.));
#47690=CARTESIAN_POINT('',(-0.00360180088972265,-0.015,0.00302090833547154));
#47691=CARTESIAN_POINT('',(-0.00360180088972272,-0.015,-0.00302090833547154));
#47692=CARTESIAN_POINT('Origin',(-0.0203312393987904,-0.015,2.13126180968845E-16));
#47693=CARTESIAN_POINT('',(-0.00302090833547157,-0.015,-0.00360180088972269));
#47694=CARTESIAN_POINT('Origin',(-0.0031097585806325,-0.015,-0.00310975858063247));
#47695=CARTESIAN_POINT('',(0.00302090833547153,-0.015,-0.00360180088972268));
#47696=CARTESIAN_POINT('Origin',(1.83290014585433E-18,-0.015,-0.0203312393987904));
#47697=CARTESIAN_POINT('',(0.00360180088972268,-0.015,-0.00302090833547154));
#47698=CARTESIAN_POINT('Origin',(0.00310975858063245,-0.015,-0.00310975858063246));
#47699=CARTESIAN_POINT('',(0.0036018008897227,-0.015,0.00302090833547154));
#47700=CARTESIAN_POINT('Origin',(0.0203312393987904,-0.015,-7.11538950559874E-17));
#47701=CARTESIAN_POINT('',(0.00302090833547155,-0.015,0.00360180088972269));
#47702=CARTESIAN_POINT('Origin',(0.00310975858063248,-0.015,0.00310975858063246));
#47703=CARTESIAN_POINT('',(-0.00302090833547149,-0.015,0.00360180088972268));
#47704=CARTESIAN_POINT('Origin',(2.16840434497101E-18,-0.015,0.0203312393987904));
#47705=CARTESIAN_POINT('Origin',(-0.00310975858063242,-0.015,0.00310975858063246));
#47706=CARTESIAN_POINT('',(0.00278445714771808,-0.015,0.));
#47707=CARTESIAN_POINT('Origin',(1.7347234759768E-18,-0.015,0.));
#47708=CARTESIAN_POINT('Origin',(3.08141670074827E-18,-0.025,0.0203312393987904));
#47709=CARTESIAN_POINT('',(0.00302090833547155,-0.025,0.00360180088972269));
#47710=CARTESIAN_POINT('',(-0.00302090833547149,-0.025,0.00360180088972268));
#47711=CARTESIAN_POINT('Origin',(-0.0203312393987904,-0.025,2.12705425161014E-16));
#47712=CARTESIAN_POINT('',(-0.00360180088972272,-0.025,-0.00302090833547154));
#47713=CARTESIAN_POINT('',(-0.00360180088972265,-0.025,0.00302090833547154));
#47714=CARTESIAN_POINT('Ctrl Pts',(-0.00344269829706477,-0.00899998224949465,
-0.0019508416734421));
#47715=CARTESIAN_POINT('Ctrl Pts',(-0.00344304626547968,-0.00885396756551811,
-0.00195143060758549));
#47716=CARTESIAN_POINT('Ctrl Pts',(-0.00344162236167648,-0.00870806791987832,
-0.00193578337263521));
#47717=CARTESIAN_POINT('Ctrl Pts',(-0.00343811948343117,-0.00856602524158671,
-0.00190328650635992));
#47718=CARTESIAN_POINT('Origin',(0.0203312393987904,-0.025,-7.07331392481562E-17));
#47719=CARTESIAN_POINT('',(0.00360180088972268,-0.025,-0.00302090833547154));
#47720=CARTESIAN_POINT('',(0.0036018008897227,-0.025,0.00302090833547154));
#47721=CARTESIAN_POINT('Origin',(3.58742411729397E-18,-0.025,-0.0203312393987904));
#47722=CARTESIAN_POINT('',(-0.00302090833547157,-0.025,-0.00360180088972269));
#47723=CARTESIAN_POINT('',(0.00302090833547153,-0.025,-0.00360180088972268));
#47724=CARTESIAN_POINT('Origin',(-0.0031097585806325,-0.025,-0.00310975858063247));
#47725=CARTESIAN_POINT('Origin',(0.00310975858063245,-0.025,-0.00310975858063246));
#47726=CARTESIAN_POINT('Origin',(0.00310975858063248,-0.025,0.00310975858063246));
#47727=CARTESIAN_POINT('Origin',(-0.00310975858063242,-0.025,0.00310975858063246));
#47728=CARTESIAN_POINT('Origin',(1.76941794549634E-18,-0.0153,0.));
#47729=CARTESIAN_POINT('',(0.00278445714771808,-0.0152,0.));
#47730=CARTESIAN_POINT('',(0.00278445714771807,-0.0153,-3.4099765333159E-19));
#47731=CARTESIAN_POINT('',(-0.00278445714771807,-0.0152,-3.4099765333159E-19));
#47732=CARTESIAN_POINT('Origin',(1.75785312232316E-18,-0.0152,0.));
#47733=CARTESIAN_POINT('Origin',(1.75785312232316E-18,-0.0152,0.));
#47734=CARTESIAN_POINT('Origin',(1.76941794549634E-18,-0.0153,0.));
#47735=CARTESIAN_POINT('',(-0.00268445714771808,-0.0153,-3.28751185340118E-19));
#47736=CARTESIAN_POINT('Origin',(1.76941794549634E-18,-0.0153,0.));
#47737=CARTESIAN_POINT('',(-0.00126635989804114,-0.0153,-1.55084359570465E-19));
#47738=CARTESIAN_POINT('Origin',(1.76941794549634E-18,-0.0153,0.));
#47739=CARTESIAN_POINT('Origin',(1.75785312232316E-18,-0.0152,0.));
#47740=CARTESIAN_POINT('Origin',(-0.00268445714771808,-0.0152,-3.28751185340118E-19));
#47741=CARTESIAN_POINT('Origin',(1.65376971376455E-18,-0.0143,0.));
#47742=CARTESIAN_POINT('',(-0.00116635989804114,-0.0144,-1.42837891578992E-19));
#47743=CARTESIAN_POINT('Origin',(1.66533453693773E-18,-0.0144,0.));
#47744=CARTESIAN_POINT('',(-0.00116635989804114,-0.0152,-1.42837891578992E-19));
#47745=CARTESIAN_POINT('',(-0.00116635989804114,-0.0143,-1.42837891578992E-19));
#47746=CARTESIAN_POINT('Origin',(1.75785312232316E-18,-0.0152,0.));
#47747=CARTESIAN_POINT('Origin',(1.65376971376455E-18,-0.0143,0.));
#47748=CARTESIAN_POINT('',(-0.00106635989804114,-0.0143,-1.30591423587518E-19));
#47749=CARTESIAN_POINT('Origin',(1.65376971376455E-18,-0.0143,0.));
#47750=CARTESIAN_POINT('Origin',(0.00900100000597247,-0.00900000021011351,
2.5166391089677E-7));
#47751=CARTESIAN_POINT('',(0.00900100000597247,-0.00900000021011351,0.00184504509674603));
#47752=CARTESIAN_POINT('Ctrl Pts',(-0.00380975858063243,-0.00899998937218426,
-0.00184137848958098));
#47753=CARTESIAN_POINT('Ctrl Pts',(-0.00380975858063243,-0.00893815389736155,
-0.00184159034836062));
#47754=CARTESIAN_POINT('Ctrl Pts',(-0.00380975858063243,-0.00887631623328271,
-0.00183865163430941));
#47755=CARTESIAN_POINT('Ctrl Pts',(-0.00380975858063243,-0.00881478413029403,
-0.00183246684420301));
#47756=CARTESIAN_POINT('Ctrl Pts',(-0.00353642309488705,-0.00858783002638803,
-0.00179790810359568));
#47757=CARTESIAN_POINT('Ctrl Pts',(-0.00353752250310302,-0.0086242637078,
-0.00180623272293779));
#47758=CARTESIAN_POINT('Ctrl Pts',(-0.00353849120739254,-0.00865990950754595,
-0.0018132613329253));
#47759=CARTESIAN_POINT('Ctrl Pts',(-0.00353932318339466,-0.00869447214609225,
-0.00181906562890172));
#47760=CARTESIAN_POINT('Ctrl Pts',(-0.00354192480978627,-0.00880255107189962,
-0.00183721592357208));
#47761=CARTESIAN_POINT('Ctrl Pts',(-0.00354318945087198,-0.00889995594775555,
-0.00184454176892423));
#47762=CARTESIAN_POINT('Ctrl Pts',(-0.00354320118263475,-0.00900000021011351,
-0.00184454176892423));
#47763=CARTESIAN_POINT('Origin',(0.00900100000597247,-0.00900000011651052,
3.82283508649252E-7));
#47764=CARTESIAN_POINT('',(-0.00380975858586299,-0.00900000011611844,-0.00134544337418665));
#47765=CARTESIAN_POINT('',(-0.00380975862800813,-0.00900000011337439,0.00134614011498439));
#47766=CARTESIAN_POINT('Origin',(-0.00380975860693448,-0.00899994566615699,
3.48370398817743E-7));
#47767=CARTESIAN_POINT('',(0.00900100000597247,-0.00900000011651052,0.00134621763185817));
#47768=CARTESIAN_POINT('',(-0.00337654510570282,-0.0084833905958057,-0.00124235155283125));
#47769=CARTESIAN_POINT('Ctrl Pts',(-0.00337620712303714,-0.00848339943917672,
-0.00124235522901977));
#47770=CARTESIAN_POINT('Ctrl Pts',(-0.00337756738494765,-0.00852772695862544,
-0.00126078198957128));
#47771=CARTESIAN_POINT('Ctrl Pts',(-0.0033788015330959,-0.00857301218210894,
-0.00127682532428018));
#47772=CARTESIAN_POINT('Ctrl Pts',(-0.00338003388768656,-0.00862570568134062,
-0.0012923761846553));
#47773=CARTESIAN_POINT('Ctrl Pts',(-0.00338018599196866,-0.00863236541625167,
-0.001294285824698));
#47774=CARTESIAN_POINT('Ctrl Pts',(-0.00338149651939755,-0.00869118133026391,
-0.00131066051706739));
#47775=CARTESIAN_POINT('Ctrl Pts',(-0.00338245034165808,-0.00874415513497043,
-0.00132201949741684));
#47776=CARTESIAN_POINT('Ctrl Pts',(-0.00338401193656355,-0.00886334276963602,
-0.00134014367932438));
#47777=CARTESIAN_POINT('Ctrl Pts',(-0.0033844896763387,-0.00892966491376065,
-0.00134525464698032));
#47778=CARTESIAN_POINT('Ctrl Pts',(-0.0033845085908206,-0.00899757065343684,
-0.00134545168095424));
#47779=CARTESIAN_POINT('Ctrl Pts',(-0.00338450877509932,-0.00899904621982914,
-0.00134545353568596));
#47780=CARTESIAN_POINT('Ctrl Pts',(-0.00338450873183093,-0.00900052178030331,
-0.00134545296373893));
#47781=CARTESIAN_POINT('Origin',(-0.00337226546574067,-0.00900117984349398,
2.58365129269925E-6));
#47782=CARTESIAN_POINT('Origin',(-0.00380975860693448,-0.00899994566615699,
3.48370398817743E-7));
#47783=CARTESIAN_POINT('Origin',(-0.00390975858063242,-0.00900003644744767,
0.0018421052628004));
#47784=CARTESIAN_POINT('',(-0.00390975858063242,-0.00900000344043453,-0.00174210526321707));
#47785=CARTESIAN_POINT('Ctrl Pts',(-0.00390975858063242,-0.00900000344043453,
-0.00174210526321707));
#47786=CARTESIAN_POINT('Ctrl Pts',(-0.00390975858063242,-0.00900010892359971,
-0.0017421052645996));
#47787=CARTESIAN_POINT('Ctrl Pts',(-0.00390975858063242,-0.00900021440675734,
-0.00174210525596106));
#47788=CARTESIAN_POINT('Ctrl Pts',(-0.00390975858063242,-0.0090003198899058,
-0.00174210523730213));
#47789=CARTESIAN_POINT('Ctrl Pts',(-0.00390975858063242,-0.00882510339125232,
-0.00173300347273605));
#47790=CARTESIAN_POINT('Ctrl Pts',(-0.00390975858063242,-0.00888321951194065,
-0.00173903303843893));
#47791=CARTESIAN_POINT('Ctrl Pts',(-0.00390975858063242,-0.00894161263180323,
-0.00174210449790967));
#47792=CARTESIAN_POINT('Ctrl Pts',(-0.00390975858063242,-0.00900000344043453,
-0.00174210526321707));
#47793=CARTESIAN_POINT('',(-0.00390966975442655,-0.00900000000006269,-0.00144210824574401));
#47794=CARTESIAN_POINT('',(-0.00390972476942416,-0.00799782182333048,-0.00104223077880221));
#47795=CARTESIAN_POINT('Ctrl Pts',(-0.00390966975442655,-0.00900000000006269,
-0.00144210824574401));
#47796=CARTESIAN_POINT('Ctrl Pts',(-0.00390966976203054,-0.0088197660211075,
-0.00144211226082542));
#47797=CARTESIAN_POINT('Ctrl Pts',(-0.0039096810567326,-0.00863964557616199,
-0.00140814906199155));
#47798=CARTESIAN_POINT('Ctrl Pts',(-0.00390969855902211,-0.00847221884979575,
-0.00134319471865232));
#47799=CARTESIAN_POINT('Ctrl Pts',(-0.0039097169364261,-0.0082964207871112,
-0.00127499265814613));
#47800=CARTESIAN_POINT('Ctrl Pts',(-0.00390972747686855,-0.00813461712028997,
-0.00117262355290227));
#47801=CARTESIAN_POINT('Ctrl Pts',(-0.00390972476942416,-0.00799782182333048,
-0.00104223077880221));
#47802=CARTESIAN_POINT('',(-0.00390971778425656,-0.00795392388178663,0.000998653228350628));
#47803=CARTESIAN_POINT('Ctrl Pts',(-0.00390972476942416,-0.00799782182333048,
-0.00104223077880221));
#47804=CARTESIAN_POINT('Ctrl Pts',(-0.00390972334479271,-0.00792584144088275,
-0.000973619342906699));
#47805=CARTESIAN_POINT('Ctrl Pts',(-0.00390972041610811,-0.0078607852822472,
-0.000897248810375659));
#47806=CARTESIAN_POINT('Ctrl Pts',(-0.0039097109017685,-0.00780438624911606,
-0.000815607003483071));
#47807=CARTESIAN_POINT('Ctrl Pts',(-0.00390970181578942,-0.00775052644847205,
-0.000737640925000353));
#47808=CARTESIAN_POINT('Ctrl Pts',(-0.00390968635523896,-0.0077045618950396,
-0.000654867542329328));
#47809=CARTESIAN_POINT('Ctrl Pts',(-0.00390967718883946,-0.00766715405430361,
-0.000567866545804131));
#47810=CARTESIAN_POINT('Ctrl Pts',(-0.00390966804404756,-0.00762983439362337,
-0.000481070633362192));
#47811=CARTESIAN_POINT('Ctrl Pts',(-0.00390966311664814,-0.00760103115841473,
-0.00039006693600034));
#47812=CARTESIAN_POINT('Ctrl Pts',(-0.00390965465336911,-0.00758136263727643,
-0.000297447048399321));
#47813=CARTESIAN_POINT('Ctrl Pts',(-0.00390964619108995,-0.00756169643980781,
-0.000204838103055954));
#47814=CARTESIAN_POINT('Ctrl Pts',(-0.00390963640198231,-0.00755116270600896,
-0.00011061345411514));
#47815=CARTESIAN_POINT('Ctrl Pts',(-0.00390963647383203,-0.00755009700252165,
-1.61629646556979E-5));
#47816=CARTESIAN_POINT('Ctrl Pts',(-0.00390963661393813,-0.00754801889331327,
0.000168014373805593));
#47817=CARTESIAN_POINT('Ctrl Pts',(-0.00390965471980009,-0.00758194386574754,
0.000353050874397227));
#47818=CARTESIAN_POINT('Ctrl Pts',(-0.00390967549689029,-0.00764941656405345,
0.000524809084816847));
#47819=CARTESIAN_POINT('Ctrl Pts',(-0.00390969678008587,-0.00771853281760433,
0.000700751122394549));
#47820=CARTESIAN_POINT('Ctrl Pts',(-0.00390971697562406,-0.00782285143124549,
0.000862759747474539));
#47821=CARTESIAN_POINT('Ctrl Pts',(-0.00390971778425656,-0.00795392388178663,
0.000998653228350628));
#47822=CARTESIAN_POINT('',(-0.00390963450991967,-0.00899994572134765,0.00144213270448328));
#47823=CARTESIAN_POINT('Ctrl Pts',(-0.00390971778425656,-0.00795392388178663,
0.000998653228350628));
#47824=CARTESIAN_POINT('Ctrl Pts',(-0.0039097185938505,-0.0080851521746966,
0.00113470828369855));
#47825=CARTESIAN_POINT('Ctrl Pts',(-0.00390970275420778,-0.00824319753023578,
0.00124458635119802));
#47826=CARTESIAN_POINT('Ctrl Pts',(-0.00390967849947921,-0.00841680717529352,
0.00132033545754371));
#47827=CARTESIAN_POINT('Ctrl Pts',(-0.00390965424331042,-0.00859042712900413,
0.00139608906174574));
#47828=CARTESIAN_POINT('Ctrl Pts',(-0.00390963265494929,-0.00877961385322806,
0.00143770908107385));
#47829=CARTESIAN_POINT('Ctrl Pts',(-0.00390963415795286,-0.00896918043380641,
0.00144179524960526));
#47830=CARTESIAN_POINT('Ctrl Pts',(-0.00390963423925692,-0.00897943492210449,
0.00144201628839417));
#47831=CARTESIAN_POINT('Ctrl Pts',(-0.00390963436154657,-0.00898969052073426,
0.00144212749742715));
#47832=CARTESIAN_POINT('Ctrl Pts',(-0.00390963450991967,-0.00899994572134765,
0.00144213270448328));
#47833=CARTESIAN_POINT('',(-0.00390971648405094,-0.0100016923901179,0.00104269314894275));
#47834=CARTESIAN_POINT('Ctrl Pts',(-0.00390963450991967,-0.00899994572134765,
0.00144213270448328));
#47835=CARTESIAN_POINT('Ctrl Pts',(-0.00390963735419761,-0.00917925816624089,
0.00144216106639203));
#47836=CARTESIAN_POINT('Ctrl Pts',(-0.00390965229205243,-0.00935824009674402,
0.00140874375267135));
#47837=CARTESIAN_POINT('Ctrl Pts',(-0.0039096719045267,-0.00952516270713903,
0.00134421182287322));
#47838=CARTESIAN_POINT('Ctrl Pts',(-0.00390969263859743,-0.00970163127318034,
0.00127598944671696));
#47839=CARTESIAN_POINT('Ctrl Pts',(-0.00390971467173984,-0.00986462208441464,
0.00117299239295296));
#47840=CARTESIAN_POINT('Ctrl Pts',(-0.00390971648405094,-0.0100016923901179,
0.00104269314894275));
#47841=CARTESIAN_POINT('',(-0.00390972211041965,-0.0100356073524843,-0.00100937059217969));
#47842=CARTESIAN_POINT('Ctrl Pts',(-0.00390971648405094,-0.0100016923901179,
0.00104269314894275));
#47843=CARTESIAN_POINT('Ctrl Pts',(-0.00390971829636204,-0.0101387626968384,
0.000912393903965479));
#47844=CARTESIAN_POINT('Ctrl Pts',(-0.0039097032843565,-0.0102499122404115,
0.000754792010601407));
#47845=CARTESIAN_POINT('Ctrl Pts',(-0.00390967824347019,-0.0103266137464934,
0.000582152223145582));
#47846=CARTESIAN_POINT('Ctrl Pts',(-0.00390965320258387,-0.0104033152526038,
0.00040951243562569));
#47847=CARTESIAN_POINT('Ctrl Pts',(-0.00390962578534569,-0.0104455689904412,
0.000221835420904369));
#47848=CARTESIAN_POINT('Ctrl Pts',(-0.00390963032251337,-0.0104496430802503,
3.218780127882E-5));
#47849=CARTESIAN_POINT('Ctrl Pts',(-0.0039096327045264,-0.0104517819774001,
-6.73771990263512E-5));
#47850=CARTESIAN_POINT('Ctrl Pts',(-0.00390964227984429,-0.0104433974606173,
-0.000167485522235034));
#47851=CARTESIAN_POINT('Ctrl Pts',(-0.00390964660722069,-0.0104250950124203,
-0.000265163779662066));
#47852=CARTESIAN_POINT('Ctrl Pts',(-0.00390965073883483,-0.0104076205321179,
-0.000358423258777086));
#47853=CARTESIAN_POINT('Ctrl Pts',(-0.00390965575216524,-0.0103811055941798,
-0.000449467563700001));
#47854=CARTESIAN_POINT('Ctrl Pts',(-0.00390966864830771,-0.0103455754734661,
-0.000537349171337576));
#47855=CARTESIAN_POINT('Ctrl Pts',(-0.00390968151389822,-0.0103101295263551,
-0.000625022580652821));
#47856=CARTESIAN_POINT('Ctrl Pts',(-0.00390969647605033,-0.0102657106427814,
-0.000709548144133988));
#47857=CARTESIAN_POINT('Ctrl Pts',(-0.00390970503051356,-0.0102136690684806,
-0.000788793353267544));
#47858=CARTESIAN_POINT('Ctrl Pts',(-0.00390971358396108,-0.0101616336733443,
-0.000868029153208667));
#47859=CARTESIAN_POINT('Ctrl Pts',(-0.00390971891000173,-0.0101019775683224,
-0.000941985919899507));
#47860=CARTESIAN_POINT('Ctrl Pts',(-0.00390972211041965,-0.0100356073524843,
-0.00100937059217969));
#47861=CARTESIAN_POINT('Ctrl Pts',(-0.00390972211041965,-0.0100356073524843,
-0.00100937059217969));
#47862=CARTESIAN_POINT('Ctrl Pts',(-0.0039097283511966,-0.00990618621974132,
-0.00114076990293808));
#47863=CARTESIAN_POINT('Ctrl Pts',(-0.00390971944756646,-0.00975123495878918,
-0.00124717904548944));
#47864=CARTESIAN_POINT('Ctrl Pts',(-0.00390970366359697,-0.00958177451303321,
-0.00132095260090437));
#47865=CARTESIAN_POINT('Ctrl Pts',(-0.00390968664417768,-0.00939904998466667,
-0.00140050059252555));
#47866=CARTESIAN_POINT('Ctrl Pts',(-0.00390966974601161,-0.00919945560991264,
-0.00144210380246136));
#47867=CARTESIAN_POINT('Ctrl Pts',(-0.00390966975442655,-0.00900000000006269,
-0.00144210824574401));
#47868=CARTESIAN_POINT('Origin',(0.,-0.009,-1.22464679914735E-19));
#47869=CARTESIAN_POINT('',(0.,-0.009,0.00125));
#47870=CARTESIAN_POINT('Origin',(0.,-0.009,-1.22464679914735E-19));
#47871=CARTESIAN_POINT('Origin',(-0.004,-0.009,-1.22464679914735E-19));
#47872=CARTESIAN_POINT('',(-0.004,-0.009,0.00125));
#47873=CARTESIAN_POINT('Ctrl Pts',(-0.00326780067323885,-0.00830775851653247,
-0.00103977630810674));
#47874=CARTESIAN_POINT('Ctrl Pts',(-0.00327714277681445,-0.00851186476585222,
-0.00117432822854541));
#47875=CARTESIAN_POINT('Ctrl Pts',(-0.0032846096979276,-0.0087559375999203,
-0.00124998758441102));
#47876=CARTESIAN_POINT('Ctrl Pts',(-0.00328461216640222,-0.00900000000000097,
-0.00124999998094225));
#47877=CARTESIAN_POINT('Ctrl Pts',(-0.00328461215845628,-0.00900048192889801,
-0.00124999990709781));
#47878=CARTESIAN_POINT('Ctrl Pts',(-0.00338400522957233,-0.00900048496365769,
-0.00124999990592778));
#47879=CARTESIAN_POINT('Ctrl Pts',(-0.00338461030538419,-0.00900052330173693,
-0.00134939112791716));
#47880=CARTESIAN_POINT('Ctrl Pts',(-0.00328462200345994,-0.0086739200473581,
-0.00125011657331827));
#47881=CARTESIAN_POINT('Ctrl Pts',(-0.003384013177488,-0.00867517913342947,
-0.00125011489397692));
#47882=CARTESIAN_POINT('Ctrl Pts',(-0.00338462023319443,-0.00864567411161468,
-0.00134951725455865));
#47883=CARTESIAN_POINT('Ctrl Pts',(-0.00325790117155621,-0.00802066659855702,
-0.000979447538677857));
#47884=CARTESIAN_POINT('Ctrl Pts',(-0.00336075013595249,-0.00800482732738064,
-0.000963468404288508));
#47885=CARTESIAN_POINT('Ctrl Pts',(-0.00335780888612222,-0.00793743054808474,
-0.00105840198561949));
#47886=CARTESIAN_POINT('Ctrl Pts',(-0.00321793190913946,-0.0076149676140644,
-1.54083867402206E-6));
#47887=CARTESIAN_POINT('Ctrl Pts',(-0.00332799412930291,-0.00761878655976351,
-1.51388930652299E-6));
#47888=CARTESIAN_POINT('Ctrl Pts',(-0.00331757760893123,-0.00749558137023603,
-1.66483058764779E-6));
#47889=CARTESIAN_POINT('Ctrl Pts',(-0.00325780785275684,-0.008019466089899,
0.000978742800856142));
#47890=CARTESIAN_POINT('Ctrl Pts',(-0.00336067162260847,-0.00800363754489395,
0.000962724449561964));
#47891=CARTESIAN_POINT('Ctrl Pts',(-0.0033577150665097,-0.00793612611646283,
0.0010576437152649));
#47892=CARTESIAN_POINT('Ctrl Pts',(-0.00329800025932114,-0.00899946420378033,
0.00138546387197374));
#47893=CARTESIAN_POINT('Ctrl Pts',(-0.0033953190356324,-0.00899944782531834,
0.00138926904137042));
#47894=CARTESIAN_POINT('Ctrl Pts',(-0.00339807408715874,-0.00899941917617344,
0.00149541593485778));
#47895=CARTESIAN_POINT('Ctrl Pts',(-0.00325786406347626,-0.00997987109426551,
0.000979401186339539));
#47896=CARTESIAN_POINT('Ctrl Pts',(-0.00336071891445555,-0.00999571441285378,
0.000963399852332962));
#47897=CARTESIAN_POINT('Ctrl Pts',(-0.00335777157893346,-0.010063153048397,
0.00105835340798998));
#47898=CARTESIAN_POINT('Ctrl Pts',(-0.00321793255865113,-0.0103850227343342,
-4.38299481707064E-7));
#47899=CARTESIAN_POINT('Ctrl Pts',(-0.00332799471446149,-0.0103812033852223,
-4.47410730017003E-7));
#47900=CARTESIAN_POINT('Ctrl Pts',(-0.00331757825861524,-0.0105044081817788,
-4.72359875001561E-7));
#47901=CARTESIAN_POINT('Ctrl Pts',(-0.00325784210153424,-0.00998003788779652,
-0.000978747541355083));
#47902=CARTESIAN_POINT('Ctrl Pts',(-0.00336070043689,-0.00999586177973733,
-0.00096275163289535));
#47903=CARTESIAN_POINT('Ctrl Pts',(-0.00335774949912804,-0.0100633355839779,
-0.00105764734367712));
#47904=CARTESIAN_POINT('Ctrl Pts',(-0.00328460231345262,-0.00932704381043793,
-0.00124988324087735));
#47905=CARTESIAN_POINT('Ctrl Pts',(-0.00338399728153908,-0.00932579560598706,
-0.00124988491617768));
#47906=CARTESIAN_POINT('Ctrl Pts',(-0.00338460037758513,-0.00935537209178598,
-0.00134926500141788));
#47907=CARTESIAN_POINT('Ctrl Pts',(-0.00328461215845628,-0.00900048192889801,
-0.00124999990709781));
#47908=CARTESIAN_POINT('Ctrl Pts',(-0.00338400522957233,-0.00900048496365769,
-0.00124999990592778));
#47909=CARTESIAN_POINT('Ctrl Pts',(-0.00338461030538419,-0.00900052330173693,
-0.00134939112791716));
#47910=CARTESIAN_POINT('Ctrl Pts',(-0.0035392791351489,-0.00858849912814965,
-0.00179466521288696));
#47911=CARTESIAN_POINT('Ctrl Pts',(-0.00342573153923465,-0.00859176400850957,
-0.00179333404984997));
#47912=CARTESIAN_POINT('Ctrl Pts',(-0.00343811948343117,-0.00856602524158671,
-0.00190328650635992));
#47913=CARTESIAN_POINT('Ctrl Pts',(-0.00355142559943888,-0.00905859136078448,
-0.00190144952999438));
#47914=CARTESIAN_POINT('Ctrl Pts',(-0.00343722171108695,-0.00906840205799737,
-0.00190374929419889));
#47915=CARTESIAN_POINT('Ctrl Pts',(-0.0034503400565124,-0.00906157284819796,
-0.0020166590821151));
#47916=CARTESIAN_POINT('Ctrl Pts',(-0.00352537010396588,-0.0100884377158575,
-0.00172789987787408));
#47917=CARTESIAN_POINT('Ctrl Pts',(-0.0034151603753512,-0.0100497091309754,
-0.00174559426658833));
#47918=CARTESIAN_POINT('Ctrl Pts',(-0.00342416641781692,-0.0101460057925454,
-0.00183316467220812));
#47919=CARTESIAN_POINT('Ctrl Pts',(-0.00341335748290235,-0.0109970962519671,
-0.000457281663563109));
#47920=CARTESIAN_POINT('Ctrl Pts',(-0.00331425963473675,-0.010996887331939,
-0.000476856829642387));
#47921=CARTESIAN_POINT('Ctrl Pts',(-0.0033115684832145,-0.0111050748119872,
-0.000486036946141634));
#47922=CARTESIAN_POINT('Ctrl Pts',(-0.00345233946123927,-0.0107338060170907,
0.00108652455487473));
#47923=CARTESIAN_POINT('Ctrl Pts',(-0.00335032457735252,-0.0107129565277369,
0.00112100474052161));
#47924=CARTESIAN_POINT('Ctrl Pts',(-0.00335076613415529,-0.0108274712600009,
0.00115282043607336));
#47925=CARTESIAN_POINT('Ctrl Pts',(-0.00356449374860163,-0.00945621932640169,
0.00198829625682747));
#47926=CARTESIAN_POINT('Ctrl Pts',(-0.00344854884364189,-0.00943365667565594,
0.00198475236629158));
#47927=CARTESIAN_POINT('Ctrl Pts',(-0.0034634722557383,-0.00948068538942303,
0.00210854197031486));
#47928=CARTESIAN_POINT('Ctrl Pts',(-0.00352531374816938,-0.00791032423527775,
0.00172792526671951));
#47929=CARTESIAN_POINT('Ctrl Pts',(-0.00341511348123987,-0.00794907951679388,
0.00174568140804206));
#47930=CARTESIAN_POINT('Ctrl Pts',(-0.00342410980697788,-0.0078526998577211,
0.00183315731298699));
#47931=CARTESIAN_POINT('Ctrl Pts',(-0.00341328178572483,-0.00700287546046352,
0.000454633913679566));
#47932=CARTESIAN_POINT('Ctrl Pts',(-0.00331419107940177,-0.00700305969526376,
0.000474177195847323));
#47933=CARTESIAN_POINT('Ctrl Pts',(-0.00331149240063511,-0.00689487285927746,
0.000483300740605997));
#47934=CARTESIAN_POINT('Ctrl Pts',(-0.00345241595160808,-0.00726632486312327,
-0.00108656836792835));
#47935=CARTESIAN_POINT('Ctrl Pts',(-0.00335038976344317,-0.00728717254733531,
-0.00112102914438496));
#47936=CARTESIAN_POINT('Ctrl Pts',(-0.00335084297932956,-0.00717272015287796,
-0.00115292921767708));
#47937=CARTESIAN_POINT('Ctrl Pts',(-0.00352712997637068,-0.00811830261348138,
-0.00168785720747976));
#47938=CARTESIAN_POINT('Ctrl Pts',(-0.00341440081056064,-0.00812174001897434,
-0.00168445098079964));
#47939=CARTESIAN_POINT('Ctrl Pts',(-0.00342589891034995,-0.00807047763497546,
-0.00178991393060475));
#47940=CARTESIAN_POINT('Ctrl Pts',(-0.0035392791351489,-0.00858849912814965,
-0.00179466521288696));
#47941=CARTESIAN_POINT('Ctrl Pts',(-0.00342573153923465,-0.00859176400850957,
-0.00179333404984997));
#47942=CARTESIAN_POINT('Ctrl Pts',(-0.00343811948343117,-0.00856602524158671,
-0.00190328650635992));
#47943=CARTESIAN_POINT('Origin',(-0.00380969939533716,-0.00899994566562597,
3.48367311799158E-7));
#47944=CARTESIAN_POINT('Origin',(-0.00380969419167622,-0.00899994566562597,
0.00144616158862221));
#47945=CARTESIAN_POINT('Ctrl Pts',(-0.00380975858063242,-0.00881478413029403,
-0.00183246684420301));
#47946=CARTESIAN_POINT('Ctrl Pts',(-0.00390993294014545,-0.00881478413029403,
-0.00183246684420301));
#47947=CARTESIAN_POINT('Ctrl Pts',(-0.00390975842889103,-0.00882512165273333,
-0.00173282745701358));
#47948=CARTESIAN_POINT('Ctrl Pts',(-0.00380975858063242,-0.00929465142715738,
-0.0018806998537358));
#47949=CARTESIAN_POINT('Ctrl Pts',(-0.00390993294014545,-0.00929465142715738,
-0.0018806998537358));
#47950=CARTESIAN_POINT('Ctrl Pts',(-0.00390975842889103,-0.00927906675289324,
-0.00177836203380147));
#47951=CARTESIAN_POINT('Ctrl Pts',(-0.00380975858063242,-0.0102936387094841,
-0.00158253456509613));
#47952=CARTESIAN_POINT('Ctrl Pts',(-0.00390993294014546,-0.0102936387094841,
-0.00158253456509614));
#47953=CARTESIAN_POINT('Ctrl Pts',(-0.00390975842889104,-0.0102241270617854,
-0.00149607241763065));
#47954=CARTESIAN_POINT('Ctrl Pts',(-0.00380975858063242,-0.0110403459009329,
-0.000207601983482724));
#47955=CARTESIAN_POINT('Ctrl Pts',(-0.00390993294014544,-0.0110403459009329,
-0.000207601983482722));
#47956=CARTESIAN_POINT('Ctrl Pts',(-0.00390975842889102,-0.0109298209858678,
-0.00019577210929604));
#47957=CARTESIAN_POINT('Ctrl Pts',(-0.00380975858063243,-0.010585488822892,
0.00129440175744357));
#47958=CARTESIAN_POINT('Ctrl Pts',(-0.00390993294014546,-0.010585488822892,
0.00129440175744357));
#47959=CARTESIAN_POINT('Ctrl Pts',(-0.00390975842889104,-0.0104994209642949,
0.0012241417666484));
#47960=CARTESIAN_POINT('Ctrl Pts',(-0.00380975858063242,-0.00920314460986179,
0.00202990873817867));
#47961=CARTESIAN_POINT('Ctrl Pts',(-0.00390993294014544,-0.00920314460986179,
0.00202990873817867));
#47962=CARTESIAN_POINT('Ctrl Pts',(-0.00390975842889102,-0.00919187984963056,
0.00191958960744435));
#47963=CARTESIAN_POINT('Ctrl Pts',(-0.00380975858063242,-0.00770446035061261,
0.0015817160659287));
#47964=CARTESIAN_POINT('Ctrl Pts',(-0.00390993294014545,-0.00770446035061261,
0.0015817160659287));
#47965=CARTESIAN_POINT('Ctrl Pts',(-0.00390975842889103,-0.00777409310458325,
0.00149536140507255));
#47966=CARTESIAN_POINT('Ctrl Pts',(-0.00380975858063242,-0.00695993177951074,
0.000203870131802003));
#47967=CARTESIAN_POINT('Ctrl Pts',(-0.00390993294014545,-0.00695993177951073,
0.000203870131802006));
#47968=CARTESIAN_POINT('Ctrl Pts',(-0.00390975842889103,-0.00707045087524681,
0.000192132115288156));
#47969=CARTESIAN_POINT('Ctrl Pts',(-0.00380975858063242,-0.00741443492830406,
-0.00129313650789938));
#47970=CARTESIAN_POINT('Ctrl Pts',(-0.00390993294014545,-0.00741443492830407,
-0.00129313650789939));
#47971=CARTESIAN_POINT('Ctrl Pts',(-0.00390975842889103,-0.00750045646082591,
-0.00122286495690331));
#47972=CARTESIAN_POINT('Ctrl Pts',(-0.00380975858063242,-0.00833491683343068,
-0.00178423383467021));
#47973=CARTESIAN_POINT('Ctrl Pts',(-0.00390993294014545,-0.00833491683343068,
-0.00178423383467021));
#47974=CARTESIAN_POINT('Ctrl Pts',(-0.00390975842889103,-0.00837117655257341,
-0.00168729288022569));
#47975=CARTESIAN_POINT('Ctrl Pts',(-0.00380975858063242,-0.00881478413029403,
-0.00183246684420301));
#47976=CARTESIAN_POINT('Ctrl Pts',(-0.00390993294014545,-0.00881478413029403,
-0.00183246684420301));
#47977=CARTESIAN_POINT('Ctrl Pts',(-0.00390975842889103,-0.00882512165273333,
-0.00173282745701358));
#47978=CARTESIAN_POINT('Origin',(1.66533453693773E-18,-0.0144,0.));
#47979=CARTESIAN_POINT('Origin',(-0.00106635989804114,-0.0144,-1.30591423587518E-19));
#47980=CARTESIAN_POINT('Origin',(1.75785312232316E-18,-0.0152,0.));
#47981=CARTESIAN_POINT('Origin',(-0.00126635989804114,-0.0152,-1.55084359570465E-19));
#47982=CARTESIAN_POINT('Origin',(-1.86727542905182E-18,0.014,0.));
#47983=CARTESIAN_POINT('Origin',(0.0045,0.014,-5.51091059616309E-19));
#47984=CARTESIAN_POINT('',(0.,0.,0.));
#47985=CARTESIAN_POINT('Origin',(0.00625,0.013,-2.29621274840129E-18));
#47986=CARTESIAN_POINT('',(0.00310513229246118,0.013,0.00782534372202691));
#47987=CARTESIAN_POINT('',(0.00283397885998211,0.013,0.00748782871937848));
#47988=CARTESIAN_POINT('',(0.000517972272646041,0.013,0.00460500712899027));
#47989=CARTESIAN_POINT('',(0.00343760106241995,0.013,0.00640851728792926));
#47990=CARTESIAN_POINT('',(0.00683781203254235,0.013,0.000328743292588178));
#47991=CARTESIAN_POINT('',(0.00334867942190192,0.013,0.00628088369661617));
#47992=CARTESIAN_POINT('',(0.00135080799850545,0.013,0.00341324086789248));
#47993=CARTESIAN_POINT('',(0.00212708576461598,0.013,0.00647319039387763));
#47994=CARTESIAN_POINT('',(0.00714468201094909,0.013,0.00568330633008214));
#47995=CARTESIAN_POINT('',(0.00190441615676979,0.013,0.00610189696988579));
#47996=CARTESIAN_POINT('',(0.00036250172514288,0.013,0.00353081107110126));
#47997=CARTESIAN_POINT('',(0.00264938241039218,0.013,0.00511483151597876));
#47998=CARTESIAN_POINT('',(0.00641544862510175,0.013,0.000124868763181971));
#47999=CARTESIAN_POINT('',(0.00257866842927369,0.013,0.00497627854900125));
#48000=CARTESIAN_POINT('',(0.00132244326030609,0.013,0.0025149021479097));
#48001=CARTESIAN_POINT('',(0.00139305626828131,0.013,0.00499946069925261));
#48002=CARTESIAN_POINT('',(0.00634586039595321,0.013,0.00490261903953383));
#48003=CARTESIAN_POINT('',(-0.00848709681638249,0.013,0.00183103613732295));
#48004=CARTESIAN_POINT('',(0.00434333886907659,0.013,0.00594557436539644));
#48005=CARTESIAN_POINT('',(-0.00853149850581388,0.013,0.00181051559890248));
#48006=CARTESIAN_POINT('Origin',(-0.00842602321036556,0.013,0.00164058925588855));
#48007=CARTESIAN_POINT('',(-0.00804781744366059,0.013,0.00368315161531047));
#48008=CARTESIAN_POINT('Origin',(-0.00926982557395217,0.013,0.003));
#48009=CARTESIAN_POINT('',(-0.00778675335060335,0.013,0.00360041384088911));
#48010=CARTESIAN_POINT('Origin',(-0.00787324485361894,0.013,0.00378074470321196));
#48011=CARTESIAN_POINT('',(4.52079337442143E-5,0.013,0.00735683187337399));
#48012=CARTESIAN_POINT('',(0.00222095414696891,0.013,0.00840037792943047));
#48013=CARTESIAN_POINT('',(0.00400212262074066,0.013,0.00858487618139458));
#48014=CARTESIAN_POINT('',(0.0036222395132741,0.013,0.00846697793876363));
#48015=CARTESIAN_POINT('',(0.00439463505993757,0.013,0.00758282450818601));
#48016=CARTESIAN_POINT('',(0.00721658525161907,0.013,0.000378619930437244));
#48017=CARTESIAN_POINT('',(0.00428916220193663,0.013,0.00746848786485147));
#48018=CARTESIAN_POINT('',(0.00146851978854034,0.013,0.00441080277214348));
#48019=CARTESIAN_POINT('',(0.00815021035144082,0.013,0.00630480303226358));
#48020=CARTESIAN_POINT('',(-0.00926982557395217,0.013,0.0024));
#48021=CARTESIAN_POINT('Origin',(-0.00926982557395217,0.013,0.003));
#48022=CARTESIAN_POINT('Origin',(-0.00926982557395217,0.001,0.003));
#48023=CARTESIAN_POINT('',(-0.00848709681638249,0.001,0.00183103613732295));
#48024=CARTESIAN_POINT('',(0.00139305626828131,0.001,0.00499946069925261));
#48025=CARTESIAN_POINT('',(-0.00885692281820857,0.001,0.001712438198831));
#48026=CARTESIAN_POINT('',(0.00257866842927369,0.001,0.00497627854900125));
#48027=CARTESIAN_POINT('',(-0.00922667024031924,0.001,0.0052071070980081));
#48028=CARTESIAN_POINT('',(0.00264938241039218,0.001,0.00511483151597876));
#48029=CARTESIAN_POINT('',(-0.000670064127940984,0.001,-0.00138910390576812));
#48030=CARTESIAN_POINT('',(0.00190441615676979,0.001,0.00610189696988579));
#48031=CARTESIAN_POINT('',(-0.000659221951814677,0.001,0.00949866642219173));
#48032=CARTESIAN_POINT('',(0.00212708576461598,0.001,0.00647319039387763));
#48033=CARTESIAN_POINT('',(-0.00241956898424355,0.001,-0.00110819004569721));
#48034=CARTESIAN_POINT('',(0.00334867942190192,0.001,0.00628088369661617));
#48035=CARTESIAN_POINT('',(-0.00846068082425976,0.001,0.0081399462843802));
#48036=CARTESIAN_POINT('',(0.00343760106241995,0.001,0.00640851728792926));
#48037=CARTESIAN_POINT('',(-0.0023135538114868,0.001,-0.00184639733665676));
#48038=CARTESIAN_POINT('',(0.00283397885998211,0.001,0.00748782871937848));
#48039=CARTESIAN_POINT('',(0.00186205600079768,0.001,0.00922568303979271));
#48040=CARTESIAN_POINT('',(0.00310513229246119,0.001,0.00782534372202692));
#48041=CARTESIAN_POINT('',(-0.0041049730035732,0.001,-0.00114934889328565));
#48042=CARTESIAN_POINT('',(0.00428916220193663,0.001,0.00746848786485147));
#48043=CARTESIAN_POINT('',(-0.0069061235431728,0.001,0.0108426452733117));
#48044=CARTESIAN_POINT('',(0.00439463505993757,0.001,0.00758282450818601));
#48045=CARTESIAN_POINT('',(-0.00417144472326108,0.001,-0.00170313614093291));
#48046=CARTESIAN_POINT('',(0.00400212262074066,0.001,0.00858487618139458));
#48047=CARTESIAN_POINT('',(0.00413325559518032,0.001,0.00825010458353409));
#48048=CARTESIAN_POINT('',(4.52079337442122E-5,0.001,0.00735683187337399));
#48049=CARTESIAN_POINT('',(-0.00968479566385333,0.001,0.00433708631901139));
#48050=CARTESIAN_POINT('',(-0.00778675335060335,0.001,0.00360041384088911));
#48051=CARTESIAN_POINT('',(-0.00922657982244437,0.001,0.00290983456883857));
#48052=CARTESIAN_POINT('',(-0.00804781744366059,0.001,0.00368315161531047));
#48053=CARTESIAN_POINT('Origin',(-0.00787324485361894,0.001,0.00378074470321196));
#48054=CARTESIAN_POINT('',(-0.00853149850581388,0.001,0.00181051559890248));
#48055=CARTESIAN_POINT('Origin',(-0.00926982557395217,0.001,0.003));
#48056=CARTESIAN_POINT('Origin',(-0.00842602321036556,0.001,0.00164058925588855));
#48057=CARTESIAN_POINT('',(-0.00926982557395217,0.001,0.0036));
#48058=CARTESIAN_POINT('Origin',(-0.00926982557395217,0.001,0.003));
#48059=CARTESIAN_POINT('Origin',(0.00217815846891078,0.0298951219150416,
0.00636391887181847));
#48060=CARTESIAN_POINT('',(0.00339495317277858,0.0129,0.00617236763925401));
#48061=CARTESIAN_POINT('',(0.00339495317277858,0.0011,0.00617236763925401));
#48062=CARTESIAN_POINT('',(0.00339495317277858,0.0298951219150416,0.00617236763925401));
#48063=CARTESIAN_POINT('',(0.00217815846891078,0.0011,0.00636391887181847));
#48064=CARTESIAN_POINT('',(0.00217815846891078,0.0011,0.00636391887181847));
#48065=CARTESIAN_POINT('',(0.00217815846891078,0.0129,0.00636391887181847));
#48066=CARTESIAN_POINT('',(0.00217815846891078,0.0298951219150416,0.00636391887181847));
#48067=CARTESIAN_POINT('',(0.00217815846891078,0.0129,0.00636391887181847));
#48068=CARTESIAN_POINT('Origin',(0.00339495317277858,0.0298951219150416,
0.00617236763925401));
#48069=CARTESIAN_POINT('',(0.00355542811483384,0.0129,0.00640270519320544));
#48070=CARTESIAN_POINT('',(0.00355542811483384,0.0011,0.00640270519320544));
#48071=CARTESIAN_POINT('',(0.00355542811483384,0.0298951219150416,0.00640270519320544));
#48072=CARTESIAN_POINT('',(0.00339495317277858,0.0011,0.00617236763925401));
#48073=CARTESIAN_POINT('',(0.00339495317277858,0.0129,0.00617236763925401));
#48074=CARTESIAN_POINT('Origin',(0.00355542811483384,0.0298951219150416,
0.00640270519320544));
#48075=CARTESIAN_POINT('',(0.00295417720403981,0.0129,0.00747777661796151));
#48076=CARTESIAN_POINT('',(0.00295417720403981,0.0011,0.00747777661796151));
#48077=CARTESIAN_POINT('',(0.00295417720403981,0.0298951219150416,0.00747777661796151));
#48078=CARTESIAN_POINT('',(0.00355542811483384,0.0011,0.00640270519320544));
#48079=CARTESIAN_POINT('',(0.00355542811483384,0.0129,0.00640270519320544));
#48080=CARTESIAN_POINT('Origin',(0.00295417720403981,0.0298951219150416,
0.00747777661796151));
#48081=CARTESIAN_POINT('',(0.00314085016583167,0.0129,0.0077101355618168));
#48082=CARTESIAN_POINT('',(0.00314085016583167,0.0011,0.0077101355618168));
#48083=CARTESIAN_POINT('',(0.00314085016583167,0.0298951219150416,0.0077101355618168));
#48084=CARTESIAN_POINT('',(0.00295417720403981,0.0011,0.00747777661796151));
#48085=CARTESIAN_POINT('',(0.00295417720403981,0.0129,0.00747777661796151));
#48086=CARTESIAN_POINT('Origin',(0.00314085016583167,0.0298951219150416,
0.0077101355618168));
#48087=CARTESIAN_POINT('',(0.00432022868869639,0.0129,0.00735468159030551));
#48088=CARTESIAN_POINT('',(0.00432022868869639,0.0011,0.00735468159030551));
#48089=CARTESIAN_POINT('',(0.00432022868869639,0.0298951219150416,0.00735468159030551));
#48090=CARTESIAN_POINT('',(0.00314085016583167,0.0011,0.0077101355618168));
#48091=CARTESIAN_POINT('',(0.00314085016583167,0.0129,0.0077101355618168));
#48092=CARTESIAN_POINT('Origin',(0.00432022868869639,0.0298951219150416,
0.00735468159030551));
#48093=CARTESIAN_POINT('',(0.00451057325136412,0.0129,0.007561022432726));
#48094=CARTESIAN_POINT('',(0.00451057325136412,0.0011,0.007561022432726));
#48095=CARTESIAN_POINT('',(0.00451057325136412,0.0298951219150416,0.007561022432726));
#48096=CARTESIAN_POINT('',(0.00432022868869639,0.0011,0.00735468159030551));
#48097=CARTESIAN_POINT('',(0.00432022868869639,0.0129,0.00735468159030551));
#48098=CARTESIAN_POINT('Origin',(0.00451057325136412,0.0298951219150416,
0.007561022432726));
#48099=CARTESIAN_POINT('',(0.0040613112974471,0.0129,0.00870795090600599));
#48100=CARTESIAN_POINT('',(0.0040613112974471,0.0011,0.00870795090600599));
#48101=CARTESIAN_POINT('',(0.0040613112974471,0.0298951219150416,0.00870795090600599));
#48102=CARTESIAN_POINT('',(0.00451057325136412,0.0011,0.007561022432726));
#48103=CARTESIAN_POINT('',(0.00451057325136412,0.0129,0.007561022432726));
#48104=CARTESIAN_POINT('Origin',(0.0040613112974471,0.0298951219150416,
0.00870795090600599));
#48105=CARTESIAN_POINT('',(8.56902727468245E-6,0.0129,0.00745016612406076));
#48106=CARTESIAN_POINT('',(8.56902727468245E-6,0.0011,0.00745016612406076));
#48107=CARTESIAN_POINT('',(8.56902727468245E-6,0.0298951219150416,0.00745016612406076));
#48108=CARTESIAN_POINT('',(0.0040613112974471,0.0011,0.00870795090600599));
#48109=CARTESIAN_POINT('',(0.0040613112974471,0.0129,0.00870795090600599));
#48110=CARTESIAN_POINT('Origin',(8.56902727468245E-6,0.0298951219150416,
0.00745016612406076));
#48111=CARTESIAN_POINT('',(-0.00782999910211115,0.0129,0.00369057927205054));
#48112=CARTESIAN_POINT('',(-0.00782999910211115,0.0011,0.00369057927205054));
#48113=CARTESIAN_POINT('',(-0.00782999910211115,0.001,0.00369057927205053));
#48114=CARTESIAN_POINT('',(8.56902727468245E-6,0.0011,0.00745016612406076));
#48115=CARTESIAN_POINT('',(8.56902727468245E-6,0.0129,0.00745016612406076));
#48116=CARTESIAN_POINT('Origin',(-0.00926982557395217,0.0298951219150416,
0.003));
#48117=CARTESIAN_POINT('',(-0.00847876085808972,0.0129,0.00172555242739552));
#48118=CARTESIAN_POINT('',(-0.00847876085808972,0.0011,0.00172555242739552));
#48119=CARTESIAN_POINT('',(-0.00847876085808972,0.0298951219150416,0.00172555242739552));
#48120=CARTESIAN_POINT('',(-0.00796053114863977,0.0011,0.00373194815926121));
#48121=CARTESIAN_POINT('Origin',(-0.00926982557395217,0.0011,0.003));
#48122=CARTESIAN_POINT('',(-0.00796053114863977,0.0129,0.00373194815926121));
#48123=CARTESIAN_POINT('',(-0.00796053114863977,0.0298951219150416,0.00373194815926121));
#48124=CARTESIAN_POINT('Origin',(-0.00926982557395217,0.0129,0.003));
#48125=CARTESIAN_POINT('Origin',(-0.00846848477354713,0.0298951219150416,
0.00173198859563243));
#48126=CARTESIAN_POINT('',(0.0014077431500399,0.0129,0.00489915441423508));
#48127=CARTESIAN_POINT('',(0.0014077431500399,0.0011,0.00489915441423508));
#48128=CARTESIAN_POINT('',(0.0014077431500399,0.0298951219150416,0.00489915441423508));
#48129=CARTESIAN_POINT('',(-0.00845656001337402,0.0011,0.00173581269660575));
#48130=CARTESIAN_POINT('',(-0.00846848477354713,0.0011,0.00173198859563243));
#48131=CARTESIAN_POINT('',(-0.00845656001337402,0.0129,0.00173581269660575));
#48132=CARTESIAN_POINT('',(-0.00845656001337402,0.013,0.00173581269660575));
#48133=CARTESIAN_POINT('',(-0.00846848477354713,0.0129,0.00173198859563243));
#48134=CARTESIAN_POINT('Origin',(0.0014077431500399,0.0298951219150416,
0.00489915441423508));
#48135=CARTESIAN_POINT('',(0.00263928745184173,0.0129,0.00487507415765127));
#48136=CARTESIAN_POINT('',(0.00263928745184173,0.0011,0.00487507415765127));
#48137=CARTESIAN_POINT('',(0.00263928745184173,0.0298951219150416,0.00487507415765127));
#48138=CARTESIAN_POINT('',(0.0014077431500399,0.0011,0.00489915441423508));
#48139=CARTESIAN_POINT('',(0.0014077431500399,0.0129,0.00489915441423508));
#48140=CARTESIAN_POINT('Origin',(0.00263928745184173,0.0298951219150416,
0.00487507415765127));
#48141=CARTESIAN_POINT('',(0.00276690342874427,0.0129,0.00512511767031892));
#48142=CARTESIAN_POINT('',(0.00276690342874427,0.0011,0.00512511767031892));
#48143=CARTESIAN_POINT('',(0.00276690342874427,0.0298951219150416,0.00512511767031892));
#48144=CARTESIAN_POINT('',(0.00263928745184173,0.0011,0.00487507415765127));
#48145=CARTESIAN_POINT('',(0.00263928745184173,0.0129,0.00487507415765127));
#48146=CARTESIAN_POINT('Origin',(0.00276690342874427,0.0298951219150416,
0.00512511767031892));
#48147=CARTESIAN_POINT('',(0.00202486372793092,0.0129,0.00610830550002113));
#48148=CARTESIAN_POINT('',(0.00202486372793092,0.0011,0.00610830550002113));
#48149=CARTESIAN_POINT('',(0.00202486372793092,0.0298951219150416,0.00610830550002113));
#48150=CARTESIAN_POINT('',(0.00276690342874427,0.0011,0.00512511767031892));
#48151=CARTESIAN_POINT('',(0.00276690342874427,0.0129,0.00512511767031892));
#48152=CARTESIAN_POINT('Origin',(0.00202486372793092,0.0298951219150416,
0.00610830550002113));
#48153=CARTESIAN_POINT('',(0.00202486372793092,0.0011,0.00610830550002113));
#48154=CARTESIAN_POINT('',(0.00202486372793092,0.0129,0.00610830550002113));
#48155=CARTESIAN_POINT('Origin',(-0.00926982557395217,0.0172006855706717,
0.003));
#48156=CARTESIAN_POINT('',(-0.00926982557395217,0.0129,0.0035));
#48157=CARTESIAN_POINT('',(-0.00926982557395217,0.0129,0.0025));
#48158=CARTESIAN_POINT('Origin',(-0.00926982557395217,0.0129,0.003));
#48159=CARTESIAN_POINT('Origin',(-0.00926982557395217,0.0129,0.003));
#48160=CARTESIAN_POINT('',(-0.00926982557395217,0.0011,0.0035));
#48161=CARTESIAN_POINT('',(-0.00926982557395217,0.0172006855706717,0.0035));
#48162=CARTESIAN_POINT('Origin',(-0.00926982557395217,0.0011,0.003));
#48163=CARTESIAN_POINT('Origin',(0.00346815021717762,0.0129,0.00635389363124816));
#48164=CARTESIAN_POINT('Origin',(0.00343760106241995,0.0129,0.00640851728792926));
#48165=CARTESIAN_POINT('Origin',(0.00283397885998211,0.0129,0.00748782871937848));
#48166=CARTESIAN_POINT('Origin',(0.00287621909532571,0.0129,0.00754040674877505));
#48167=CARTESIAN_POINT('Origin',(0.00310513229246118,0.0129,0.00782534372202691));
#48168=CARTESIAN_POINT('Origin',(-0.0041049730035732,0.0011,-0.00114934889328566));
#48169=CARTESIAN_POINT('Origin',(0.00310513229246118,0.0011,0.00782534372202692));
#48170=CARTESIAN_POINT('Origin',(0.00283397885998211,0.0011,0.00748782871937847));
#48171=CARTESIAN_POINT('Origin',(0.00186205600079768,0.0011,0.00922568303979271));
#48172=CARTESIAN_POINT('Origin',(0.00343760106241995,0.0011,0.00640851728792926));
#48173=CARTESIAN_POINT('Origin',(0.00331290277113331,0.0129,0.006229531715297));
#48174=CARTESIAN_POINT('Origin',(0.00334867942190192,0.0129,0.00628088369661617));
#48175=CARTESIAN_POINT('Origin',(0.00316970710931718,0.0129,0.00780588145892302));
#48176=CARTESIAN_POINT('Origin',(0.00428916220193663,0.0129,0.00746848786485147));
#48177=CARTESIAN_POINT('Origin',(-0.0069061235431728,0.0011,0.0108426452733117));
#48178=CARTESIAN_POINT('Origin',(0.00428916220193663,0.0011,0.00746848786485147));
#48179=CARTESIAN_POINT('Origin',(-0.0023135538114868,0.0011,-0.00184639733665676));
#48180=CARTESIAN_POINT('Origin',(0.00334867942190192,0.0011,0.00628088369661617));
#48181=CARTESIAN_POINT('Origin',(0.00219370923929376,0.0129,0.00646270233976982));
#48182=CARTESIAN_POINT('Origin',(0.00212708576461598,0.0129,0.00647319039387763));
#48183=CARTESIAN_POINT('Origin',(0.00424672634960323,0.0129,0.00742248576530849));
#48184=CARTESIAN_POINT('Origin',(0.00439463505993757,0.0129,0.00758282450818601));
#48185=CARTESIAN_POINT('Origin',(-0.00417144472326108,0.0011,-0.00170313614093291));
#48186=CARTESIAN_POINT('Origin',(0.00439463505993757,0.0011,0.00758282450818601));
#48187=CARTESIAN_POINT('Origin',(-0.00846068082425976,0.0011,0.0081399462843802));
#48188=CARTESIAN_POINT('Origin',(0.00212708576461597,0.0011,0.00647319039387763));
#48189=CARTESIAN_POINT('Origin',(0.00193910359020296,0.0129,0.00615973699598304));
#48190=CARTESIAN_POINT('Origin',(0.00190441615676979,0.0129,0.00610189696988579));
#48191=CARTESIAN_POINT('Origin',(0.00441746175792763,0.0129,0.00752454984315485));
#48192=CARTESIAN_POINT('Origin',(0.00400212262074066,0.0129,0.00858487618139458));
#48193=CARTESIAN_POINT('Origin',(0.00413325559518032,0.0011,0.00825010458353409));
#48194=CARTESIAN_POINT('Origin',(0.00400212262074067,0.0011,0.00858487618139459));
#48195=CARTESIAN_POINT('Origin',(-0.00241956898424355,0.0011,-0.00110819004569721));
#48196=CARTESIAN_POINT('Origin',(0.00190441615676979,0.0011,0.00610189696988579));
#48197=CARTESIAN_POINT('Origin',(0.00268708494896553,0.0129,0.00506487640301974));
#48198=CARTESIAN_POINT('Origin',(0.00264938241039218,0.0129,0.00511483151597876));
#48199=CARTESIAN_POINT('Origin',(0.00409095201815432,0.0129,0.00861244474036231));
#48200=CARTESIAN_POINT('Origin',(4.52079337441844E-5,0.0129,0.00735683187337397));
#48201=CARTESIAN_POINT('Origin',(-0.00968479566385333,0.0011,0.00433708631901139));
#48202=CARTESIAN_POINT('Origin',(4.5207933744215E-5,0.0011,0.00735683187337399));
#48203=CARTESIAN_POINT('Origin',(-0.000659221951814679,0.0011,0.00949866642219173));
#48204=CARTESIAN_POINT('Origin',(0.00264938241039218,0.0011,0.00511483151597876));
#48205=CARTESIAN_POINT('Origin',(0.00255021743138166,0.0129,0.00492053327615618));
#48206=CARTESIAN_POINT('Origin',(0.00257866842927369,0.0129,0.00497627854900125));
#48207=CARTESIAN_POINT('Origin',(5.18147787824767E-5,0.0129,0.00736000069289933));
#48208=CARTESIAN_POINT('Origin',(-0.00778675335060335,0.0129,0.00360041384088911));
#48209=CARTESIAN_POINT('Origin',(-0.00787324485361894,0.0298951219150416,
0.00378074470321196));
#48210=CARTESIAN_POINT('Origin',(-0.00787324485361894,0.0011,0.00378074470321196));
#48211=CARTESIAN_POINT('Origin',(-0.00787324485361894,0.0129,0.00378074470321196));
#48212=CARTESIAN_POINT('Origin',(-0.00922657982244437,0.0011,0.00290983456883857));
#48213=CARTESIAN_POINT('Origin',(-0.00778675335060335,0.0011,0.00360041384088911));
#48214=CARTESIAN_POINT('Origin',(-0.000670064127940984,0.0011,-0.00138910390576812));
#48215=CARTESIAN_POINT('Origin',(0.00257866842927369,0.0011,0.00497627854900125));
#48216=CARTESIAN_POINT('Origin',(0.00140969806589131,0.0129,0.00499913530392913));
#48217=CARTESIAN_POINT('Origin',(0.00139305626828132,0.0129,0.00499946069925261));
#48218=CARTESIAN_POINT('Origin',(-0.00787324485361894,0.0129,0.00378074470321196));
#48219=CARTESIAN_POINT('Origin',(-0.00804781744366059,0.0129,0.00368315161531047));
#48220=CARTESIAN_POINT('Origin',(-0.00787324485361894,0.0011,0.00378074470321196));
#48221=CARTESIAN_POINT('Origin',(-0.00804781744366059,0.0011,0.00368315161531047));
#48222=CARTESIAN_POINT('Origin',(-0.00922667024031924,0.0011,0.0052071070980081));
#48223=CARTESIAN_POINT('Origin',(0.00139305626828131,0.0011,0.00499946069925261));
#48224=CARTESIAN_POINT('Origin',(-0.0084990215765556,0.0129,0.00182721203634963));
#48225=CARTESIAN_POINT('Origin',(-0.00848709681638249,0.0129,0.00183103613732295));
#48226=CARTESIAN_POINT('Origin',(-0.00926982557395217,0.0129,0.003));
#48227=CARTESIAN_POINT('Origin',(-0.00853149850581388,0.0129,0.00181051559890248));
#48228=CARTESIAN_POINT('Origin',(-0.00926982557395217,0.0011,0.003));
#48229=CARTESIAN_POINT('Origin',(-0.00853149850581388,0.0011,0.00181051559890248));
#48230=CARTESIAN_POINT('Origin',(-0.00885692281820857,0.0011,0.001712438198831));
#48231=CARTESIAN_POINT('Origin',(-0.00848709681638249,0.0011,0.00183103613732295));
#48232=CARTESIAN_POINT('Origin',(-0.00842602321036556,0.0129,0.00164058925588855));
#48233=CARTESIAN_POINT('Origin',(-0.00842602321036556,0.0129,0.00164058925588855));
#48234=CARTESIAN_POINT('Origin',(-0.00842602321036556,0.0011,0.00164058925588855));
#48235=CARTESIAN_POINT('Origin',(-0.00842602321036556,0.0011,0.00164058925588855));
#48236=CARTESIAN_POINT('Origin',(-0.00842602321036556,0.0298951219150416,
0.00164058925588855));
#48237=CARTESIAN_POINT('Origin',(-0.00926982557395217,0.0011,0.003));
#48238=CARTESIAN_POINT('Origin',(-0.00926982557395217,0.0011,0.0036));
#48239=CARTESIAN_POINT('Origin',(-0.00926982557395217,0.0129,0.003));
#48240=CARTESIAN_POINT('Origin',(-0.00926982557395217,0.0129,0.0024));
#48241=CARTESIAN_POINT('',(0.,0.,0.));
#48242=CARTESIAN_POINT('Origin',(-0.00926982557395217,-0.0158951219150417,
-0.003));
#48243=CARTESIAN_POINT('',(-0.00796053114863977,0.0129,-0.00373194815926121));
#48244=CARTESIAN_POINT('',(-0.00796053114863977,0.0011,-0.00373194815926121));
#48245=CARTESIAN_POINT('',(-0.00796053114863977,-0.0158951219150417,-0.00373194815926121));
#48246=CARTESIAN_POINT('',(-0.00847876085808972,0.0011,-0.00172555242739552));
#48247=CARTESIAN_POINT('Origin',(-0.00926982557395217,0.0011,-0.003));
#48248=CARTESIAN_POINT('',(-0.00847876085808972,0.0129,-0.00172555242739552));
#48249=CARTESIAN_POINT('',(-0.00847876085808972,-0.0158951219150417,-0.00172555242739552));
#48250=CARTESIAN_POINT('Origin',(-0.00926982557395217,0.0129,-0.003));
#48251=CARTESIAN_POINT('Origin',(8.56902727468245E-6,-0.0158951219150417,
-0.00745016612406076));
#48252=CARTESIAN_POINT('',(1.96218223641792E-6,0.0129,-0.00744699730453541));
#48253=CARTESIAN_POINT('',(1.96218223641796E-6,0.0011,-0.00744699730453541));
#48254=CARTESIAN_POINT('',(1.96218223641796E-6,-0.0158951219150417,-0.00744699730453541));
#48255=CARTESIAN_POINT('',(-0.00782999910211115,0.0011,-0.00369057927205054));
#48256=CARTESIAN_POINT('',(-0.00791734410653075,0.0011,-0.00364868627261692));
#48257=CARTESIAN_POINT('',(-0.00782999910211115,0.0129,-0.00369057927205054));
#48258=CARTESIAN_POINT('',(-0.00782999910211115,0.013,-0.00369057927205053));
#48259=CARTESIAN_POINT('',(8.56902727468244E-6,0.0129,-0.00745016612406076));
#48260=CARTESIAN_POINT('Origin',(0.0040613112974471,-0.0158951219150417,
-0.00870795090600599));
#48261=CARTESIAN_POINT('',(0.0040613112974471,0.0011,-0.00870795090600599));
#48262=CARTESIAN_POINT('',(0.0040613112974471,0.0129,-0.00870795090600599));
#48263=CARTESIAN_POINT('',(0.0040613112974471,-0.0158951219150417,-0.00870795090600599));
#48264=CARTESIAN_POINT('',(1.55672130369862E-5,0.0011,-0.00745233803901766));
#48265=CARTESIAN_POINT('',(8.56902727468726E-6,0.0011,-0.00745016612406076));
#48266=CARTESIAN_POINT('',(1.55672130369862E-5,0.0129,-0.00745233803901766));
#48267=CARTESIAN_POINT('',(1.55672130369867E-5,-0.0158951219150417,-0.00745233803901766));
#48268=CARTESIAN_POINT('',(0.0040613112974471,0.0129,-0.00870795090600599));
#48269=CARTESIAN_POINT('Origin',(0.00451057325136412,-0.0158951219150417,
-0.007561022432726));
#48270=CARTESIAN_POINT('',(0.00451057325136412,0.0011,-0.007561022432726));
#48271=CARTESIAN_POINT('',(0.00451057325136412,0.0129,-0.007561022432726));
#48272=CARTESIAN_POINT('',(0.00451057325136412,-0.0158951219150417,-0.007561022432726));
#48273=CARTESIAN_POINT('',(0.0040613112974471,0.0011,-0.00870795090600599));
#48274=CARTESIAN_POINT('',(0.00451057325136412,0.0129,-0.007561022432726));
#48275=CARTESIAN_POINT('Origin',(0.00432022868869639,-0.0158951219150417,
-0.00735468159030551));
#48276=CARTESIAN_POINT('',(0.00432022868869639,0.0011,-0.00735468159030551));
#48277=CARTESIAN_POINT('',(0.00432022868869639,0.0129,-0.00735468159030551));
#48278=CARTESIAN_POINT('',(0.00432022868869639,-0.0158951219150417,-0.00735468159030551));
#48279=CARTESIAN_POINT('',(0.00451057325136413,0.0011,-0.007561022432726));
#48280=CARTESIAN_POINT('',(0.00432022868869639,0.0129,-0.00735468159030551));
#48281=CARTESIAN_POINT('Origin',(0.00314085016583167,-0.0158951219150417,
-0.0077101355618168));
#48282=CARTESIAN_POINT('',(0.00314085016583167,0.0011,-0.0077101355618168));
#48283=CARTESIAN_POINT('',(0.00314085016583167,0.0129,-0.0077101355618168));
#48284=CARTESIAN_POINT('',(0.00314085016583167,-0.0158951219150417,-0.0077101355618168));
#48285=CARTESIAN_POINT('',(0.00432022868869639,0.0011,-0.00735468159030551));
#48286=CARTESIAN_POINT('',(0.00314085016583167,0.0129,-0.0077101355618168));
#48287=CARTESIAN_POINT('Origin',(0.00295417720403981,-0.0158951219150417,
-0.00747777661796151));
#48288=CARTESIAN_POINT('',(0.00295417720403981,0.0011,-0.00747777661796151));
#48289=CARTESIAN_POINT('',(0.00295417720403981,0.0129,-0.00747777661796151));
#48290=CARTESIAN_POINT('',(0.00295417720403981,-0.0158951219150417,-0.00747777661796151));
#48291=CARTESIAN_POINT('',(0.00314085016583167,0.0011,-0.0077101355618168));
#48292=CARTESIAN_POINT('',(0.00295417720403981,0.0129,-0.00747777661796151));
#48293=CARTESIAN_POINT('Origin',(0.00355542811483384,-0.0158951219150417,
-0.00640270519320544));
#48294=CARTESIAN_POINT('',(0.00355542811483384,0.0011,-0.00640270519320544));
#48295=CARTESIAN_POINT('',(0.00355542811483384,0.0129,-0.00640270519320544));
#48296=CARTESIAN_POINT('',(0.00355542811483384,-0.0158951219150417,-0.00640270519320544));
#48297=CARTESIAN_POINT('',(0.00295417720403981,0.0011,-0.00747777661796151));
#48298=CARTESIAN_POINT('',(0.00355542811483384,0.0129,-0.00640270519320544));
#48299=CARTESIAN_POINT('Origin',(0.00339495317277858,-0.0158951219150417,
-0.00617236763925401));
#48300=CARTESIAN_POINT('',(0.00339495317277858,0.0011,-0.00617236763925401));
#48301=CARTESIAN_POINT('',(0.00339495317277858,0.0129,-0.00617236763925401));
#48302=CARTESIAN_POINT('',(0.00339495317277858,-0.0158951219150417,-0.00617236763925401));
#48303=CARTESIAN_POINT('',(0.00355542811483384,0.0011,-0.00640270519320544));
#48304=CARTESIAN_POINT('',(0.00339495317277858,0.0129,-0.00617236763925401));
#48305=CARTESIAN_POINT('Origin',(0.00217815846891078,-0.0158951219150417,
-0.00636391887181847));
#48306=CARTESIAN_POINT('',(0.00217815846891078,0.0011,-0.00636391887181847));
#48307=CARTESIAN_POINT('',(0.00217815846891078,0.0129,-0.00636391887181847));
#48308=CARTESIAN_POINT('',(0.00217815846891078,-0.0158951219150417,-0.00636391887181847));
#48309=CARTESIAN_POINT('',(0.00339495317277858,0.0011,-0.00617236763925401));
#48310=CARTESIAN_POINT('',(0.00217815846891078,0.0129,-0.00636391887181847));
#48311=CARTESIAN_POINT('Origin',(0.00202486372793092,-0.0158951219150417,
-0.00610830550002113));
#48312=CARTESIAN_POINT('',(0.00202486372793092,0.0011,-0.00610830550002113));
#48313=CARTESIAN_POINT('',(0.00202486372793092,0.0129,-0.00610830550002113));
#48314=CARTESIAN_POINT('',(0.00202486372793092,-0.0158951219150417,-0.00610830550002113));
#48315=CARTESIAN_POINT('',(0.00217815846891078,0.0011,-0.00636391887181847));
#48316=CARTESIAN_POINT('',(0.00202486372793092,0.0129,-0.00610830550002113));
#48317=CARTESIAN_POINT('Origin',(0.00276690342874427,-0.0158951219150417,
-0.00512511767031892));
#48318=CARTESIAN_POINT('',(0.00276690342874427,0.0011,-0.00512511767031892));
#48319=CARTESIAN_POINT('',(0.00276690342874427,0.0129,-0.00512511767031892));
#48320=CARTESIAN_POINT('',(0.00276690342874427,-0.0158951219150417,-0.00512511767031892));
#48321=CARTESIAN_POINT('',(0.00202486372793092,0.0011,-0.00610830550002113));
#48322=CARTESIAN_POINT('',(0.00276690342874427,0.0129,-0.00512511767031892));
#48323=CARTESIAN_POINT('Origin',(0.00263928745184173,-0.0158951219150417,
-0.00487507415765127));
#48324=CARTESIAN_POINT('',(0.00263928745184173,0.0011,-0.00487507415765127));
#48325=CARTESIAN_POINT('',(0.00263928745184173,0.0129,-0.00487507415765127));
#48326=CARTESIAN_POINT('',(0.00263928745184173,-0.0158951219150417,-0.00487507415765127));
#48327=CARTESIAN_POINT('',(0.00276690342874427,0.0011,-0.00512511767031893));
#48328=CARTESIAN_POINT('',(0.00263928745184173,0.0129,-0.00487507415765127));
#48329=CARTESIAN_POINT('Origin',(0.0014077431500399,-0.0158951219150417,
-0.00489915441423508));
#48330=CARTESIAN_POINT('',(0.0014243849476499,0.0129,-0.0048988290189116));
#48331=CARTESIAN_POINT('',(0.0014243849476499,0.0011,-0.0048988290189116));
#48332=CARTESIAN_POINT('',(0.0014243849476499,0.001,-0.0048988290189116));
#48333=CARTESIAN_POINT('',(0.00263928745184173,0.0011,-0.00487507415765127));
#48334=CARTESIAN_POINT('',(0.0014077431500399,0.0129,-0.00489915441423508));
#48335=CARTESIAN_POINT('Origin',(-0.00846848477354713,-0.0158951219150417,
-0.00173198859563243));
#48336=CARTESIAN_POINT('',(-0.00845656001337402,0.0129,-0.00173581269660575));
#48337=CARTESIAN_POINT('',(-0.00845656001337402,0.0011,-0.00173581269660575));
#48338=CARTESIAN_POINT('',(-0.00845656001337402,0.001,-0.00173581269660575));
#48339=CARTESIAN_POINT('',(0.00139189322879002,0.0011,-0.00489407156993475));
#48340=CARTESIAN_POINT('',(0.0014077431500399,0.0011,-0.00489915441423508));
#48341=CARTESIAN_POINT('',(0.00139189322879002,0.0129,-0.00489407156993475));
#48342=CARTESIAN_POINT('',(0.00139189322879002,0.013,-0.00489407156993475));
#48343=CARTESIAN_POINT('',(-0.00846848477354713,0.0129,-0.00173198859563243));
#48344=CARTESIAN_POINT('Origin',(-0.00926982557395217,0.013,-0.003));
#48345=CARTESIAN_POINT('',(0.00439463505993757,0.013,-0.00758282450818601));
#48346=CARTESIAN_POINT('',(0.00400212262074066,0.013,-0.00858487618139458));
#48347=CARTESIAN_POINT('',(0.0039681998040106,0.013,-0.00867147831643483));
#48348=CARTESIAN_POINT('',(4.52079337442158E-5,0.013,-0.00735683187337399));
#48349=CARTESIAN_POINT('',(3.82097479819073E-5,0.013,-0.00735465995841708));
#48350=CARTESIAN_POINT('',(-0.00778675335060335,0.013,-0.00360041384088911));
#48351=CARTESIAN_POINT('',(-0.00787409835502296,0.013,-0.00355852084145549));
#48352=CARTESIAN_POINT('',(-0.00804781744366059,0.013,-0.00368315161531047));
#48353=CARTESIAN_POINT('Origin',(-0.00787324485361894,0.013,-0.00378074470321196));
#48354=CARTESIAN_POINT('',(-0.00853149850581388,0.013,-0.00181051559890248));
#48355=CARTESIAN_POINT('Origin',(-0.00926982557395217,0.013,-0.003));
#48356=CARTESIAN_POINT('',(-0.00848709681638249,0.013,-0.00183103613732295));
#48357=CARTESIAN_POINT('Origin',(-0.00842602321036556,0.013,-0.00164058925588855));
#48358=CARTESIAN_POINT('',(0.00136135642578156,0.013,-0.00498929501065195));
#48359=CARTESIAN_POINT('',(0.00137720634703143,0.013,-0.00499437785495228));
#48360=CARTESIAN_POINT('',(0.00142633986350131,0.013,-0.00499880990860565));
#48361=CARTESIAN_POINT('Origin',(0.00142243003179848,0.013,-0.00479884812921755));
#48362=CARTESIAN_POINT('',(0.00257866842927369,0.013,-0.00497627854900125));
#48363=CARTESIAN_POINT('',(0.00264124236769314,0.013,-0.00497505504734532));
#48364=CARTESIAN_POINT('',(0.00264938241039218,0.013,-0.00511483151597876));
#48365=CARTESIAN_POINT('',(0.0026778334082842,0.013,-0.00517057678882383));
#48366=CARTESIAN_POINT('',(0.00190441615676979,0.013,-0.00610189696988579));
#48367=CARTESIAN_POINT('',(0.00194504524815218,0.013,-0.00604806423272195));
#48368=CARTESIAN_POINT('',(0.00212708576461598,0.013,-0.00647319039387763));
#48369=CARTESIAN_POINT('',(0.00209239833118282,0.013,-0.00641535036778038));
#48370=CARTESIAN_POINT('',(0.00334867942190192,0.013,-0.00628088369661617));
#48371=CARTESIAN_POINT('',(0.00341050394316157,0.013,-0.00627115110720536));
#48372=CARTESIAN_POINT('',(0.00343760106241995,0.013,-0.00640851728792926));
#48373=CARTESIAN_POINT('',(0.00347337771318856,0.013,-0.00645986926924843));
#48374=CARTESIAN_POINT('',(0.00283397885998211,0.013,-0.00748782871937848));
#48375=CARTESIAN_POINT('',(0.00286689930638359,0.013,-0.00742896505600422));
#48376=CARTESIAN_POINT('',(0.00310513229246118,0.013,-0.00782534372202691));
#48377=CARTESIAN_POINT('',(0.00306289205711758,0.013,-0.00777276569263034));
#48378=CARTESIAN_POINT('',(0.00428916220193663,0.013,-0.00746848786485147));
#48379=CARTESIAN_POINT('',(0.00434908563218188,0.013,-0.00745042748741173));
#48380=CARTESIAN_POINT('',(0.00443707091227097,0.013,-0.00762882660772898));
#48381=CARTESIAN_POINT('',(-0.00926982557395217,0.013,-0.0036));
#48382=CARTESIAN_POINT('Origin',(-0.00926982557395217,0.013,-0.003));
#48383=CARTESIAN_POINT('Origin',(-0.00926982557395217,0.001,0.003));
#48384=CARTESIAN_POINT('',(0.00190441615676979,0.001,-0.00610189696988579));
#48385=CARTESIAN_POINT('',(0.00264938241039218,0.001,-0.00511483151597876));
#48386=CARTESIAN_POINT('',(0.00268708494896553,0.001,-0.00506487640301974));
#48387=CARTESIAN_POINT('',(0.00257866842927369,0.001,-0.00497627854900125));
#48388=CARTESIAN_POINT('',(0.00255021743138166,0.001,-0.00492053327615618));
#48389=CARTESIAN_POINT('',(0.00142633986350131,0.001,-0.00499880990860565));
#48390=CARTESIAN_POINT('',(0.00140969806589131,0.001,-0.00499913530392913));
#48391=CARTESIAN_POINT('',(0.00136135642578156,0.001,-0.00498929501065195));
#48392=CARTESIAN_POINT('Origin',(0.00142243003179848,0.001,-0.00479884812921755));
#48393=CARTESIAN_POINT('',(-0.00848709681638249,0.001,-0.00183103613732295));
#48394=CARTESIAN_POINT('',(-0.0084990215765556,0.001,-0.00182721203634963));
#48395=CARTESIAN_POINT('',(-0.00853149850581388,0.001,-0.00181051559890248));
#48396=CARTESIAN_POINT('Origin',(-0.00842602321036556,0.001,-0.00164058925588855));
#48397=CARTESIAN_POINT('',(-0.00804781744366059,0.001,-0.00368315161531047));
#48398=CARTESIAN_POINT('Origin',(-0.00926982557395217,0.001,-0.003));
#48399=CARTESIAN_POINT('',(-0.00778675335060335,0.001,-0.00360041384088911));
#48400=CARTESIAN_POINT('Origin',(-0.00787324485361894,0.001,-0.00378074470321196));
#48401=CARTESIAN_POINT('',(4.52079337441885E-5,0.001,-0.00735683187337398));
#48402=CARTESIAN_POINT('',(5.18147787824802E-5,0.001,-0.00736000069289933));
#48403=CARTESIAN_POINT('',(0.00400212262074066,0.001,-0.00858487618139458));
#48404=CARTESIAN_POINT('',(0.00409095201815433,0.001,-0.00861244474036231));
#48405=CARTESIAN_POINT('',(0.00439463505993757,0.001,-0.00758282450818601));
#48406=CARTESIAN_POINT('',(0.00441746175792763,0.001,-0.00752454984315485));
#48407=CARTESIAN_POINT('',(0.00428916220193663,0.001,-0.00746848786485146));
#48408=CARTESIAN_POINT('',(0.00424672634960324,0.001,-0.0074224857653085));
#48409=CARTESIAN_POINT('',(0.00310513229246118,0.001,-0.00782534372202691));
#48410=CARTESIAN_POINT('',(0.00316970710931718,0.001,-0.00780588145892302));
#48411=CARTESIAN_POINT('',(0.00283397885998211,0.001,-0.00748782871937848));
#48412=CARTESIAN_POINT('',(0.00287621909532571,0.001,-0.00754040674877505));
#48413=CARTESIAN_POINT('',(0.00343760106241995,0.001,-0.00640851728792926));
#48414=CARTESIAN_POINT('',(0.00346815021717762,0.001,-0.00635389363124816));
#48415=CARTESIAN_POINT('',(0.00334867942190192,0.001,-0.00628088369661617));
#48416=CARTESIAN_POINT('',(0.0033129027711333,0.001,-0.006229531715297));
#48417=CARTESIAN_POINT('',(0.00212708576461598,0.001,-0.00647319039387763));
#48418=CARTESIAN_POINT('',(0.00219370923929376,0.001,-0.00646270233976982));
#48419=CARTESIAN_POINT('',(0.00193910359020296,0.001,-0.00615973699598304));
#48420=CARTESIAN_POINT('',(-0.00926982557395217,0.001,-0.0024));
#48421=CARTESIAN_POINT('Origin',(-0.00926982557395217,0.001,-0.003));
#48422=CARTESIAN_POINT('Origin',(-0.00926982557395217,0.0172006855706717,
-0.003));
#48423=CARTESIAN_POINT('',(-0.00926982557395217,0.0129,-0.0025));
#48424=CARTESIAN_POINT('',(-0.00926982557395217,0.0129,-0.0035));
#48425=CARTESIAN_POINT('Origin',(-0.00926982557395217,0.0129,-0.003));
#48426=CARTESIAN_POINT('Origin',(-0.00926982557395217,0.0129,-0.003));
#48427=CARTESIAN_POINT('',(-0.00926982557395217,0.0011,-0.0025));
#48428=CARTESIAN_POINT('',(-0.00926982557395217,0.0172006855706717,-0.0025));
#48429=CARTESIAN_POINT('Origin',(-0.00926982557395217,0.0011,-0.003));
#48430=CARTESIAN_POINT('Origin',(0.00441815830616679,0.0011,-0.00465522418821883));
#48431=CARTESIAN_POINT('Origin',(0.00343760106241995,0.0011,-0.00640851728792926));
#48432=CARTESIAN_POINT('Origin',(0.00283397885998212,0.0011,-0.00748782871937848));
#48433=CARTESIAN_POINT('Origin',(-0.00703448893161721,0.0011,0.00479582892185301));
#48434=CARTESIAN_POINT('Origin',(0.00310513229246118,0.0011,-0.00782534372202691));
#48435=CARTESIAN_POINT('Origin',(0.00287621909532571,0.0129,-0.00754040674877505));
#48436=CARTESIAN_POINT('Origin',(0.00310513229246118,0.0129,-0.00782534372202691));
#48437=CARTESIAN_POINT('Origin',(0.00283397885998211,0.0129,-0.00748782871937848));
#48438=CARTESIAN_POINT('Origin',(0.00346815021717762,0.0129,-0.00635389363124816));
#48439=CARTESIAN_POINT('Origin',(0.00343760106241995,0.0129,-0.00640851728792926));
#48440=CARTESIAN_POINT('Origin',(-0.00512775505089191,0.0011,0.00588575838274743));
#48441=CARTESIAN_POINT('Origin',(0.00334867942190192,0.0011,-0.00628088369661617));
#48442=CARTESIAN_POINT('Origin',(-0.00524836317811532,0.0011,-0.0103430113609166));
#48443=CARTESIAN_POINT('Origin',(0.00428916220193663,0.0011,-0.00746848786485146));
#48444=CARTESIAN_POINT('Origin',(0.00316970710931718,0.0129,-0.00780588145892302));
#48445=CARTESIAN_POINT('Origin',(0.00428916220193663,0.0129,-0.00746848786485147));
#48446=CARTESIAN_POINT('Origin',(0.00331290277113331,0.0129,-0.006229531715297));
#48447=CARTESIAN_POINT('Origin',(0.00334867942190192,0.0129,-0.00628088369661617));
#48448=CARTESIAN_POINT('Origin',(-0.00753898540761223,0.0011,-0.00799485040867771));
#48449=CARTESIAN_POINT('Origin',(0.00212708576461597,0.0011,-0.00647319039387763));
#48450=CARTESIAN_POINT('Origin',(-0.00716170400106153,0.0011,0.00494469245223184));
#48451=CARTESIAN_POINT('Origin',(0.00439463505993757,0.0011,-0.00758282450818601));
#48452=CARTESIAN_POINT('Origin',(0.00424672634960323,0.0129,-0.00742248576530849));
#48453=CARTESIAN_POINT('Origin',(0.00439463505993757,0.0129,-0.00758282450818601));
#48454=CARTESIAN_POINT('Origin',(0.00219370923929376,0.0129,-0.00646270233976982));
#48455=CARTESIAN_POINT('Origin',(0.00212708576461598,0.0129,-0.00647319039387763));
#48456=CARTESIAN_POINT('Origin',(-0.00506603229059289,0.0011,0.00552107077956914));
#48457=CARTESIAN_POINT('Origin',(0.00190441615676979,0.0011,-0.00610189696988579));
#48458=CARTESIAN_POINT('Origin',(0.00617086596586019,0.0011,-0.00304825445754962));
#48459=CARTESIAN_POINT('Origin',(0.00400212262074066,0.0011,-0.00858487618139458));
#48460=CARTESIAN_POINT('Origin',(0.00441746175792763,0.0129,-0.00752454984315485));
#48461=CARTESIAN_POINT('Origin',(0.00400212262074066,0.0129,-0.00858487618139458));
#48462=CARTESIAN_POINT('Origin',(0.00193910359020296,0.0129,-0.00615973699598304));
#48463=CARTESIAN_POINT('Origin',(0.00190441615676979,0.0129,-0.00610189696988579));
#48464=CARTESIAN_POINT('Origin',(0.00222579787364439,0.0011,-0.00567607259367848));
#48465=CARTESIAN_POINT('Origin',(0.00264938241039218,0.0011,-0.00511483151597876));
#48466=CARTESIAN_POINT('Origin',(-0.0113833186128506,0.0011,-0.00380994292458512));
#48467=CARTESIAN_POINT('Origin',(4.52079337442121E-5,0.0011,-0.00735683187337399));
#48468=CARTESIAN_POINT('Origin',(4.52079337442124E-5,-0.0158951219150417,
-0.00735683187337399));
#48469=CARTESIAN_POINT('Origin',(4.52079337442121E-5,0.0129,-0.00735683187337399));
#48470=CARTESIAN_POINT('Origin',(4.52079337442123E-5,0.0011,-0.00735683187337399));
#48471=CARTESIAN_POINT('Origin',(0.00409095201815432,0.0129,-0.00861244474036231));
#48472=CARTESIAN_POINT('Origin',(4.52079337442158E-5,0.0129,-0.00735683187337399));
#48473=CARTESIAN_POINT('Origin',(0.00268708494896553,0.0129,-0.00506487640301974));
#48474=CARTESIAN_POINT('Origin',(0.00264938241039218,0.0129,-0.00511483151597876));
#48475=CARTESIAN_POINT('Origin',(-0.00309949089713811,0.0011,0.00614918503262233));
#48476=CARTESIAN_POINT('Origin',(0.00257866842927369,0.0011,-0.00497627854900125));
#48477=CARTESIAN_POINT('Origin',(4.52079337442135E-5,0.0011,-0.00735683187337399));
#48478=CARTESIAN_POINT('Origin',(4.52079337441885E-5,0.0011,-0.00735683187337398));
#48479=CARTESIAN_POINT('Origin',(4.52079337442119E-5,0.0129,-0.00735683187337399));
#48480=CARTESIAN_POINT('Origin',(4.52079337442122E-5,0.0129,-0.00735683187337399));
#48481=CARTESIAN_POINT('Origin',(0.00255021743138166,0.0129,-0.00492053327615618));
#48482=CARTESIAN_POINT('Origin',(0.00257866842927369,0.0129,-0.00497627854900125));
#48483=CARTESIAN_POINT('Origin',(-0.00910939770465845,0.0011,-0.00520481408041643));
#48484=CARTESIAN_POINT('Origin',(0.00142633986350131,0.0011,-0.00499880990860565));
#48485=CARTESIAN_POINT('Origin',(-0.0115661429208045,0.0011,-0.00178771755475424));
#48486=CARTESIAN_POINT('Origin',(-0.00778675335060335,0.0011,-0.00360041384088911));
#48487=CARTESIAN_POINT('Origin',(-0.00787324485361894,-0.0158951219150417,
-0.00378074470321196));
#48488=CARTESIAN_POINT('Origin',(-0.00787324485361894,0.0129,-0.00378074470321196));
#48489=CARTESIAN_POINT('Origin',(-0.00787324485361894,0.0011,-0.00378074470321196));
#48490=CARTESIAN_POINT('Origin',(5.18147787824767E-5,0.0129,-0.00736000069289933));
#48491=CARTESIAN_POINT('Origin',(-0.00778675335060335,0.0129,-0.00360041384088911));
#48492=CARTESIAN_POINT('Origin',(0.00140969806589131,0.0129,-0.00499913530392913));
#48493=CARTESIAN_POINT('Origin',(0.00142633986350131,0.0129,-0.00499880990860565));
#48494=CARTESIAN_POINT('Origin',(0.00142243003179848,-0.0158951219150417,
-0.00479884812921755));
#48495=CARTESIAN_POINT('Origin',(0.00142243003179848,0.0011,-0.00479884812921755));
#48496=CARTESIAN_POINT('Origin',(0.00142243003179848,0.0129,-0.00479884812921755));
#48497=CARTESIAN_POINT('Origin',(0.00142243003179848,0.0011,-0.00479884812921755));
#48498=CARTESIAN_POINT('Origin',(0.00136135642578156,0.0011,-0.00498929501065196));
#48499=CARTESIAN_POINT('Origin',(-0.00787324485361894,0.0011,-0.00378074470321196));
#48500=CARTESIAN_POINT('Origin',(-0.00804781744366059,0.0011,-0.00368315161531047));
#48501=CARTESIAN_POINT('Origin',(-0.00787324485361894,0.0129,-0.00378074470321196));
#48502=CARTESIAN_POINT('Origin',(-0.00804781744366059,0.0129,-0.00368315161531047));
#48503=CARTESIAN_POINT('Origin',(0.00142243003179848,0.0129,-0.00479884812921755));
#48504=CARTESIAN_POINT('Origin',(0.00136135642578156,0.0129,-0.00498929501065195));
#48505=CARTESIAN_POINT('Origin',(-0.0106016144887901,0.0011,-0.0011529403960444));
#48506=CARTESIAN_POINT('Origin',(-0.00848709681638249,0.0011,-0.00183103613732295));
#48507=CARTESIAN_POINT('Origin',(-0.00926982557395217,0.0011,-0.003));
#48508=CARTESIAN_POINT('Origin',(-0.00853149850581388,0.0011,-0.00181051559890248));
#48509=CARTESIAN_POINT('Origin',(-0.00926982557395217,0.0129,-0.003));
#48510=CARTESIAN_POINT('Origin',(-0.00853149850581388,0.0129,-0.00181051559890248));
#48511=CARTESIAN_POINT('Origin',(-0.0084990215765556,0.0129,-0.00182721203634963));
#48512=CARTESIAN_POINT('Origin',(-0.00848709681638249,0.0129,-0.00183103613732295));
#48513=CARTESIAN_POINT('Origin',(-0.00842602321036556,0.0011,-0.00164058925588855));
#48514=CARTESIAN_POINT('Origin',(-0.00842602321036556,0.0011,-0.00164058925588855));
#48515=CARTESIAN_POINT('Origin',(-0.00842602321036556,0.0129,-0.00164058925588855));
#48516=CARTESIAN_POINT('Origin',(-0.00842602321036556,0.0129,-0.00164058925588855));
#48517=CARTESIAN_POINT('Origin',(-0.00842602321036556,-0.0158951219150417,
-0.00164058925588855));
#48518=CARTESIAN_POINT('Origin',(-0.00926982557395217,0.0011,-0.003));
#48519=CARTESIAN_POINT('Origin',(-0.00926982557395217,0.0011,-0.0024));
#48520=CARTESIAN_POINT('Origin',(-0.00926982557395217,0.0129,-0.003));
#48521=CARTESIAN_POINT('Origin',(-0.00926982557395217,0.0129,-0.0036));
#48522=CARTESIAN_POINT('',(0.,0.,0.));
#48523=CARTESIAN_POINT('Origin',(0.,-0.00311126983722081,0.));
#48524=CARTESIAN_POINT('',(-1.34711147906209E-19,0.013,-0.0011));
#48525=CARTESIAN_POINT('Origin',(0.,0.013,0.));
#48526=CARTESIAN_POINT('',(0.,0.,-0.0011));
#48527=CARTESIAN_POINT('',(-1.34711147906209E-19,-0.00311126983722081,-0.0011));
#48528=CARTESIAN_POINT('Origin',(0.,0.,0.));
#48529=CARTESIAN_POINT('Origin',(0.00213706124849222,0.,0.000772521431045073));
#48530=CARTESIAN_POINT('Origin',(0.,0.013,-0.012));
#48531=CARTESIAN_POINT('',(0.0005,0.014,-0.012));
#48532=CARTESIAN_POINT('',(-0.0005,0.014,-0.012));
#48533=CARTESIAN_POINT('Origin',(0.,0.014,-0.012));
#48534=CARTESIAN_POINT('',(0.0005,0.013,-0.012));
#48535=CARTESIAN_POINT('',(0.0005,0.013,-0.012));
#48536=CARTESIAN_POINT('',(-0.0005,0.013,-0.012));
#48537=CARTESIAN_POINT('Origin',(0.,0.013,-0.012));
#48538=CARTESIAN_POINT('',(-0.0005,0.013,-0.012));
#48539=CARTESIAN_POINT('Origin',(0.0005,0.013,-0.012));
#48540=CARTESIAN_POINT('',(0.00124754980749396,0.014,-7.8227091354418E-5));
#48541=CARTESIAN_POINT('',(0.0005,0.014,-0.012));
#48542=CARTESIAN_POINT('',(0.00124754980749396,0.013,-7.8227091354418E-5));
#48543=CARTESIAN_POINT('',(0.00124754980749396,0.013,-7.8227091354418E-5));
#48544=CARTESIAN_POINT('',(0.0005,0.013,-0.012));
#48545=CARTESIAN_POINT('Origin',(0.,0.013,0.));
#48546=CARTESIAN_POINT('',(-0.00124754980749396,0.014,-7.82270913544182E-5));
#48547=CARTESIAN_POINT('Origin',(0.,0.014,0.));
#48548=CARTESIAN_POINT('',(-0.00124754980749396,0.013,-7.82270913544182E-5));
#48549=CARTESIAN_POINT('',(-0.00124754980749396,0.013,-7.82270913544182E-5));
#48550=CARTESIAN_POINT('Origin',(0.,0.013,0.));
#48551=CARTESIAN_POINT('Origin',(-0.0005,0.013,-0.012));
#48552=CARTESIAN_POINT('',(-0.0005,0.014,-0.012));
#48553=CARTESIAN_POINT('',(-0.0005,0.013,-0.012));
#48554=CARTESIAN_POINT('Origin',(0.,0.013,-0.012));
#48555=CARTESIAN_POINT('Origin',(0.,0.014,0.));
#48556=CARTESIAN_POINT('',(0.,0.,0.));
#48557=CARTESIAN_POINT('Origin',(0.00475,0.014,0.));
#48558=CARTESIAN_POINT('',(-0.0085,0.014,-1.04094977927525E-18));
#48559=CARTESIAN_POINT('Origin',(1.20286593710508E-18,0.014,0.));
#48560=CARTESIAN_POINT('',(0.0055,0.014,0.));
#48561=CARTESIAN_POINT('Origin',(-1.86727542905183E-18,0.014,0.));
#48562=CARTESIAN_POINT('Origin',(0.,0.0230185533732548,0.));
#48563=CARTESIAN_POINT('',(0.009,0.0135,0.));
#48564=CARTESIAN_POINT('',(-0.009,0.0135,-1.10218211923262E-18));
#48565=CARTESIAN_POINT('Origin',(1.2695543452855E-18,0.0135,0.));
#48566=CARTESIAN_POINT('Origin',(1.2695543452855E-18,0.0135,0.));
#48567=CARTESIAN_POINT('',(0.009,-0.000500000000000003,-1.10218211923262E-18));
#48568=CARTESIAN_POINT('',(0.009,0.0230185533732548,-1.10218211923262E-18));
#48569=CARTESIAN_POINT('Origin',(3.13682977433732E-18,-0.0005,0.));
#48570=CARTESIAN_POINT('Origin',(0.009,-0.001,0.));
#48571=CARTESIAN_POINT('',(0.0085,-0.000999999999999999,-1.04094977927525E-18));
#48572=CARTESIAN_POINT('Origin',(3.20351818251775E-18,-0.001,0.));
#48573=CARTESIAN_POINT('',(0.0055,-0.001,-6.73555739531044E-19));
#48574=CARTESIAN_POINT('Origin',(1.33376816360845E-19,-0.001,0.));
#48575=CARTESIAN_POINT('Origin',(2.13402906177352E-18,-0.016,0.));
#48576=CARTESIAN_POINT('',(0.0055,-0.016,-6.73555739531044E-19));
#48577=CARTESIAN_POINT('Origin',(3.13682977433732E-18,-0.0005,0.));
#48578=CARTESIAN_POINT('Origin',(0.0085,-0.000499999999999999,-1.04094977927525E-18));
#48579=CARTESIAN_POINT('Origin',(1.2695543452855E-18,0.0135,0.));
#48580=CARTESIAN_POINT('Origin',(-0.0085,0.0135,-1.04094977927525E-18));
#48581=CARTESIAN_POINT('',(0.,0.,0.));
#48582=CARTESIAN_POINT('Origin',(0.0016,0.,0.));
#48583=CARTESIAN_POINT('',(-0.00145274996309991,0.000934523397478773,-0.000217677932639515));
#48584=CARTESIAN_POINT('',(-0.00154602165644221,0.000569150220513997,-0.000136439597205102));
#48585=CARTESIAN_POINT('Origin',(0.00156503616117409,8.06815870157537E-5,
0.000322726348063015));
#48586=CARTESIAN_POINT('',(-0.00145274996309991,0.000934523397478773,0.000217677932639515));
#48587=CARTESIAN_POINT('Origin',(0.00166379421431252,0.000606961405040141,
0.));
#48588=CARTESIAN_POINT('',(-0.00154602165644221,0.000569150220513997,0.000136439597205102));
#48589=CARTESIAN_POINT('Origin',(0.00156503616117409,8.06815870157537E-5,
-0.000322726348063015));
#48590=CARTESIAN_POINT('',(-0.00157234339721419,0.000296847915734235,0.000296847915734239));
#48591=CARTESIAN_POINT('Origin',(0.00160749262454254,3.56437803082174E-5,
6.17368384676569E-5));
#48592=CARTESIAN_POINT('',(-0.00154602165644221,0.000136439597205108,0.000569150220513995));
#48593=CARTESIAN_POINT('Origin',(0.00160749262454254,6.17368384676549E-5,
3.56437803082147E-5));
#48594=CARTESIAN_POINT('',(-0.00145274996309991,0.000217677932639525,0.000934523397478771));
#48595=CARTESIAN_POINT('Origin',(0.00156503616117409,-0.000322726348063014,
8.06815870157571E-5));
#48596=CARTESIAN_POINT('',(-0.00145274996309991,-0.000217677932639505,0.000934523397478775));
#48597=CARTESIAN_POINT('Origin',(0.00166379421431252,6.37287751623816E-18,
0.000606961405040141));
#48598=CARTESIAN_POINT('',(-0.00154602165644221,-0.000136439597205096,0.000569150220513998));
#48599=CARTESIAN_POINT('Origin',(0.00156503616117409,0.000322726348063016,
8.06815870157503E-5));
#48600=CARTESIAN_POINT('',(-0.00157234339721419,-0.000296847915734233,0.000296847915734241));
#48601=CARTESIAN_POINT('Origin',(0.00160749262454254,-6.17368384676559E-5,
3.56437803082175E-5));
#48602=CARTESIAN_POINT('',(-0.00154602165644221,-0.000569150220513996,0.000136439597205106));
#48603=CARTESIAN_POINT('Origin',(0.00160749262454254,-3.5643780308217E-5,
6.17368384676573E-5));
#48604=CARTESIAN_POINT('',(-0.00145274996309991,-0.000934523397478772,0.000217677932639521));
#48605=CARTESIAN_POINT('Origin',(0.00156503616117409,-8.06815870157559E-5,
-0.000322726348063014));
#48606=CARTESIAN_POINT('',(-0.00146025981347714,-0.000935312714559631,1.14542772208728E-19));
#48607=CARTESIAN_POINT('Origin',(0.00166379421431252,-0.000606961405040141,
4.15622446711184E-18));
#48608=CARTESIAN_POINT('',(-0.00089799919935936,-0.002,2.44929359829471E-19));
#48609=CARTESIAN_POINT('Origin',(0.0016,0.,0.));
#48610=CARTESIAN_POINT('',(-0.00089799919935936,-2.44929359829471E-19,-0.002));
#48611=CARTESIAN_POINT('Origin',(-0.00089799919935936,0.,0.));
#48612=CARTESIAN_POINT('Origin',(-0.00089799919935936,0.,0.));
#48613=CARTESIAN_POINT('',(-0.00145274996309991,-0.000934523397478775,-0.000217677932639508));
#48614=CARTESIAN_POINT('Origin',(0.00166379421431252,-0.000606961405040141,
4.15622446711184E-18));
#48615=CARTESIAN_POINT('',(-0.00154602165644221,-0.000569150220513998,-0.000136439597205098));
#48616=CARTESIAN_POINT('Origin',(0.00156503616117409,-8.06815870157514E-5,
0.000322726348063015));
#48617=CARTESIAN_POINT('',(-0.00157234339721419,-0.000296847915734242,-0.000296847915734239));
#48618=CARTESIAN_POINT('Origin',(0.00160749262454254,-3.56437803082212E-5,
-6.17368384676608E-5));
#48619=CARTESIAN_POINT('',(-0.00154602165644221,-0.000136439597205104,-0.000569150220513996));
#48620=CARTESIAN_POINT('Origin',(0.00160749262454254,-6.17368384676611E-5,
-3.56437803082205E-5));
#48621=CARTESIAN_POINT('',(-0.00145274996309991,-0.000217677932639518,-0.000934523397478772));
#48622=CARTESIAN_POINT('Origin',(0.00156503616117409,0.000322726348063015,
-8.06815870157548E-5));
#48623=CARTESIAN_POINT('',(-0.00145274996309991,0.000217677932639511,-0.000934523397478774));
#48624=CARTESIAN_POINT('Origin',(0.00166379421431252,-2.21665304912631E-18,
-0.000606961405040141));
#48625=CARTESIAN_POINT('',(-0.00154602165644221,0.0001364395972051,-0.000569150220513997));
#48626=CARTESIAN_POINT('Origin',(0.00156503616117409,-0.000322726348063015,
-8.06815870157525E-5));
#48627=CARTESIAN_POINT('',(-0.00157234339721419,0.000296847915734235,-0.000296847915734239));
#48628=CARTESIAN_POINT('Origin',(0.00160749262454254,6.17368384676561E-5,
-3.5643780308217E-5));
#48629=CARTESIAN_POINT('Origin',(0.00160749262454254,3.56437803082175E-5,
-6.1736838467657E-5));
#48630=CARTESIAN_POINT('Origin',(0.,0.001,0.));
#48631=CARTESIAN_POINT('',(0.,-2.44929359829471E-19,-0.002));
#48632=CARTESIAN_POINT('Origin',(0.,0.,0.));
#48633=CARTESIAN_POINT('',(0.,-1.34711147906209E-19,-0.0011));
#48634=CARTESIAN_POINT('Origin',(0.,0.,0.));
#48635=CARTESIAN_POINT('Origin',(0.,0.,0.));
#48636=CARTESIAN_POINT('',(0.,-2.44929359829471E-19,-0.002));
#48637=CARTESIAN_POINT('Origin',(0.0045,0.001,0.));
#48638=CARTESIAN_POINT('',(0.0045,-9.79717439317885E-20,-0.000800000000000002));
#48639=CARTESIAN_POINT('Origin',(0.0045,0.,0.));
#48640=CARTESIAN_POINT('Origin',(0.,0.,0.));
#48641=CARTESIAN_POINT('',(0.0001,-1.22464679914735E-19,-0.001));
#48642=CARTESIAN_POINT('Origin',(0.0001,0.,0.));
#48643=CARTESIAN_POINT('',(0.00415358983848623,-1.22464679914735E-19,-0.001));
#48644=CARTESIAN_POINT('',(0.,-1.22464679914735E-19,-0.001));
#48645=CARTESIAN_POINT('Origin',(0.00415358983848623,0.,0.));
#48646=CARTESIAN_POINT('Origin',(0.00415358983848623,0.,0.));
#48647=CARTESIAN_POINT('',(0.00415358983848623,-1.22464679914735E-19,-0.001));
#48648=CARTESIAN_POINT('Origin',(-0.0016,0.00095,-0.0002375));
#48649=CARTESIAN_POINT('',(-0.00075,0.000556618474827239,-4.70664976705276E-5));
#48650=CARTESIAN_POINT('',(-0.0016,0.00057,-0.0001425));
#48651=CARTESIAN_POINT('',(-0.00075,0.000860661400024175,-0.000123077228969761));
#48652=CARTESIAN_POINT('',(-0.00075,2.16677931850071E-5,8.66711727400304E-5));
#48653=CARTESIAN_POINT('',(-0.00153787007542131,0.000943469881790042,-0.000229136378665655));
#48654=CARTESIAN_POINT('Origin',(-0.0016,0.00095,0.0002375));
#48655=CARTESIAN_POINT('',(-0.00075,0.000860661400024175,0.000123077228969761));
#48656=CARTESIAN_POINT('',(-0.00075,0.000860661400024175,-4.33680868994202E-19));
#48657=CARTESIAN_POINT('',(-0.0016,0.00095,0.0002375));
#48658=CARTESIAN_POINT('Origin',(-0.0016,0.00095,0.0002375));
#48659=CARTESIAN_POINT('',(-0.00075,0.000556618474827239,4.70664976705276E-5));
#48660=CARTESIAN_POINT('',(-0.00075,2.16677931850068E-5,-8.66711727400304E-5));
#48661=CARTESIAN_POINT('',(-0.00161643715208567,0.00057025876960518,0.00014434547646101));
#48662=CARTESIAN_POINT('Origin',(-0.0016,0.00057,0.0001425));
#48663=CARTESIAN_POINT('',(-0.00075,0.000233575465858467,0.000233575465858471));
#48664=CARTESIAN_POINT('',(-0.00075,0.000159535010031724,0.000276322742960963));
#48665=CARTESIAN_POINT('',(-0.00160871040111109,0.000299646052667046,0.000299646052667049));
#48666=CARTESIAN_POINT('Origin',(-0.0016,0.000142500000000006,0.00057));
#48667=CARTESIAN_POINT('',(-0.00075,4.70664976705335E-5,0.000556618474827239));
#48668=CARTESIAN_POINT('',(-0.00075,0.000276322742960963,0.000159535010031717));
#48669=CARTESIAN_POINT('',(-0.0016,0.000142500000000006,0.00057));
#48670=CARTESIAN_POINT('Origin',(-0.0016,0.0002375,0.00095));
#48671=CARTESIAN_POINT('',(-0.00075,0.00012307722896977,0.000860661400024173));
#48672=CARTESIAN_POINT('',(-0.00075,-8.66711727400301E-5,2.16677931850079E-5));
#48673=CARTESIAN_POINT('',(-0.00153787007542131,0.000229136378665665,0.00094346988179004));
#48674=CARTESIAN_POINT('Origin',(-0.0016,-0.00023749999999999,0.00095));
#48675=CARTESIAN_POINT('',(-0.00075,-0.000123077228969752,0.000860661400024176));
#48676=CARTESIAN_POINT('',(-0.00075,8.44032546730324E-18,0.000860661400024174));
#48677=CARTESIAN_POINT('',(-0.0016,-0.00023749999999999,0.00095));
#48678=CARTESIAN_POINT('Origin',(-0.0016,-0.00023749999999999,0.00095));
#48679=CARTESIAN_POINT('',(-0.00075,-4.70664976705218E-5,0.00055661847482724));
#48680=CARTESIAN_POINT('',(-0.00075,8.66711727400305E-5,2.16677931850063E-5));
#48681=CARTESIAN_POINT('',(-0.00161643715208567,-0.000144345476461004,0.000570258769605181));
#48682=CARTESIAN_POINT('Origin',(-0.0016,-0.000142499999999994,0.00057));
#48683=CARTESIAN_POINT('',(-0.00075,-0.000233575465858466,0.000233575465858473));
#48684=CARTESIAN_POINT('',(-0.00075,-0.000276322742960961,0.000159535010031725));
#48685=CARTESIAN_POINT('',(-0.00160871040111109,-0.000299646052667044,0.000299646052667051));
#48686=CARTESIAN_POINT('Origin',(-0.0016,-0.00057,0.000142500000000004));
#48687=CARTESIAN_POINT('',(-0.00075,-0.000556618474827239,4.70664976705315E-5));
#48688=CARTESIAN_POINT('',(-0.00075,-0.000159535010031723,0.000276322742960963));
#48689=CARTESIAN_POINT('',(-0.0016,-0.00057,0.000142500000000004));
#48690=CARTESIAN_POINT('Origin',(-0.0016,-0.00095,0.000237500000000007));
#48691=CARTESIAN_POINT('',(-0.00075,-0.000860661400024174,0.000123077228969767));
#48692=CARTESIAN_POINT('',(-0.00075,-2.16677931850086E-5,-8.667117274003E-5));
#48693=CARTESIAN_POINT('',(-0.00153787007542131,-0.000943469881790041,0.000229136378665661));
#48694=CARTESIAN_POINT('Origin',(-0.0016,-0.00095,-0.000237499999999993));
#48695=CARTESIAN_POINT('',(-0.00075,-0.000860661400024175,-0.000123077228969755));
#48696=CARTESIAN_POINT('',(-0.00075,-0.000860661400024175,5.45977782372553E-18));
#48697=CARTESIAN_POINT('',(-0.0016,-0.00095,-0.000237499999999993));
#48698=CARTESIAN_POINT('Origin',(-0.0016,-0.00095,-0.000237499999999993));
#48699=CARTESIAN_POINT('',(-0.00075,-0.000556618474827239,-4.70664976705236E-5));
#48700=CARTESIAN_POINT('',(-0.00075,-2.16677931850076E-5,8.66711727400303E-5));
#48701=CARTESIAN_POINT('',(-0.00161643715208567,-0.000570258769605181,-0.000144345476461006));
#48702=CARTESIAN_POINT('Origin',(-0.0016,-0.00057,-0.000142499999999996));
#48703=CARTESIAN_POINT('',(-0.00075,-0.000233575465858474,-0.000233575465858472));
#48704=CARTESIAN_POINT('',(-0.00075,-0.000159535010031733,-0.000276322742960964));
#48705=CARTESIAN_POINT('',(-0.00160871040111109,-0.000299646052667053,-0.000299646052667049));
#48706=CARTESIAN_POINT('Origin',(-0.0016,-0.000142500000000002,-0.00057));
#48707=CARTESIAN_POINT('',(-0.00075,-4.70664976705294E-5,-0.000556618474827239));
#48708=CARTESIAN_POINT('',(-0.00075,-0.000276322742960965,-0.000159535010031729));
#48709=CARTESIAN_POINT('',(-0.0016,-0.000142500000000002,-0.00057));
#48710=CARTESIAN_POINT('Origin',(-0.0016,-0.000237500000000003,-0.00095));
#48711=CARTESIAN_POINT('',(-0.00075,-0.000123077228969764,-0.000860661400024174));
#48712=CARTESIAN_POINT('',(-0.00075,8.667117274003E-5,-2.16677931850084E-5));
#48713=CARTESIAN_POINT('',(-0.00153787007542131,-0.000229136378665658,-0.000943469881790042));
#48714=CARTESIAN_POINT('Origin',(-0.0016,0.000237499999999997,-0.00095));
#48715=CARTESIAN_POINT('',(-0.00075,0.000123077228969758,-0.000860661400024175));
#48716=CARTESIAN_POINT('',(-0.00075,-3.73948916431755E-18,-0.000860661400024175));
#48717=CARTESIAN_POINT('',(-0.0016,0.000237499999999997,-0.00095));
#48718=CARTESIAN_POINT('Origin',(-0.0016,0.000237499999999997,-0.00095));
#48719=CARTESIAN_POINT('',(-0.00075,4.70664976705257E-5,-0.00055661847482724));
#48720=CARTESIAN_POINT('',(-0.00075,-8.66711727400302E-5,-2.16677931850075E-5));
#48721=CARTESIAN_POINT('',(-0.00161643715208567,0.000144345476461008,-0.00057025876960518));
#48722=CARTESIAN_POINT('Origin',(-0.0016,0.000142499999999998,-0.00057));
#48723=CARTESIAN_POINT('',(-0.00075,0.000233575465858468,-0.000233575465858471));
#48724=CARTESIAN_POINT('',(-0.00075,0.000276322742960961,-0.000159535010031724));
#48725=CARTESIAN_POINT('',(-0.00160871040111109,0.000299646052667046,-0.000299646052667049));
#48726=CARTESIAN_POINT('Origin',(-0.0016,0.00057,-0.0001425));
#48727=CARTESIAN_POINT('',(-0.00075,0.000159535010031724,-0.000276322742960963));
#48728=CARTESIAN_POINT('Origin',(-0.00075,-5.96311194867027E-19,-4.33680868994202E-19));
#48729=CARTESIAN_POINT('Origin',(0.0001,0.,0.));
#48730=CARTESIAN_POINT('Origin',(0.0001,-1.34711147906209E-19,-0.0011));
#48731=CARTESIAN_POINT('',(0.,0.,0.));
#48732=CARTESIAN_POINT('Origin',(0.,0.001,0.));
#48733=CARTESIAN_POINT('',(0.00625,0.0009,-0.0119660979437743));
#48734=CARTESIAN_POINT('',(0.00625,0.0001,-0.0119660979437743));
#48735=CARTESIAN_POINT('',(0.00625,0.001,-0.0119660979437743));
#48736=CARTESIAN_POINT('',(0.00625,0.0001,0.0119660979437743));
#48737=CARTESIAN_POINT('Origin',(0.,0.0001,0.));
#48738=CARTESIAN_POINT('',(0.00625,0.0009,0.0119660979437743));
#48739=CARTESIAN_POINT('',(0.00625,0.001,0.0119660979437743));
#48740=CARTESIAN_POINT('Origin',(0.,0.0009,0.));
#48741=CARTESIAN_POINT('Origin',(0.0125,0.001,-4.59242549680257E-18));
#48742=CARTESIAN_POINT('Origin',(0.0125,0.0001,-4.59242549680257E-18));
#48743=CARTESIAN_POINT('Origin',(0.0125,0.0009,-4.59242549680257E-18));
#48744=CARTESIAN_POINT('Origin',(0.00625,0.001,-2.29621274840129E-18));
#48745=CARTESIAN_POINT('',(0.00625,0.001,-0.0118531641345254));
#48746=CARTESIAN_POINT('',(0.00625,0.001,0.0118531641345254));
#48747=CARTESIAN_POINT('Origin',(0.,0.001,0.));
#48748=CARTESIAN_POINT('Origin',(0.0125,0.001,-4.59242549680257E-18));
#48749=CARTESIAN_POINT('',(0.0125,0.001,-0.00910000000000001));
#48750=CARTESIAN_POINT('Origin',(0.0125,0.001,-4.59242549680257E-18));
#48751=CARTESIAN_POINT('',(-0.00501982557395217,0.001,-0.0013));
#48752=CARTESIAN_POINT('Origin',(-0.00501982557395217,0.001,-2.16840434497101E-19));
#48753=CARTESIAN_POINT('',(-7.34788079488411E-20,0.001,-0.0116));
#48754=CARTESIAN_POINT('Origin',(0.,0.001,-0.011));
#48755=CARTESIAN_POINT('',(-7.34788079488411E-20,0.001,0.0104));
#48756=CARTESIAN_POINT('Origin',(0.,0.001,0.011));
#48757=CARTESIAN_POINT('Origin',(0.00625,0.,-2.29621274840129E-18));
#48758=CARTESIAN_POINT('',(0.00625,0.,0.0118531641345254));
#48759=CARTESIAN_POINT('',(0.00625,0.,-0.0118531641345254));
#48760=CARTESIAN_POINT('Origin',(0.,0.,0.));
#48761=CARTESIAN_POINT('Origin',(0.0125,0.,-4.59242549680257E-18));
#48762=CARTESIAN_POINT('',(0.0125,0.,-0.00910000000000001));
#48763=CARTESIAN_POINT('Origin',(0.0125,0.,-4.59242549680257E-18));
#48764=CARTESIAN_POINT('',(-0.00501982557395217,0.,-0.0013));
#48765=CARTESIAN_POINT('Origin',(-0.00501982557395217,0.,-2.16840434497101E-19));
#48766=CARTESIAN_POINT('',(-7.34788079488411E-20,0.,-0.0116));
#48767=CARTESIAN_POINT('Origin',(0.,0.,-0.011));
#48768=CARTESIAN_POINT('',(-7.34788079488411E-20,0.,0.0104));
#48769=CARTESIAN_POINT('Origin',(0.,0.,0.011));
#48770=CARTESIAN_POINT('Origin',(0.0125,0.0254,-4.59242549680257E-18));
#48771=CARTESIAN_POINT('',(0.0125,0.0009,0.00899999999999999));
#48772=CARTESIAN_POINT('',(0.0125,0.0009,-0.009));
#48773=CARTESIAN_POINT('Origin',(0.0125,0.0009,-4.59242549680257E-18));
#48774=CARTESIAN_POINT('Origin',(0.0125,0.0009,-4.59242549680257E-18));
#48775=CARTESIAN_POINT('',(0.0125,0.0001,0.00899999999999999));
#48776=CARTESIAN_POINT('',(0.0125,0.0254,0.00899999999999999));
#48777=CARTESIAN_POINT('',(0.0125,0.0001,-0.009));
#48778=CARTESIAN_POINT('Origin',(0.0125,0.0001,-4.59242549680257E-18));
#48779=CARTESIAN_POINT('Origin',(0.0125,0.0001,-4.59242549680257E-18));
#48780=CARTESIAN_POINT('Origin',(-0.00501982557395217,0.0254,-2.16840434497101E-19));
#48781=CARTESIAN_POINT('',(-0.00501982557395217,0.0009,0.0012));
#48782=CARTESIAN_POINT('',(-0.00501982557395217,0.0009,-0.0012));
#48783=CARTESIAN_POINT('Origin',(-0.00501982557395217,0.0009,-2.16840434497101E-19));
#48784=CARTESIAN_POINT('Origin',(-0.00501982557395217,0.0009,-2.16840434497101E-19));
#48785=CARTESIAN_POINT('',(-0.00501982557395217,0.0001,0.0012));
#48786=CARTESIAN_POINT('',(-0.00501982557395217,0.0254,0.0012));
#48787=CARTESIAN_POINT('',(-0.00501982557395217,0.0001,-0.0012));
#48788=CARTESIAN_POINT('Origin',(-0.00501982557395217,0.0001,-2.16840434497101E-19));
#48789=CARTESIAN_POINT('Origin',(-0.00501982557395217,0.0001,-2.16840434497101E-19));
#48790=CARTESIAN_POINT('Origin',(0.,0.0254,-0.011));
#48791=CARTESIAN_POINT('',(0.,0.0009,-0.0105));
#48792=CARTESIAN_POINT('',(-6.12323399573675E-20,0.0009,-0.0115));
#48793=CARTESIAN_POINT('Origin',(0.,0.0009,-0.011));
#48794=CARTESIAN_POINT('Origin',(0.,0.0009,-0.011));
#48795=CARTESIAN_POINT('',(0.,0.0001,-0.0105));
#48796=CARTESIAN_POINT('',(-6.12323399573677E-20,0.0254,-0.0105));
#48797=CARTESIAN_POINT('',(-6.12323399573675E-20,0.0001,-0.0115));
#48798=CARTESIAN_POINT('Origin',(0.,0.0001,-0.011));
#48799=CARTESIAN_POINT('Origin',(0.,0.0001,-0.011));
#48800=CARTESIAN_POINT('Origin',(0.,0.0254,0.011));
#48801=CARTESIAN_POINT('',(0.,0.0009,0.0115));
#48802=CARTESIAN_POINT('',(-6.12323399573675E-20,0.0009,0.0105));
#48803=CARTESIAN_POINT('Origin',(0.,0.0009,0.011));
#48804=CARTESIAN_POINT('Origin',(0.,0.0009,0.011));
#48805=CARTESIAN_POINT('',(0.,0.0001,0.0115));
#48806=CARTESIAN_POINT('',(-6.12323399573677E-20,0.0254,0.0115));
#48807=CARTESIAN_POINT('',(-6.12323399573675E-20,0.0001,0.0105));
#48808=CARTESIAN_POINT('Origin',(0.,0.0001,0.011));
#48809=CARTESIAN_POINT('Origin',(0.,0.0001,0.011));
#48810=CARTESIAN_POINT('Origin',(0.,0.0001,0.));
#48811=CARTESIAN_POINT('Ctrl Pts',(0.00624999999999999,0.0001,-0.0119660979437743));
#48812=CARTESIAN_POINT('Ctrl Pts',(0.00624999999999999,8.83792829537417E-5,
-0.0119660979437743));
#48813=CARTESIAN_POINT('Ctrl Pts',(0.00625000000000008,7.69379006756195E-5,
-0.0119638141731892));
#48814=CARTESIAN_POINT('Ctrl Pts',(0.00625000000000009,5.47630188197498E-5,
-0.0119548176774847));
#48815=CARTESIAN_POINT('Ctrl Pts',(0.00625000000004375,4.4420733774185E-5,
-0.0119479855235934));
#48816=CARTESIAN_POINT('Ctrl Pts',(0.00625000000005384,2.54794304335682E-5,
-0.0119299406248958));
#48817=CARTESIAN_POINT('Ctrl Pts',(0.00624999999999999,1.74353766384864E-5,
-0.0119184732907306));
#48818=CARTESIAN_POINT('Ctrl Pts',(0.00624999999999999,7.85927944026424E-6,
-0.0118979845239147));
#48819=CARTESIAN_POINT('Ctrl Pts',(0.00625000000002098,5.03563170544993E-6,
-0.011889655603743));
#48820=CARTESIAN_POINT('Ctrl Pts',(0.00625000000003952,1.15383481991825E-6,
-0.011872472207609));
#48821=CARTESIAN_POINT('Ctrl Pts',(0.00624999999999998,1.2088148348863E-7,
-0.011863625630709));
#48822=CARTESIAN_POINT('Ctrl Pts',(0.00625,3.33322623339041E-9,-0.011854229961993));
#48823=CARTESIAN_POINT('Ctrl Pts',(0.00625,2.88647381170633E-23,-0.0118536970486924));
#48824=CARTESIAN_POINT('Ctrl Pts',(0.00625,0.,-0.0118531641345254));
#48825=CARTESIAN_POINT('Ctrl Pts',(0.00625,0.0001,0.0119660979437743));
#48826=CARTESIAN_POINT('Ctrl Pts',(0.00625,8.83792829537419E-5,0.0119660979437743));
#48827=CARTESIAN_POINT('Ctrl Pts',(0.00625000000000009,7.69379006756203E-5,
0.0119638141731892));
#48828=CARTESIAN_POINT('Ctrl Pts',(0.0062500000000001,5.47630188197589E-5,
0.0119548176774847));
#48829=CARTESIAN_POINT('Ctrl Pts',(0.00625000000004376,4.44207337741988E-5,
0.0119479855235934));
#48830=CARTESIAN_POINT('Ctrl Pts',(0.00625000000005385,2.54794304335679E-5,
0.0119299406248958));
#48831=CARTESIAN_POINT('Ctrl Pts',(0.00625,1.74353766384861E-5,0.0119184732907306));
#48832=CARTESIAN_POINT('Ctrl Pts',(0.00624999999999999,7.85927944026339E-6,
0.0118979845239147));
#48833=CARTESIAN_POINT('Ctrl Pts',(0.00625000000002099,5.03563170544918E-6,
0.011889655603743));
#48834=CARTESIAN_POINT('Ctrl Pts',(0.00625000000003952,1.15383481991727E-6,
0.011872472207609));
#48835=CARTESIAN_POINT('Ctrl Pts',(0.00624999999999998,1.20881483488571E-7,
0.011863625630709));
#48836=CARTESIAN_POINT('Ctrl Pts',(0.00625000000000001,3.33322623339041E-9,
0.011854229961993));
#48837=CARTESIAN_POINT('Ctrl Pts',(0.00625,2.88647381170633E-23,0.0118536970486924));
#48838=CARTESIAN_POINT('Ctrl Pts',(0.00625,0.,0.0118531641345254));
#48839=CARTESIAN_POINT('Origin',(0.0125,0.0001,-4.59242549680257E-18));
#48840=CARTESIAN_POINT('Origin',(0.0125,0.0001,-4.59242549680257E-18));
#48841=CARTESIAN_POINT('Origin',(0.0125,0.0001,-0.00910000000000001));
#48842=CARTESIAN_POINT('Origin',(-0.00501982557395217,0.0001,-2.16840434497101E-19));
#48843=CARTESIAN_POINT('Origin',(-0.00501982557395217,0.0001,-0.0013));
#48844=CARTESIAN_POINT('Origin',(0.,0.0001,-0.011));
#48845=CARTESIAN_POINT('Origin',(-7.34788079488411E-20,0.0001,-0.0116));
#48846=CARTESIAN_POINT('Origin',(0.,0.0001,0.011));
#48847=CARTESIAN_POINT('Origin',(-7.34788079488411E-20,0.0001,0.0104));
#48848=CARTESIAN_POINT('Origin',(0.,0.0009,0.));
#48849=CARTESIAN_POINT('Ctrl Pts',(0.00624999999999999,0.0009,-0.0119660979437743));
#48850=CARTESIAN_POINT('Ctrl Pts',(0.00624999999999999,0.000911620717046258,
-0.0119660979437743));
#48851=CARTESIAN_POINT('Ctrl Pts',(0.00625000000000008,0.00092306209932438,
-0.0119638141731892));
#48852=CARTESIAN_POINT('Ctrl Pts',(0.00625000000000009,0.00094523698118025,
-0.0119548176774847));
#48853=CARTESIAN_POINT('Ctrl Pts',(0.00625000000004375,0.000955579266225815,
-0.0119479855235934));
#48854=CARTESIAN_POINT('Ctrl Pts',(0.00625000000005384,0.000974520569566432,
-0.0119299406248958));
#48855=CARTESIAN_POINT('Ctrl Pts',(0.00624999999999999,0.000982564623361514,
-0.0119184732907306));
#48856=CARTESIAN_POINT('Ctrl Pts',(0.00624999999999999,0.000992140720559736,
-0.0118979845239147));
#48857=CARTESIAN_POINT('Ctrl Pts',(0.00625000000002098,0.00099496436829455,
-0.011889655603743));
#48858=CARTESIAN_POINT('Ctrl Pts',(0.00625000000003952,0.000998846165180082,
-0.011872472207609));
#48859=CARTESIAN_POINT('Ctrl Pts',(0.00624999999999993,0.000999879118516512,
-0.011863625630709));
#48860=CARTESIAN_POINT('Ctrl Pts',(0.00625000000000001,0.000999996666773766,
-0.011854229961993));
#48861=CARTESIAN_POINT('Ctrl Pts',(0.00625,0.001,-0.0118536970486924));
#48862=CARTESIAN_POINT('Ctrl Pts',(0.00625,0.001,-0.0118531641345254));
#48863=CARTESIAN_POINT('Ctrl Pts',(0.00625,0.0009,0.0119660979437743));
#48864=CARTESIAN_POINT('Ctrl Pts',(0.00625,0.000911620717046258,0.0119660979437743));
#48865=CARTESIAN_POINT('Ctrl Pts',(0.00625000000000009,0.00092306209932438,
0.0119638141731892));
#48866=CARTESIAN_POINT('Ctrl Pts',(0.0062500000000001,0.000945236981180241,
0.0119548176774847));
#48867=CARTESIAN_POINT('Ctrl Pts',(0.00625000000004376,0.000955579266225801,
0.0119479855235934));
#48868=CARTESIAN_POINT('Ctrl Pts',(0.00625000000005385,0.000974520569566438,
0.0119299406248958));
#48869=CARTESIAN_POINT('Ctrl Pts',(0.00625,0.00098256462336152,0.0119184732907305));
#48870=CARTESIAN_POINT('Ctrl Pts',(0.00625000000000001,0.00099214072055973,
0.0118979845239147));
#48871=CARTESIAN_POINT('Ctrl Pts',(0.00625000000002099,0.000994964368294546,
0.011889655603743));
#48872=CARTESIAN_POINT('Ctrl Pts',(0.00625000000003952,0.000998846165180083,
0.011872472207609));
#48873=CARTESIAN_POINT('Ctrl Pts',(0.00624999999999998,0.000999879118516511,
0.011863625630709));
#48874=CARTESIAN_POINT('Ctrl Pts',(0.00625000000000001,0.000999996666773767,
0.011854229961993));
#48875=CARTESIAN_POINT('Ctrl Pts',(0.00625,0.001,0.0118536970486924));
#48876=CARTESIAN_POINT('Ctrl Pts',(0.00625,0.001,0.0118531641345254));
#48877=CARTESIAN_POINT('Origin',(0.0125,0.0009,-4.59242549680257E-18));
#48878=CARTESIAN_POINT('Origin',(0.0125,0.0009,-4.59242549680257E-18));
#48879=CARTESIAN_POINT('Origin',(0.0125,0.0009,-0.00910000000000001));
#48880=CARTESIAN_POINT('Origin',(-0.00501982557395217,0.0009,-2.16840434497101E-19));
#48881=CARTESIAN_POINT('Origin',(-0.00501982557395217,0.0009,-0.0013));
#48882=CARTESIAN_POINT('Origin',(0.,0.0009,-0.011));
#48883=CARTESIAN_POINT('Origin',(-7.34788079488411E-20,0.0009,-0.0116));
#48884=CARTESIAN_POINT('Origin',(0.,0.0009,0.011));
#48885=CARTESIAN_POINT('Origin',(-7.34788079488411E-20,0.0009,0.0104));
#48886=CARTESIAN_POINT('',(0.,0.,0.));
#48887=CARTESIAN_POINT('Origin',(0.0026795695442083,0.0119999999976374,
0.00311832636829977));
#48888=CARTESIAN_POINT('',(0.0011104902728708,0.0118999999786958,0.00129548235688735));
#48889=CARTESIAN_POINT('',(0.0011104897024608,0.000100000021359172,0.00129548157965629));
#48890=CARTESIAN_POINT('',(0.00111150801408478,0.0119,0.00129670923842467));
#48891=CARTESIAN_POINT('',(0.00320791856642742,0.000100000046696322,0.000774301462227049));
#48892=CARTESIAN_POINT('Origin',(0.00266641386133884,0.000100000326685605,
0.00308004099065544));
#48893=CARTESIAN_POINT('',(0.00320786705247145,0.0118999999521473,0.000774537053797754));
#48894=CARTESIAN_POINT('',(0.00320887657816064,0.0001,0.000769953068500355));
#48895=CARTESIAN_POINT('Origin',(0.00266641994550595,0.0118999996733985,
0.00308005675377107));
#48896=CARTESIAN_POINT('Origin',(0.00334795260328877,0.012,0.000799258762279974));
#48897=CARTESIAN_POINT('',(0.00332640074788228,0.0001,0.000656753759343362));
#48898=CARTESIAN_POINT('',(0.00317081887252197,0.0001,-0.000371983450837843));
#48899=CARTESIAN_POINT('',(0.00316646966616483,0.0001,-0.000400741237720026));
#48900=CARTESIAN_POINT('',(0.00317081887252197,0.0119,-0.000371983450837843));
#48901=CARTESIAN_POINT('',(0.00317081887252197,0.012,-0.000371983450837842));
#48902=CARTESIAN_POINT('',(0.00332640074788228,0.0119,0.000656753759343362));
#48903=CARTESIAN_POINT('',(0.00334795260328877,0.0119,0.000799258762279974));
#48904=CARTESIAN_POINT('',(0.00332640074788228,0.012,0.000656753759343362));
#48905=CARTESIAN_POINT('Origin',(0.00200017452605719,0.012,-0.00174080634098864));
#48906=CARTESIAN_POINT('',(0.00314737531812273,0.0119,-0.000422680512437861));
#48907=CARTESIAN_POINT('',(0.00314737531812273,0.0001,-0.000422680512437861));
#48908=CARTESIAN_POINT('',(0.00314737531812273,0.012,-0.000422680512437861));
#48909=CARTESIAN_POINT('',(0.00200017452605719,0.0001,-0.00174080634098864));
#48910=CARTESIAN_POINT('',(0.00200017452605719,0.0001,-0.00174080634098864));
#48911=CARTESIAN_POINT('',(0.00200017452605719,0.0119,-0.00174080634098864));
#48912=CARTESIAN_POINT('',(0.00200017452605719,0.012,-0.00174080634098864));
#48913=CARTESIAN_POINT('',(0.00200017452605719,0.0119,-0.00174080634098864));
#48914=CARTESIAN_POINT('Origin',(0.,0.012,0.));
#48915=CARTESIAN_POINT('',(-0.00200017452605719,0.0001,-0.00174080634098864));
#48916=CARTESIAN_POINT('Origin',(0.,0.0001,0.));
#48917=CARTESIAN_POINT('',(-0.00200017452605719,0.0119,-0.00174080634098864));
#48918=CARTESIAN_POINT('',(-0.00200017452605719,0.012,-0.00174080634098864));
#48919=CARTESIAN_POINT('Origin',(0.,0.0119,0.));
#48920=CARTESIAN_POINT('Origin',(-0.00200017452605719,0.012,-0.00174080634098864));
#48921=CARTESIAN_POINT('',(-0.00314737531812273,0.0001,-0.000422680512437861));
#48922=CARTESIAN_POINT('',(-0.00316646966616483,0.0001,-0.000400741237720025));
#48923=CARTESIAN_POINT('',(-0.00314737531812273,0.0119,-0.000422680512437861));
#48924=CARTESIAN_POINT('',(-0.00314737531812273,0.012,-0.000422680512437861));
#48925=CARTESIAN_POINT('',(-0.00200017452605719,0.0119,-0.00174080634098864));
#48926=CARTESIAN_POINT('Origin',(-0.00334795260328877,0.012,0.000799258762279975));
#48927=CARTESIAN_POINT('',(-0.00332640074788227,0.0119,0.000656753759343363));
#48928=CARTESIAN_POINT('',(-0.00317081887252197,0.0119,-0.000371983450837842));
#48929=CARTESIAN_POINT('',(-0.00334795260328877,0.0119,0.000799258762279975));
#48930=CARTESIAN_POINT('',(-0.00317081887252197,0.0001,-0.000371983450837842));
#48931=CARTESIAN_POINT('',(-0.00317081887252197,0.012,-0.000371983450837842));
#48932=CARTESIAN_POINT('',(-0.00332640074788227,0.0001,0.000656753759343363));
#48933=CARTESIAN_POINT('',(-0.00334795260328877,0.0001,0.000799258762279975));
#48934=CARTESIAN_POINT('',(-0.00332640074788227,0.012,0.000656753759343363));
#48935=CARTESIAN_POINT('Origin',(-0.00267956954438675,0.0119999999976374,
0.00311832636876968));
#48936=CARTESIAN_POINT('',(-0.00320791856642536,0.0118999999533037,0.000774301462240489));
#48937=CARTESIAN_POINT('',(-0.00320791920421998,0.000100000046677651,0.000774298724656522));
#48938=CARTESIAN_POINT('',(-0.00320887657816269,0.0119,0.000769953068500743));
#48939=CARTESIAN_POINT('',(-0.00111049188113299,0.000100000455445466,0.00129548100148887));
#48940=CARTESIAN_POINT('Origin',(-0.00266641994549533,0.000100000326601476,
0.0030800567537451));
#48941=CARTESIAN_POINT('',(-0.00111049131362328,0.0118999995438595,0.0012954802219009));
#48942=CARTESIAN_POINT('',(-0.00111150801408489,0.0001,0.00129670923842458));
#48943=CARTESIAN_POINT('Origin',(-0.00266641386137086,0.0118999996733144,
0.00308004099074208));
#48944=CARTESIAN_POINT('Origin',(0.,0.012,0.));
#48945=CARTESIAN_POINT('Origin',(0.,0.0001,0.));
#48946=CARTESIAN_POINT('Origin',(0.,0.0119,0.));
#48947=CARTESIAN_POINT('Origin',(0.00213706124849222,0.012,0.000772521431045073));
#48948=CARTESIAN_POINT('',(-0.00322752330024893,0.0119998704155119,0.000671715368343072));
#48949=CARTESIAN_POINT('',(-0.00308038924536576,0.0120000000376982,0.000647274389139154));
#48950=CARTESIAN_POINT('Ctrl Pts',(-0.00322752354088739,0.0119998703308515,
0.000671713719076399));
#48951=CARTESIAN_POINT('Ctrl Pts',(-0.00317812331295772,0.0119999770854659,
0.000662354121866401));
#48952=CARTESIAN_POINT('Ctrl Pts',(-0.00312908474940071,0.0120000000376982,
0.000654218836705111));
#48953=CARTESIAN_POINT('Ctrl Pts',(-0.00308038924536576,0.0120000000376982,
0.000647274389139154));
#48954=CARTESIAN_POINT('',(-0.00104643070386136,0.0119999950205632,0.0012207818227995));
#48955=CARTESIAN_POINT('Ctrl Pts',(-0.00308038924536576,0.0120000000376982,
0.000647274389139154));
#48956=CARTESIAN_POINT('Ctrl Pts',(-0.00280336974579476,0.0120000000376982,
0.000607768742208423));
#48957=CARTESIAN_POINT('Ctrl Pts',(-0.00253662303677809,0.0119999551733919,
0.000605951286767472));
#48958=CARTESIAN_POINT('Ctrl Pts',(-0.00228179200572747,0.0119999881420702,
0.000644022735642257));
#48959=CARTESIAN_POINT('Ctrl Pts',(-0.00192078189626786,0.0120000348476307,
0.000697957210846894));
#48960=CARTESIAN_POINT('Ctrl Pts',(-0.00158393163555709,0.0119999540372077,
0.0008335151744178));
#48961=CARTESIAN_POINT('Ctrl Pts',(-0.00127112647954639,0.011999958801516,
0.00104811133060204));
#48962=CARTESIAN_POINT('Ctrl Pts',(-0.00119465884940102,0.0119999599661878,
0.0011005710141667));
#48963=CARTESIAN_POINT('Ctrl Pts',(-0.00111968086511865,0.0119999715654864,
0.00115799258041393));
#48964=CARTESIAN_POINT('Ctrl Pts',(-0.00104643062837067,0.0119999850616897,
0.00122078173615864));
#48965=CARTESIAN_POINT('',(0.00104643070371687,0.0119999950154752,0.00122078182263315));
#48966=CARTESIAN_POINT('Origin',(0.,0.012,0.));
#48967=CARTESIAN_POINT('',(0.00308076069387804,0.012,0.000647255039318342));
#48968=CARTESIAN_POINT('Origin',(0.024699859933188,0.012,0.0685450159411535));
#48969=CARTESIAN_POINT('',(0.00322751928435601,0.0119998716555966,0.000671736604513569));
#48970=CARTESIAN_POINT('Origin',(0.024699859933188,0.012,0.0685450159411535));
#48971=CARTESIAN_POINT('',(0.00307194323441727,0.012,-0.000357029916493473));
#48972=CARTESIAN_POINT('',(0.00321804722080344,0.012,0.000609037673341061));
#48973=CARTESIAN_POINT('',(0.00192474244235174,0.012,-0.00167515574504426));
#48974=CARTESIAN_POINT('',(0.00322838106972541,0.012,-0.00017728391848822));
#48975=CARTESIAN_POINT('',(-0.00192474244235174,0.012,-0.00167515574504426));
#48976=CARTESIAN_POINT('Origin',(0.,0.012,0.));
#48977=CARTESIAN_POINT('',(-0.00307194323441727,0.012,-0.000357029916493472));
#48978=CARTESIAN_POINT('',(-0.00138623395388341,0.012,-0.00229389829861756));
#48979=CARTESIAN_POINT('',(-0.00312247434152602,0.012,-2.29085412752433E-5));
#48980=CARTESIAN_POINT('',(-1.34711147906209E-19,0.012,0.0011));
#48981=CARTESIAN_POINT('Origin',(0.,0.012,0.));
#48982=CARTESIAN_POINT('Origin',(0.00213706124849222,0.,0.000772521431045073));
#48983=CARTESIAN_POINT('',(0.00192474244235174,0.,-0.00167515574504426));
#48984=CARTESIAN_POINT('',(0.00307194323441727,0.,-0.000357029916493473));
#48985=CARTESIAN_POINT('',(0.00309103758245938,0.,-0.000335090641775636));
#48986=CARTESIAN_POINT('',(0.00322752330024892,1.29584488918668E-7,0.000671715368343146));
#48987=CARTESIAN_POINT('',(0.00324907696518407,0.,0.000814212296624345));
#48988=CARTESIAN_POINT('',(0.00308038924492918,-3.76981371119633E-11,0.000647274389076851));
#48989=CARTESIAN_POINT('Ctrl Pts',(0.00322752354088737,1.29669149337175E-7,
0.000671713719076455));
#48990=CARTESIAN_POINT('Ctrl Pts',(0.00317812331281008,2.29145342387538E-8,
0.000662354121838435));
#48991=CARTESIAN_POINT('Ctrl Pts',(0.0031290847491076,-3.7698137119178E-11,
0.000654218836656452));
#48992=CARTESIAN_POINT('Ctrl Pts',(0.00308038924492918,-3.76981371195528E-11,
0.000647274389076851));
#48993=CARTESIAN_POINT('',(0.00104643062837068,1.49383102941193E-8,0.00122078173615864));
#48994=CARTESIAN_POINT('Ctrl Pts',(0.00308038924492918,-3.76981371195528E-11,
0.000647274389076851));
#48995=CARTESIAN_POINT('Ctrl Pts',(0.00280336974551912,-3.76981371216846E-11,
0.000607768742207853));
#48996=CARTESIAN_POINT('Ctrl Pts',(0.00253662303665133,4.48266081172561E-8,
0.000605951286787511));
#48997=CARTESIAN_POINT('Ctrl Pts',(0.00228179200573768,1.18579298942923E-8,
0.000644022735640731));
#48998=CARTESIAN_POINT('Ctrl Pts',(0.00192078189628118,-3.48476306147057E-8,
0.000697957210843341));
#48999=CARTESIAN_POINT('Ctrl Pts',(0.00158393163557307,4.59627924215703E-8,
0.000833515174410873));
#49000=CARTESIAN_POINT('Ctrl Pts',(0.00127112647956448,4.11984840427545E-8,
0.00104811133058969));
#49001=CARTESIAN_POINT('Ctrl Pts',(0.00119465884941284,4.00338121566248E-8,
0.00110057101415767));
#49002=CARTESIAN_POINT('Ctrl Pts',(0.00111968086512442,2.84345135863231E-8,
0.00115799258040899));
#49003=CARTESIAN_POINT('Ctrl Pts',(0.00104643062837068,1.49383102941041E-8,
0.00122078173615864));
#49004=CARTESIAN_POINT('',(-0.00104643079757785,0.,0.00122078193166094));
#49005=CARTESIAN_POINT('Origin',(0.,0.,0.));
#49006=CARTESIAN_POINT('',(-0.0030807606937324,0.,0.000647255039297434));
#49007=CARTESIAN_POINT('Origin',(-0.0246998599330348,0.,0.0685450159406926));
#49008=CARTESIAN_POINT('',(-0.00322751928435599,1.28344403638389E-7,0.00067173660451365));
#49009=CARTESIAN_POINT('Origin',(-0.0246998599330348,0.,0.0685450159406926));
#49010=CARTESIAN_POINT('',(-0.00307194323441727,0.,-0.000357029916493471));
#49011=CARTESIAN_POINT('',(-0.00306759402806013,0.,-0.000385787703375655));
#49012=CARTESIAN_POINT('',(-0.00192474244235174,0.,-0.00167515574504426));
#49013=CARTESIAN_POINT('',(-0.00192474244235174,0.,-0.00167515574504426));
#49014=CARTESIAN_POINT('Origin',(0.,0.,0.));
#49015=CARTESIAN_POINT('',(-1.34711147906209E-19,0.,0.0011));
#49016=CARTESIAN_POINT('Origin',(0.,0.,0.));
#49017=CARTESIAN_POINT('Origin',(0.,0.,0.));
#49018=CARTESIAN_POINT('',(0.,0.0001,-0.001));
#49019=CARTESIAN_POINT('',(-1.22464679914735E-19,0.0001,0.001));
#49020=CARTESIAN_POINT('Origin',(0.,0.0001,0.));
#49021=CARTESIAN_POINT('Origin',(0.,0.0001,0.));
#49022=CARTESIAN_POINT('',(0.,0.0119,-0.001));
#49023=CARTESIAN_POINT('',(-1.22464679914735E-19,0.,-0.001));
#49024=CARTESIAN_POINT('',(-1.22464679914735E-19,0.0119,0.001));
#49025=CARTESIAN_POINT('Origin',(0.,0.0119,0.));
#49026=CARTESIAN_POINT('Origin',(0.,0.0119,0.));
#49027=CARTESIAN_POINT('Origin',(-0.00312247434152602,0.0119,-2.29085412752431E-5));
#49028=CARTESIAN_POINT('Origin',(-0.00322752510977757,0.0119,0.000671707293687733));
#49029=CARTESIAN_POINT('Origin',(-0.00307194323441727,0.0119,-0.000357029916493472));
#49030=CARTESIAN_POINT('Origin',(-0.00322752510977757,0.0119,0.000671707293687733));
#49031=CARTESIAN_POINT('Ctrl Pts',(-0.00320773952081963,0.0118999999536822,
0.000775013487105381));
#49032=CARTESIAN_POINT('Ctrl Pts',(-0.00320773942939966,0.0119447930614053,
0.000775013876381884));
#49033=CARTESIAN_POINT('Ctrl Pts',(-0.00321413964601594,0.011986412579691,
0.000741829045057959));
#49034=CARTESIAN_POINT('Ctrl Pts',(-0.00322198939913603,0.0119969554905399,
0.000700795898891431));
#49035=CARTESIAN_POINT('Ctrl Pts',(-0.00322381747770655,0.0119994107613107,
0.00069123995311325));
#49036=CARTESIAN_POINT('Ctrl Pts',(-0.00322569246909101,0.0120003720874417,
0.000681395742799694));
#49037=CARTESIAN_POINT('Ctrl Pts',(-0.00322752330024893,0.0119998704155119,
0.000671715368343072));
#49038=CARTESIAN_POINT('Origin',(-0.00322752510977757,0.0119,0.000671707293687733));
#49039=CARTESIAN_POINT('Origin',(-0.00307194323441727,0.0119,-0.000357029916493472));
#49040=CARTESIAN_POINT('Origin',(-0.00307194323441727,0.0119,-0.000357029916493472));
#49041=CARTESIAN_POINT('Origin',(-0.00307194323441727,0.0119,-0.000357029916493472));
#49042=CARTESIAN_POINT('Origin',(-0.00322752510977757,0.006,0.000671707293687733));
#49043=CARTESIAN_POINT('Origin',(-0.00322752510977757,0.0001,0.000671707293687733));
#49044=CARTESIAN_POINT('Origin',(-0.00266641386136991,0.0119000008463731,
0.00308004099073934));
#49045=CARTESIAN_POINT('Ctrl Pts',(-0.00111150052572481,0.0119000008612573,
0.0012967156572246));
#49046=CARTESIAN_POINT('Ctrl Pts',(-0.00111167480720489,0.0119448666404984,
0.00129656576013425));
#49047=CARTESIAN_POINT('Ctrl Pts',(-0.00108952702596546,0.0119871861227217,
0.00127080632163187));
#49048=CARTESIAN_POINT('Ctrl Pts',(-0.00106139371099157,0.0119973373095639,
0.00123814749532547));
#49049=CARTESIAN_POINT('Ctrl Pts',(-0.00105648554162436,0.0119991082968914,
0.00123244980022645));
#49050=CARTESIAN_POINT('Ctrl Pts',(-0.00105145244004021,0.0119999999999997,
0.00122660881996128));
#49051=CARTESIAN_POINT('Ctrl Pts',(-0.00104643079716415,0.012,0.00122078193201883));
#49052=CARTESIAN_POINT('Origin',(-0.00138623395388341,0.0119,-0.00229389829861756));
#49053=CARTESIAN_POINT('Origin',(-0.00192474244235174,0.0119,-0.00167515574504426));
#49054=CARTESIAN_POINT('Origin',(-0.00307194323441727,0.012,-0.000357029916493472));
#49055=CARTESIAN_POINT('Origin',(-0.00307194323441727,0.0001,-0.000357029916493472));
#49056=CARTESIAN_POINT('Origin',(-0.00324907696518407,0.0001,0.000814212296624346));
#49057=CARTESIAN_POINT('Origin',(-0.00322752510977757,0.0001,0.000671707293687733));
#49058=CARTESIAN_POINT('Origin',(-0.00307194323441727,0.0001,-0.000357029916493471));
#49059=CARTESIAN_POINT('Origin',(-0.00322752510977757,9.99999999999988E-5,
0.000671707293687733));
#49060=CARTESIAN_POINT('Ctrl Pts',(-0.00322751928435599,1.2834440363839E-7,
0.00067173660451365));
#49061=CARTESIAN_POINT('Ctrl Pts',(-0.00321965722956229,-2.01559019057911E-6,
0.000713306122590413));
#49062=CARTESIAN_POINT('Ctrl Pts',(-0.00321120798733041,2.68608144209912E-5,
0.000756802444556823));
#49063=CARTESIAN_POINT('Ctrl Pts',(-0.00320864134773808,6.92989875928505E-5,
0.000770261872992935));
#49064=CARTESIAN_POINT('Ctrl Pts',(-0.00320804412466433,7.91737889874055E-5,
0.000773393703907348));
#49065=CARTESIAN_POINT('Ctrl Pts',(-0.00320774016282151,8.95773685078349E-5,
0.000775010844451836));
#49066=CARTESIAN_POINT('Ctrl Pts',(-0.00320774018409717,0.000100000046301422,
0.00077501075385594));
#49067=CARTESIAN_POINT('Origin',(0.,0.0119,0.));
#49068=CARTESIAN_POINT('Origin',(0.00104528387395555,0.0118999989257993,
0.00121948624514362));
#49069=CARTESIAN_POINT('Origin',(0.,0.0119,0.));
#49070=CARTESIAN_POINT('Origin',(0.00192474244235174,0.0119,-0.00167515574504426));
#49071=CARTESIAN_POINT('Origin',(-0.00307194323441727,0.0001,-0.000357029916493472));
#49072=CARTESIAN_POINT('Origin',(-0.00307194323441727,0.0001,-0.000357029916493472));
#49073=CARTESIAN_POINT('Origin',(-0.00266641994549438,9.9999153442383E-5,
0.00308005675374236));
#49074=CARTESIAN_POINT('Ctrl Pts',(-0.00104643079716283,0.,0.00122078193201997));
#49075=CARTESIAN_POINT('Ctrl Pts',(-0.00107521420056969,1.64668732167874E-15,
0.0012541809493851));
#49076=CARTESIAN_POINT('Ctrl Pts',(-0.00110310833148252,3.31402733155764E-5,
0.00128656285040545));
#49077=CARTESIAN_POINT('Ctrl Pts',(-0.00110978851162454,7.67397954013635E-5,
0.00129457061122281));
#49078=CARTESIAN_POINT('Ctrl Pts',(-0.00111095398235606,8.43464715416405E-5,
0.00129596770092087));
#49079=CARTESIAN_POINT('Ctrl Pts',(-0.00111153092065892,9.21715553007715E-5,
0.00129668951490891));
#49080=CARTESIAN_POINT('Ctrl Pts',(-0.00111150052324074,9.9999138547178E-5,
0.00129671565935386));
#49081=CARTESIAN_POINT('Origin',(0.002666419945505,0.0119000008465576,0.00308005675376833));
#49082=CARTESIAN_POINT('Ctrl Pts',(0.00322751928435601,0.0119998716555966,
0.00067173660451357));
#49083=CARTESIAN_POINT('Ctrl Pts',(0.00321965722956182,0.0120020155901889,
0.000713306122592838));
#49084=CARTESIAN_POINT('Ctrl Pts',(0.00321120798733032,0.0119731391855723,
0.000756802444558106));
#49085=CARTESIAN_POINT('Ctrl Pts',(0.00320864134773872,0.011930701012399,
0.000770261872990747));
#49086=CARTESIAN_POINT('Ctrl Pts',(0.00320804412466531,0.0119208262110068,
0.000773393703903478));
#49087=CARTESIAN_POINT('Ctrl Pts',(0.00320774016282266,0.0119104226314893,
0.000775010844447059));
#49088=CARTESIAN_POINT('Ctrl Pts',(0.00320774018409833,0.0118999999536986,
0.000775010753851165));
#49089=CARTESIAN_POINT('Origin',(0.00321804722080344,0.0119,0.000609037673341061));
#49090=CARTESIAN_POINT('Origin',(0.00307194323441727,0.0119,-0.000357029916493473));
#49091=CARTESIAN_POINT('',(0.00331869935185679,0.0119386927171885,0.000657918485985577));
#49092=CARTESIAN_POINT('Origin',(0.00322752510977757,0.0119,0.000671707293687733));
#49093=CARTESIAN_POINT('Origin',(0.00322752510977757,0.0119,0.000671707293687733));
#49094=CARTESIAN_POINT('Origin',(0.00322838106972541,0.0119,-0.00017728391848822));
#49095=CARTESIAN_POINT('Origin',(0.00307194323441727,0.0119,-0.000357029916493473));
#49096=CARTESIAN_POINT('Origin',(-0.00192474244235174,0.0001,-0.00167515574504426));
#49097=CARTESIAN_POINT('Origin',(-0.00192474244235174,0.0001,-0.00167515574504426));
#49098=CARTESIAN_POINT('Origin',(0.,0.0001,0.));
#49099=CARTESIAN_POINT('Origin',(0.00104528444769579,0.000100001075468891,
0.00121948692081579));
#49100=CARTESIAN_POINT('Origin',(0.00322752510977757,0.0119,0.000671707293687733));
#49101=CARTESIAN_POINT('',(0.00328526013669653,0.011957735026919,0.000729442320606695));
#49102=CARTESIAN_POINT('Origin',(0.00322752510977757,0.0119,0.000671707293687733));
#49103=CARTESIAN_POINT('Origin',(0.00322752510977783,0.0119,0.000671707293687782));
#49104=CARTESIAN_POINT('Origin',(0.00307194323441727,0.0119,-0.000357029916493473));
#49105=CARTESIAN_POINT('Origin',(0.00307194323441727,0.0119,-0.000357029916493473));
#49106=CARTESIAN_POINT('Origin',(0.,0.0001,0.));
#49107=CARTESIAN_POINT('Origin',(0.00192474244235174,0.0001,-0.00167515574504426));
#49108=CARTESIAN_POINT('Origin',(0.00266641386133789,9.99991536269668E-5,
0.0030800409906527));
#49109=CARTESIAN_POINT('Ctrl Pts',(0.00320773952081613,0.000100000046317807,
0.000775013487119797));
#49110=CARTESIAN_POINT('Ctrl Pts',(0.00320773942939615,5.52069385949101E-5,
0.000775013876396265));
#49111=CARTESIAN_POINT('Ctrl Pts',(0.00321413964601276,1.35874203120974E-5,
0.000741829045073119));
#49112=CARTESIAN_POINT('Ctrl Pts',(0.00322198939913204,3.04450946169635E-6,
0.00070079589891201));
#49113=CARTESIAN_POINT('Ctrl Pts',(0.00322381747770392,5.89238688465402E-7,
0.000691239953126957));
#49114=CARTESIAN_POINT('Ctrl Pts',(0.00322569246908978,-3.72087442654418E-7,
0.000681395742806229));
#49115=CARTESIAN_POINT('Ctrl Pts',(0.00322752330024892,1.29584488918648E-7,
0.000671715368343146));
#49116=CARTESIAN_POINT('Origin',(0.00322752510977757,0.006,0.000671707293687733));
#49117=CARTESIAN_POINT('Origin',(0.00322752510977757,0.0001,0.000671707293687733));
#49118=CARTESIAN_POINT('Origin',(0.00307194323441727,0.012,-0.000357029916493473));
#49119=CARTESIAN_POINT('Origin',(0.00307194323441727,0.0001,-0.000357029916493473));
#49120=CARTESIAN_POINT('Origin',(0.00192474244235174,0.0001,-0.00167515574504426));
#49121=CARTESIAN_POINT('Origin',(0.00307194323441727,0.0001,-0.000357029916493473));
#49122=CARTESIAN_POINT('Origin',(0.00322752510977757,9.99999999999988E-5,
0.000671707293687733));
#49123=CARTESIAN_POINT('Origin',(0.00322752510977757,0.0001,0.000671707293687732));
#49124=CARTESIAN_POINT('Origin',(0.00307194323441727,0.0001,-0.000357029916493473));
#49125=CARTESIAN_POINT('Origin',(0.00307194323441727,0.0001,-0.000357029916493473));
#49126=CARTESIAN_POINT('Origin',(0.00324907696518407,0.0001,0.000814212296624345));
#49127=CARTESIAN_POINT('Origin',(0.,0.0001,0.));
#49128=CARTESIAN_POINT('Origin',(-1.34711147906209E-19,0.0001,0.0011));
#49129=CARTESIAN_POINT('Origin',(0.,0.0119,0.));
#49130=CARTESIAN_POINT('Origin',(-1.34711147906209E-19,0.0119,0.0011));
#49131=CARTESIAN_POINT('',(0.,0.,0.));
#49132=CARTESIAN_POINT('Ctrl Pts',(-0.047521969753009,0.00292791234232007,
0.0014375007351075));
#49133=CARTESIAN_POINT('Ctrl Pts',(-0.0475217905822521,0.00272283848633948,
0.00149851530284684));
#49134=CARTESIAN_POINT('Ctrl Pts',(-0.0475249292449862,0.00279751942631425,
0.00169899223914139));
#49135=CARTESIAN_POINT('Ctrl Pts',(-0.0471359306861318,0.00292980295225596,
0.00144284563795755));
#49136=CARTESIAN_POINT('Ctrl Pts',(-0.0471283033320531,0.0027246802372573,
0.00150425289890676));
#49137=CARTESIAN_POINT('Ctrl Pts',(-0.0470869890419856,0.00279975471284071,
0.00170530652254621));
#49138=CARTESIAN_POINT('Ctrl Pts',(-0.0463597555989418,0.00281040271795959,
0.00116400921661837));
#49139=CARTESIAN_POINT('Ctrl Pts',(-0.0463911712050714,0.00262787967136623,
0.00125349479954789));
#49140=CARTESIAN_POINT('Ctrl Pts',(-0.0462058670420217,0.0026583834282292,
0.00137542120560276));
#49141=CARTESIAN_POINT('Ctrl Pts',(-0.0458448108046749,0.00261243102946703,
2.73686784603569E-5));
#49142=CARTESIAN_POINT('Ctrl Pts',(-0.0458094820998151,0.00243981891809829,
3.02504277461982E-5));
#49143=CARTESIAN_POINT('Ctrl Pts',(-0.0456221070083461,0.00242419343546418,
3.23331464450899E-5));
#49144=CARTESIAN_POINT('Ctrl Pts',(-0.0463246614268507,0.00279922894991229,
-0.00113315917795547));
#49145=CARTESIAN_POINT('Ctrl Pts',(-0.0463534248332843,0.00261785874660286,
-0.00122287857653879));
#49146=CARTESIAN_POINT('Ctrl Pts',(-0.0461660653383145,0.00264516117224189,
-0.00133894667362545));
#49147=CARTESIAN_POINT('Ctrl Pts',(-0.047475667560966,0.00298937709191257,
-0.00158152248003427));
#49148=CARTESIAN_POINT('Ctrl Pts',(-0.0474776982153359,0.0027762552545778,
-0.00163733766341943));
#49149=CARTESIAN_POINT('Ctrl Pts',(-0.0474723735075983,0.00287024649410696,
-0.00186926883315251));
#49150=CARTESIAN_POINT('Ctrl Pts',(-0.0486390883124264,0.00281072577948571,
-0.00116572585728214));
#49151=CARTESIAN_POINT('Ctrl Pts',(-0.048607647449207,0.00262816948297617,
-0.00125530022942588));
#49152=CARTESIAN_POINT('Ctrl Pts',(-0.0487928212048197,0.00265876571215968,
-0.00137744992107542));
#49153=CARTESIAN_POINT('Ctrl Pts',(-0.0491553277660853,0.00261238743571346,
-2.56552014422379E-5));
#49154=CARTESIAN_POINT('Ctrl Pts',(-0.0491906502037132,0.00243978444592517,
-2.85609443699274E-5));
#49155=CARTESIAN_POINT('Ctrl Pts',(-0.0493780503329557,0.00242414178609795,
-3.03066921536269E-5));
#49156=CARTESIAN_POINT('Ctrl Pts',(-0.0486760035727277,0.00279905892909024,
0.00113193946402892));
#49157=CARTESIAN_POINT('Ctrl Pts',(-0.0486472257773982,0.00261770650436948,
0.00122160652879805));
#49158=CARTESIAN_POINT('Ctrl Pts',(-0.0488346894846697,0.00264495997721764,
0.00133750508047801));
#49159=CARTESIAN_POINT('Ctrl Pts',(-0.0479080088854605,0.00292602173206304,
0.00143215583134954));
#49160=CARTESIAN_POINT('Ctrl Pts',(-0.0479147483545036,0.00272099921368874,
0.00149278542731809));
#49161=CARTESIAN_POINT('Ctrl Pts',(-0.0479628751525174,0.00279528411067136,
0.00169267787348785));
#49162=CARTESIAN_POINT('Ctrl Pts',(-0.047521969753009,0.00292791234232007,
0.0014375007351075));
#49163=CARTESIAN_POINT('Ctrl Pts',(-0.0475217905822521,0.00272283848633948,
0.00149851530284684));
#49164=CARTESIAN_POINT('Ctrl Pts',(-0.0475249292449862,0.00279751942631425,
0.00169899223914139));
#49165=CARTESIAN_POINT('',(-0.0475248989283422,0.00279679729590145,0.00169705696579711));
#49166=CARTESIAN_POINT('',(-0.047521969610817,0.00292787381968359,0.00143750579808091));
#49167=CARTESIAN_POINT('Ctrl Pts',(-0.047524898940367,0.0027968083975309,
0.00169705296016689));
#49168=CARTESIAN_POINT('Ctrl Pts',(-0.0475217930237305,0.00272496362417165,
0.00149792539327892));
#49169=CARTESIAN_POINT('Ctrl Pts',(-0.0475219697209349,0.00292787557066265,
0.00143751167942811));
#49170=CARTESIAN_POINT('',(-0.0475,0.002796875,0.00169723753033423));
#49171=CARTESIAN_POINT('Ctrl Pts',(-0.0475,0.002796875,0.00169723753033423));
#49172=CARTESIAN_POINT('Ctrl Pts',(-0.0470556118872741,0.00279685666170104,
0.00169708273941662));
#49173=CARTESIAN_POINT('Ctrl Pts',(-0.0461665719179776,0.00264539629297986,
0.00133451307288424));
#49174=CARTESIAN_POINT('Ctrl Pts',(-0.0456341151866447,0.00242721165967408,
2.04143110301131E-6));
#49175=CARTESIAN_POINT('Ctrl Pts',(-0.0461678030184114,0.00264575759329887,
-0.00133706644457989));
#49176=CARTESIAN_POINT('Ctrl Pts',(-0.0475004674124815,0.00287245605236691,
-0.00187753708326946));
#49177=CARTESIAN_POINT('Ctrl Pts',(-0.0488323000379284,0.00264566812967151,
-0.00133621021713015));
#49178=CARTESIAN_POINT('Ctrl Pts',(-0.0493659912919883,0.00242720638772112,
8.03570479835991E-8));
#49179=CARTESIAN_POINT('Ctrl Pts',(-0.0488362194957707,0.00264414723702811,
0.00132712816164593));
#49180=CARTESIAN_POINT('Ctrl Pts',(-0.0479609366490351,0.00279406634542388,
0.00169058598422321));
#49181=CARTESIAN_POINT('Ctrl Pts',(-0.0475248989283412,0.00279679729590146,
0.00169705696579713));
#49182=CARTESIAN_POINT('',(-0.0475,0.00292794117647059,0.00143766002569487));
#49183=CARTESIAN_POINT('Ctrl Pts',(-0.0474999999943631,0.00279686254156731,
0.00169724202650596));
#49184=CARTESIAN_POINT('Ctrl Pts',(-0.047499419575665,0.00272498843318775,
0.00149808548501933));
#49185=CARTESIAN_POINT('Ctrl Pts',(-0.0475000000046904,0.00292793913822137,
0.00143765318065731));
#49186=CARTESIAN_POINT('',(-0.0464613877374918,0.00280559596990715,0.00103824715833725));
#49187=CARTESIAN_POINT('Ctrl Pts',(-0.0464613877374919,0.00280559596990715,
0.00103824715833725));
#49188=CARTESIAN_POINT('Ctrl Pts',(-0.0467365913194384,0.0028677273296309,
0.00129598001878092));
#49189=CARTESIAN_POINT('Ctrl Pts',(-0.0471182158646947,0.0029279629632896,
0.00143762672627057));
#49190=CARTESIAN_POINT('Ctrl Pts',(-0.0475,0.00292794117647059,0.00143766002569487));
#49191=CARTESIAN_POINT('',(-0.0460105501879809,0.00267652225571725,2.02991083324788E-5));
#49192=CARTESIAN_POINT('Ctrl Pts',(-0.0460105501879809,0.00267652225571725,
2.02991083324788E-5));
#49193=CARTESIAN_POINT('Ctrl Pts',(-0.0460158709169045,0.0026785745264266,
0.000396779691601982));
#49194=CARTESIAN_POINT('Ctrl Pts',(-0.0461825726657913,0.00274235049501108,
0.000774645398476074));
#49195=CARTESIAN_POINT('Ctrl Pts',(-0.0464582351392805,0.00280488422330797,
0.00103529469620324));
#49196=CARTESIAN_POINT('Ctrl Pts',(-0.0464613877374919,0.00280559596990715,
0.00103824715833725));
#49197=CARTESIAN_POINT('',(-0.0464522715406983,0.00280353121836822,-0.00102962802751535));
#49198=CARTESIAN_POINT('Ctrl Pts',(-0.0464522715406983,0.00280353121836822,
-0.00102962802751535));
#49199=CARTESIAN_POINT('Ctrl Pts',(-0.0461764109517263,0.00274067965092877,
-0.000765636240703534));
#49200=CARTESIAN_POINT('Ctrl Pts',(-0.0460077424451037,0.00267543025507494,
-0.000375293469169163));
#49201=CARTESIAN_POINT('Ctrl Pts',(-0.0460104603923367,0.0026764876204308,
1.39454081202657E-5));
#49202=CARTESIAN_POINT('Ctrl Pts',(-0.0460105501879809,0.00267652225571725,
2.02991083324788E-5));
#49203=CARTESIAN_POINT('',(-0.0485379243677292,0.0028057609228668,-0.00103890261335411));
#49204=CARTESIAN_POINT('Ctrl Pts',(-0.0485379243677292,0.0028057609228668,
-0.00103890261335411));
#49205=CARTESIAN_POINT('Ctrl Pts',(-0.0482626321295759,0.00286788646427852,
-0.00129688101678008));
#49206=CARTESIAN_POINT('Ctrl Pts',(-0.0474954951077672,0.00298874310808213,
-0.00158006024895397));
#49207=CARTESIAN_POINT('Ctrl Pts',(-0.0467281321296702,0.00286638278580766,
-0.00129361981432716));
#49208=CARTESIAN_POINT('Ctrl Pts',(-0.0464522715406983,0.00280353121836822,
-0.00102962802751535));
#49209=CARTESIAN_POINT('',(-0.0489894472304209,0.00267652109012544,-1.8656167423741E-5));
#49210=CARTESIAN_POINT('Ctrl Pts',(-0.0489894472304209,0.00267652109012544,
-1.8656167423741E-5));
#49211=CARTESIAN_POINT('Ctrl Pts',(-0.0489840520567291,0.00267855735573614,
-0.000395630752060275));
#49212=CARTESIAN_POINT('Ctrl Pts',(-0.0488168919200026,0.00274251464423592,
-0.000775051359101422));
#49213=CARTESIAN_POINT('Ctrl Pts',(-0.0485409904223183,0.00280506900251836,
-0.0010360293907997));
#49214=CARTESIAN_POINT('Ctrl Pts',(-0.0485379243677292,0.0028057609228668,
-0.00103890261335411));
#49215=CARTESIAN_POINT('',(-0.0485484173841136,0.00280336755518862,0.0010289747883925));
#49216=CARTESIAN_POINT('Ctrl Pts',(-0.0485484173841136,0.00280336755518862,
0.0010289747883925));
#49217=CARTESIAN_POINT('Ctrl Pts',(-0.0488243561640007,0.00274048389401599,
0.000765098689612273));
#49218=CARTESIAN_POINT('Ctrl Pts',(-0.0489924898026455,0.00267538673953036,
0.000376229036000762));
#49219=CARTESIAN_POINT('Ctrl Pts',(-0.0489895325382811,0.00267648889292995,
-1.26954890466987E-5));
#49220=CARTESIAN_POINT('Ctrl Pts',(-0.0489894472304209,0.00267652109012544,
-1.8656167423741E-5));
#49221=CARTESIAN_POINT('Ctrl Pts',(-0.047521969610817,0.00292787381968359,
0.0014375057980809));
#49222=CARTESIAN_POINT('Ctrl Pts',(-0.0479007709531672,0.00292557966528534,
0.00143215706955921));
#49223=CARTESIAN_POINT('Ctrl Pts',(-0.0482777117231938,0.00286505864139897,
0.00128784653432999));
#49224=CARTESIAN_POINT('Ctrl Pts',(-0.0485484173841136,0.00280336755518862,
0.0010289747883925));
#49225=CARTESIAN_POINT('Ctrl Pts',(-0.0675219697530089,0.00292791234232007,
0.0014375007351075));
#49226=CARTESIAN_POINT('Ctrl Pts',(-0.0675217905822521,0.00272283848633946,
0.00149851530284684));
#49227=CARTESIAN_POINT('Ctrl Pts',(-0.0675249292449862,0.00279751942631426,
0.00169899223914141));
#49228=CARTESIAN_POINT('Ctrl Pts',(-0.0671359306861318,0.00292980295225596,
0.00144284563795754));
#49229=CARTESIAN_POINT('Ctrl Pts',(-0.0671283033320531,0.00272468023725727,
0.00150425289890677));
#49230=CARTESIAN_POINT('Ctrl Pts',(-0.0670869890419856,0.00279975471284072,
0.00170530652254623));
#49231=CARTESIAN_POINT('Ctrl Pts',(-0.0663597555989418,0.00281040271795959,
0.00116400921661836));
#49232=CARTESIAN_POINT('Ctrl Pts',(-0.0663911712050714,0.00262787967136621,
0.00125349479954789));
#49233=CARTESIAN_POINT('Ctrl Pts',(-0.0662058670420217,0.0026583834282292,
0.00137542120560276));
#49234=CARTESIAN_POINT('Ctrl Pts',(-0.065844810804675,0.00261243102946704,
2.73686784603625E-5));
#49235=CARTESIAN_POINT('Ctrl Pts',(-0.0658094820998151,0.00243981891809827,
3.02504277462119E-5));
#49236=CARTESIAN_POINT('Ctrl Pts',(-0.0656221070083461,0.00242419343546418,
3.23331464450973E-5));
#49237=CARTESIAN_POINT('Ctrl Pts',(-0.0663246614268507,0.00279922894991229,
-0.00113315917795546));
#49238=CARTESIAN_POINT('Ctrl Pts',(-0.0663534248332843,0.00261785874660285,
-0.00122287857653879));
#49239=CARTESIAN_POINT('Ctrl Pts',(-0.0661660653383145,0.00264516117224189,
-0.00133894667362545));
#49240=CARTESIAN_POINT('Ctrl Pts',(-0.067475667560966,0.00298937709191257,
-0.00158152248003427));
#49241=CARTESIAN_POINT('Ctrl Pts',(-0.0674776982153359,0.00277625525457778,
-0.00163733766341944));
#49242=CARTESIAN_POINT('Ctrl Pts',(-0.0674723735075983,0.00287024649410697,
-0.00186926883315253));
#49243=CARTESIAN_POINT('Ctrl Pts',(-0.0686390883124264,0.00281072577948571,
-0.00116572585728214));
#49244=CARTESIAN_POINT('Ctrl Pts',(-0.068607647449207,0.00262816948297615,
-0.0012553002294259));
#49245=CARTESIAN_POINT('Ctrl Pts',(-0.0687928212048197,0.00265876571215968,
-0.00137744992107544));
#49246=CARTESIAN_POINT('Ctrl Pts',(-0.0691553277660854,0.00261238743571347,
-2.56552014422452E-5));
#49247=CARTESIAN_POINT('Ctrl Pts',(-0.0691906502037132,0.00243978444592516,
-2.85609443699341E-5));
#49248=CARTESIAN_POINT('Ctrl Pts',(-0.0693780503329557,0.00242414178609795,
-3.03066921536361E-5));
#49249=CARTESIAN_POINT('Ctrl Pts',(-0.0686760035727276,0.00279905892909023,
0.00113193946402892));
#49250=CARTESIAN_POINT('Ctrl Pts',(-0.0686472257773982,0.00261770650436945,
0.00122160652879807));
#49251=CARTESIAN_POINT('Ctrl Pts',(-0.0688346894846698,0.00264495997721765,
0.00133750508047802));
#49252=CARTESIAN_POINT('Ctrl Pts',(-0.0679080088854605,0.00292602173206304,
0.00143215583134953));
#49253=CARTESIAN_POINT('Ctrl Pts',(-0.0679147483545036,0.00272099921368871,
0.0014927854273181));
#49254=CARTESIAN_POINT('Ctrl Pts',(-0.0679628751525174,0.00279528411067137,
0.00169267787348788));
#49255=CARTESIAN_POINT('Ctrl Pts',(-0.0675219697530089,0.00292791234232007,
0.0014375007351075));
#49256=CARTESIAN_POINT('Ctrl Pts',(-0.0675217905822521,0.00272283848633946,
0.00149851530284684));
#49257=CARTESIAN_POINT('Ctrl Pts',(-0.0675249292449862,0.00279751942631426,
0.00169899223914141));
#49258=CARTESIAN_POINT('',(-0.0675248989283422,0.00279679729590145,0.00169705696579711));
#49259=CARTESIAN_POINT('',(-0.067521969610817,0.00292787381968359,0.00143750579808091));
#49260=CARTESIAN_POINT('Ctrl Pts',(-0.067524898940367,0.0027968083975309,
0.00169705296016689));
#49261=CARTESIAN_POINT('Ctrl Pts',(-0.0675217930237306,0.00272496362417165,
0.00149792539327892));
#49262=CARTESIAN_POINT('Ctrl Pts',(-0.0675219697209349,0.00292787557066265,
0.00143751167942811));
#49263=CARTESIAN_POINT('',(-0.0675,0.002796875,0.00169723753033423));
#49264=CARTESIAN_POINT('Ctrl Pts',(-0.0675,0.002796875,0.00169723753033423));
#49265=CARTESIAN_POINT('Ctrl Pts',(-0.0670556118872741,0.00279685666170104,
0.00169708273941661));
#49266=CARTESIAN_POINT('Ctrl Pts',(-0.0661665719179776,0.00264539629297987,
0.00133451307288425));
#49267=CARTESIAN_POINT('Ctrl Pts',(-0.0656341151866447,0.00242721165967408,
2.0414311030091E-6));
#49268=CARTESIAN_POINT('Ctrl Pts',(-0.0661678030184114,0.00264575759329887,
-0.00133706644457988));
#49269=CARTESIAN_POINT('Ctrl Pts',(-0.0675004674124815,0.00287245605236691,
-0.00187753708326946));
#49270=CARTESIAN_POINT('Ctrl Pts',(-0.0688323000379284,0.00264566812967151,
-0.00133621021713016));
#49271=CARTESIAN_POINT('Ctrl Pts',(-0.0693659912919883,0.00242720638772113,
8.0357047990023E-8));
#49272=CARTESIAN_POINT('Ctrl Pts',(-0.0688362194957707,0.00264414723702811,
0.00132712816164593));
#49273=CARTESIAN_POINT('Ctrl Pts',(-0.0679609366490351,0.00279406634542389,
0.00169058598422322));
#49274=CARTESIAN_POINT('Ctrl Pts',(-0.0675248989283412,0.00279679729590146,
0.00169705696579713));
#49275=CARTESIAN_POINT('',(-0.0675,0.00292794117647059,0.00143766002569487));
#49276=CARTESIAN_POINT('Ctrl Pts',(-0.0674999999943631,0.00279686254156731,
0.00169724202650596));
#49277=CARTESIAN_POINT('Ctrl Pts',(-0.0674994195756651,0.00272498843318775,
0.00149808548501933));
#49278=CARTESIAN_POINT('Ctrl Pts',(-0.0675000000046904,0.00292793913822137,
0.00143765318065731));
#49279=CARTESIAN_POINT('',(-0.0664613877374912,0.002805595969907,0.00103824715833662));
#49280=CARTESIAN_POINT('Ctrl Pts',(-0.0664613877374912,0.002805595969907,
0.00103824715833662));
#49281=CARTESIAN_POINT('Ctrl Pts',(-0.0667365913194378,0.0028677273296308,
0.00129598001878069));
#49282=CARTESIAN_POINT('Ctrl Pts',(-0.0671182158646944,0.0029279629632896,
0.00143762672627058));
#49283=CARTESIAN_POINT('Ctrl Pts',(-0.0675,0.00292794117647059,0.00143766002569488));
#49284=CARTESIAN_POINT('',(-0.0660105501879809,0.00267652225571724,2.02991083315871E-5));
#49285=CARTESIAN_POINT('Ctrl Pts',(-0.0660105501879809,0.00267652225571724,
2.0299108331587E-5));
#49286=CARTESIAN_POINT('Ctrl Pts',(-0.0660158709169042,0.0026785745264265,
0.000396779691601394));
#49287=CARTESIAN_POINT('Ctrl Pts',(-0.0661825726657909,0.00274235049501098,
0.000774645398475571));
#49288=CARTESIAN_POINT('Ctrl Pts',(-0.0664582351392801,0.00280488422330787,
0.00103529469620283));
#49289=CARTESIAN_POINT('Ctrl Pts',(-0.0664613877374912,0.002805595969907,
0.00103824715833662));
#49290=CARTESIAN_POINT('',(-0.0664522715406983,0.00280353121836822,-0.00102962802751535));
#49291=CARTESIAN_POINT('Ctrl Pts',(-0.0664522715406983,0.00280353121836822,
-0.00102962802751535));
#49292=CARTESIAN_POINT('Ctrl Pts',(-0.0661764109517263,0.00274067965092877,
-0.000765636240703538));
#49293=CARTESIAN_POINT('Ctrl Pts',(-0.0660077424451038,0.00267543025507499,
-0.000375293469169463));
#49294=CARTESIAN_POINT('Ctrl Pts',(-0.0660104603923367,0.0026764876204308,
1.39454081196724E-5));
#49295=CARTESIAN_POINT('Ctrl Pts',(-0.0660105501879809,0.00267652225571724,
2.0299108331587E-5));
#49296=CARTESIAN_POINT('',(-0.0685379243677287,0.00280576092286691,-0.00103890261335452));
#49297=CARTESIAN_POINT('Ctrl Pts',(-0.0685379243677287,0.00280576092286691,
-0.00103890261335452));
#49298=CARTESIAN_POINT('Ctrl Pts',(-0.0682626321295755,0.00286788646427859,
-0.00129688101678024));
#49299=CARTESIAN_POINT('Ctrl Pts',(-0.067495495107767,0.0029887431080821,
-0.0015800602489539));
#49300=CARTESIAN_POINT('Ctrl Pts',(-0.0667281321296702,0.00286638278580766,
-0.00129361981432716));
#49301=CARTESIAN_POINT('Ctrl Pts',(-0.0664522715406983,0.00280353121836822,
-0.00102962802751535));
#49302=CARTESIAN_POINT('',(-0.0689894472304209,0.00267652109012544,-1.86561674233391E-5));
#49303=CARTESIAN_POINT('Ctrl Pts',(-0.0689894472304209,0.00267652109012544,
-1.86561674233391E-5));
#49304=CARTESIAN_POINT('Ctrl Pts',(-0.0689840520567293,0.0026785573557361,
-0.000395630752060009));
#49305=CARTESIAN_POINT('Ctrl Pts',(-0.0688168919200026,0.00274251464423593,
-0.000775051359101532));
#49306=CARTESIAN_POINT('Ctrl Pts',(-0.068540990422318,0.00280506900251843,
-0.00103602939079997));
#49307=CARTESIAN_POINT('Ctrl Pts',(-0.0685379243677287,0.00280576092286691,
-0.00103890261335452));
#49308=CARTESIAN_POINT('',(-0.0685484173841136,0.00280336755518862,0.0010289747883925));
#49309=CARTESIAN_POINT('Ctrl Pts',(-0.0685484173841136,0.00280336755518862,
0.00102897478839251));
#49310=CARTESIAN_POINT('Ctrl Pts',(-0.0688243561640007,0.00274048389401599,
0.00076509868961228));
#49311=CARTESIAN_POINT('Ctrl Pts',(-0.0689924898026455,0.00267538673953038,
0.000376229036000899));
#49312=CARTESIAN_POINT('Ctrl Pts',(-0.0689895325382811,0.00267648889292995,
-1.26954890464299E-5));
#49313=CARTESIAN_POINT('Ctrl Pts',(-0.0689894472304209,0.00267652109012544,
-1.86561674233391E-5));
#49314=CARTESIAN_POINT('Ctrl Pts',(-0.067521969610817,0.00292787381968359,
0.00143750579808091));
#49315=CARTESIAN_POINT('Ctrl Pts',(-0.0679007709531672,0.00292557966528535,
0.00143215706955923));
#49316=CARTESIAN_POINT('Ctrl Pts',(-0.0682777117231937,0.00286505864139897,
0.00128784653433001));
#49317=CARTESIAN_POINT('Ctrl Pts',(-0.0685484173841136,0.00280336755518862,
0.0010289747883925));
#49318=CARTESIAN_POINT('Ctrl Pts',(-0.087521969753009,0.00292791234232007,
0.0014375007351075));
#49319=CARTESIAN_POINT('Ctrl Pts',(-0.0875217905822522,0.00272283848633951,
0.00149851530284683));
#49320=CARTESIAN_POINT('Ctrl Pts',(-0.0875249292449862,0.00279751942631424,
0.00169899223914137));
#49321=CARTESIAN_POINT('Ctrl Pts',(-0.0871359306861318,0.00292980295225596,
0.00144284563795755));
#49322=CARTESIAN_POINT('Ctrl Pts',(-0.087128303332053,0.00272468023725732,
0.00150425289890676));
#49323=CARTESIAN_POINT('Ctrl Pts',(-0.0870869890419856,0.0027997547128407,
0.00170530652254619));
#49324=CARTESIAN_POINT('Ctrl Pts',(-0.0863597555989418,0.00281040271795959,
0.00116400921661838));
#49325=CARTESIAN_POINT('Ctrl Pts',(-0.0863911712050714,0.00262787967136625,
0.00125349479954789));
#49326=CARTESIAN_POINT('Ctrl Pts',(-0.0862058670420218,0.0026583834282292,
0.00137542120560275));
#49327=CARTESIAN_POINT('Ctrl Pts',(-0.0858448108046749,0.00261243102946704,
2.73686784603756E-5));
#49328=CARTESIAN_POINT('Ctrl Pts',(-0.0858094820998151,0.00243981891809831,
3.02504277462256E-5));
#49329=CARTESIAN_POINT('Ctrl Pts',(-0.0856221070083461,0.00242419343546418,
3.23331464451119E-5));
#49330=CARTESIAN_POINT('Ctrl Pts',(-0.0863246614268507,0.00279922894991229,
-0.00113315917795547));
#49331=CARTESIAN_POINT('Ctrl Pts',(-0.0863534248332843,0.00261785874660288,
-0.00122287857653878));
#49332=CARTESIAN_POINT('Ctrl Pts',(-0.0861660653383145,0.00264516117224188,
-0.00133894667362542));
#49333=CARTESIAN_POINT('Ctrl Pts',(-0.0874756675609659,0.00298937709191257,
-0.00158152248003427));
#49334=CARTESIAN_POINT('Ctrl Pts',(-0.0874776982153359,0.00277625525457783,
-0.00163733766341943));
#49335=CARTESIAN_POINT('Ctrl Pts',(-0.0874723735075982,0.00287024649410694,
-0.00186926883315248));
#49336=CARTESIAN_POINT('Ctrl Pts',(-0.0886390883124264,0.00281072577948571,
-0.00116572585728214));
#49337=CARTESIAN_POINT('Ctrl Pts',(-0.088607647449207,0.00262816948297619,
-0.00125530022942588));
#49338=CARTESIAN_POINT('Ctrl Pts',(-0.0887928212048197,0.00265876571215967,
-0.00137744992107541));
#49339=CARTESIAN_POINT('Ctrl Pts',(-0.0891553277660854,0.00261238743571347,
-2.56552014422575E-5));
#49340=CARTESIAN_POINT('Ctrl Pts',(-0.0891906502037131,0.00243978444592521,
-2.85609443699477E-5));
#49341=CARTESIAN_POINT('Ctrl Pts',(-0.0893780503329556,0.00242414178609795,
-3.030669215365E-5));
#49342=CARTESIAN_POINT('Ctrl Pts',(-0.0886760035727276,0.00279905892909023,
0.0011319394640289));
#49343=CARTESIAN_POINT('Ctrl Pts',(-0.0886472257773982,0.0026177065043695,
0.00122160652879803));
#49344=CARTESIAN_POINT('Ctrl Pts',(-0.0888346894846697,0.00264495997721763,
0.00133750508047797));
#49345=CARTESIAN_POINT('Ctrl Pts',(-0.0879080088854605,0.00292602173206304,
0.00143215583134954));
#49346=CARTESIAN_POINT('Ctrl Pts',(-0.0879147483545036,0.00272099921368876,
0.00149278542731808));
#49347=CARTESIAN_POINT('Ctrl Pts',(-0.0879628751525175,0.00279528411067136,
0.00169267787348782));
#49348=CARTESIAN_POINT('Ctrl Pts',(-0.087521969753009,0.00292791234232007,
0.0014375007351075));
#49349=CARTESIAN_POINT('Ctrl Pts',(-0.0875217905822522,0.00272283848633951,
0.00149851530284683));
#49350=CARTESIAN_POINT('Ctrl Pts',(-0.0875249292449862,0.00279751942631424,
0.00169899223914137));
#49351=CARTESIAN_POINT('',(-0.0875248989283422,0.00279679729590145,0.00169705696579711));
#49352=CARTESIAN_POINT('',(-0.087521969610817,0.00292787381968359,0.00143750579808091));
#49353=CARTESIAN_POINT('Ctrl Pts',(-0.087524898940367,0.00279680839753089,
0.00169705296016689));
#49354=CARTESIAN_POINT('Ctrl Pts',(-0.0875217930237306,0.00272496362417165,
0.00149792539327892));
#49355=CARTESIAN_POINT('Ctrl Pts',(-0.087521969720935,0.00292787557066265,
0.00143751167942811));
#49356=CARTESIAN_POINT('',(-0.0875,0.002796875,0.00169723753033423));
#49357=CARTESIAN_POINT('Ctrl Pts',(-0.0875,0.002796875,0.00169723753033423));
#49358=CARTESIAN_POINT('Ctrl Pts',(-0.0870556118872741,0.00279685666170104,
0.00169708273941661));
#49359=CARTESIAN_POINT('Ctrl Pts',(-0.0861665719179776,0.00264539629297987,
0.00133451307288424));
#49360=CARTESIAN_POINT('Ctrl Pts',(-0.0856341151866447,0.00242721165967408,
2.04143110301139E-6));
#49361=CARTESIAN_POINT('Ctrl Pts',(-0.0861678030184114,0.00264575759329887,
-0.00133706644457989));
#49362=CARTESIAN_POINT('Ctrl Pts',(-0.0875004674124815,0.00287245605236691,
-0.00187753708326946));
#49363=CARTESIAN_POINT('Ctrl Pts',(-0.0888323000379284,0.00264566812967151,
-0.00133621021713016));
#49364=CARTESIAN_POINT('Ctrl Pts',(-0.0893659912919883,0.00242720638772113,
8.03570479923811E-8));
#49365=CARTESIAN_POINT('Ctrl Pts',(-0.0888362194957707,0.00264414723702811,
0.00132712816164589));
#49366=CARTESIAN_POINT('Ctrl Pts',(-0.0879609366490351,0.00279406634542388,
0.00169058598422319));
#49367=CARTESIAN_POINT('Ctrl Pts',(-0.0875248989283412,0.00279679729590146,
0.00169705696579712));
#49368=CARTESIAN_POINT('',(-0.0875,0.00292794117647059,0.00143766002569487));
#49369=CARTESIAN_POINT('Ctrl Pts',(-0.0874999999943631,0.00279686254156731,
0.00169724202650596));
#49370=CARTESIAN_POINT('Ctrl Pts',(-0.0874994195756651,0.00272498843318775,
0.00149808548501933));
#49371=CARTESIAN_POINT('Ctrl Pts',(-0.0875000000046905,0.00292793913822137,
0.00143765318065731));
#49372=CARTESIAN_POINT('',(-0.0864613877374919,0.00280559596990716,0.00103824715833728));
#49373=CARTESIAN_POINT('Ctrl Pts',(-0.0864613877374919,0.00280559596990716,
0.00103824715833728));
#49374=CARTESIAN_POINT('Ctrl Pts',(-0.0867365913194384,0.0028677273296309,
0.00129598001878093));
#49375=CARTESIAN_POINT('Ctrl Pts',(-0.0871182158646947,0.0029279629632896,
0.00143762672627057));
#49376=CARTESIAN_POINT('Ctrl Pts',(-0.0875,0.00292794117647059,0.00143766002569487));
#49377=CARTESIAN_POINT('',(-0.0860105501879809,0.00267652225571725,2.02991083332626E-5));
#49378=CARTESIAN_POINT('Ctrl Pts',(-0.0860105501879809,0.00267652225571725,
2.02991083332626E-5));
#49379=CARTESIAN_POINT('Ctrl Pts',(-0.0860158709169047,0.00267857452642669,
0.000396779691602501));
#49380=CARTESIAN_POINT('Ctrl Pts',(-0.0861825726657915,0.00274235049501113,
0.000774645398476271));
#49381=CARTESIAN_POINT('Ctrl Pts',(-0.0864582351392805,0.00280488422330797,
0.00103529469620327));
#49382=CARTESIAN_POINT('Ctrl Pts',(-0.0864613877374919,0.00280559596990716,
0.00103824715833728));
#49383=CARTESIAN_POINT('',(-0.0864522715406982,0.00280353121836822,-0.00102962802751535));
#49384=CARTESIAN_POINT('Ctrl Pts',(-0.0864522715406982,0.00280353121836822,
-0.00102962802751535));
#49385=CARTESIAN_POINT('Ctrl Pts',(-0.0861764109517263,0.00274067965092877,
-0.000765636240703536));
#49386=CARTESIAN_POINT('Ctrl Pts',(-0.0860077424451036,0.00267543025507489,
-0.000375293469168902));
#49387=CARTESIAN_POINT('Ctrl Pts',(-0.0860104603923367,0.00267648762043081,
1.39454081207884E-5));
#49388=CARTESIAN_POINT('Ctrl Pts',(-0.0860105501879809,0.00267652225571725,
2.02991083332626E-5));
#49389=CARTESIAN_POINT('',(-0.0885379243677292,0.00280576092286681,-0.00103890261335415));
#49390=CARTESIAN_POINT('Ctrl Pts',(-0.0885379243677291,0.00280576092286681,
-0.00103890261335415));
#49391=CARTESIAN_POINT('Ctrl Pts',(-0.0882626321295759,0.00286788646427853,
-0.0012968810167801));
#49392=CARTESIAN_POINT('Ctrl Pts',(-0.0874954951077672,0.00298874310808213,
-0.00158006024895397));
#49393=CARTESIAN_POINT('Ctrl Pts',(-0.0867281321296702,0.00286638278580766,
-0.00129361981432716));
#49394=CARTESIAN_POINT('Ctrl Pts',(-0.0864522715406982,0.00280353121836822,
-0.00102962802751535));
#49395=CARTESIAN_POINT('',(-0.0889894472304209,0.00267652109012543,-1.86561674220561E-5));
#49396=CARTESIAN_POINT('Ctrl Pts',(-0.0889894472304209,0.00267652109012543,
-1.86561674220561E-5));
#49397=CARTESIAN_POINT('Ctrl Pts',(-0.0889840520567296,0.00267855735573596,
-0.000395630752059159));
#49398=CARTESIAN_POINT('Ctrl Pts',(-0.088816891920003,0.00274251464423583,
-0.000775051359101059));
#49399=CARTESIAN_POINT('Ctrl Pts',(-0.0885409904223183,0.00280506900251837,
-0.00103602939079972));
#49400=CARTESIAN_POINT('Ctrl Pts',(-0.0885379243677291,0.00280576092286681,
-0.00103890261335415));
#49401=CARTESIAN_POINT('',(-0.0885484173841136,0.00280336755518862,0.0010289747883925));
#49402=CARTESIAN_POINT('Ctrl Pts',(-0.0885484173841136,0.00280336755518862,
0.0010289747883925));
#49403=CARTESIAN_POINT('Ctrl Pts',(-0.0888243561640007,0.00274048389401599,
0.000765098689612275));
#49404=CARTESIAN_POINT('Ctrl Pts',(-0.0889924898026453,0.00267538673953045,
0.000376229036001328));
#49405=CARTESIAN_POINT('Ctrl Pts',(-0.0889895325382811,0.00267648889292995,
-1.26954890455724E-5));
#49406=CARTESIAN_POINT('Ctrl Pts',(-0.0889894472304209,0.00267652109012543,
-1.86561674220561E-5));
#49407=CARTESIAN_POINT('Ctrl Pts',(-0.087521969610817,0.00292787381968359,
0.00143750579808091));
#49408=CARTESIAN_POINT('Ctrl Pts',(-0.0879007709531672,0.00292557966528534,
0.00143215706955922));
#49409=CARTESIAN_POINT('Ctrl Pts',(-0.0882777117231937,0.00286505864139897,
0.00128784653433));
#49410=CARTESIAN_POINT('Ctrl Pts',(-0.0885484173841136,0.00280336755518862,
0.0010289747883925));
#49411=CARTESIAN_POINT('Ctrl Pts',(-0.107521969753009,0.00292791234232008,
0.0014375007351075));
#49412=CARTESIAN_POINT('Ctrl Pts',(-0.107521790582252,0.00272283848633961,
0.00149851530284679));
#49413=CARTESIAN_POINT('Ctrl Pts',(-0.107524929244986,0.00279751942631421,
0.00169899223914127));
#49414=CARTESIAN_POINT('Ctrl Pts',(-0.107135930686132,0.00292980295225595,
0.00144284563795752));
#49415=CARTESIAN_POINT('Ctrl Pts',(-0.107128303332053,0.00272468023725742,
0.00150425289890669));
#49416=CARTESIAN_POINT('Ctrl Pts',(-0.107086989041985,0.00279975471284066,
0.00170530652254606));
#49417=CARTESIAN_POINT('Ctrl Pts',(-0.106359755598941,0.00281040271795956,
0.00116400921661828));
#49418=CARTESIAN_POINT('Ctrl Pts',(-0.106391171205071,0.00262787967136631,
0.00125349479954775));
#49419=CARTESIAN_POINT('Ctrl Pts',(-0.106205867042022,0.00265838342822915,
0.00137542120560257));
#49420=CARTESIAN_POINT('Ctrl Pts',(-0.105844810804675,0.00261243102946704,
2.73686784602542E-5));
#49421=CARTESIAN_POINT('Ctrl Pts',(-0.105809482099816,0.00243981891809839,
3.02504277460862E-5));
#49422=CARTESIAN_POINT('Ctrl Pts',(-0.105622107008346,0.00242419343546419,
3.23331464449678E-5));
#49423=CARTESIAN_POINT('Ctrl Pts',(-0.106324661426851,0.00279922894991231,
-0.00113315917795554));
#49424=CARTESIAN_POINT('Ctrl Pts',(-0.106353424833284,0.002617858746603,
-0.00122287857653881));
#49425=CARTESIAN_POINT('Ctrl Pts',(-0.106166065338315,0.0026451611722419,
-0.00133894667362546));
#49426=CARTESIAN_POINT('Ctrl Pts',(-0.107475667560966,0.00298937709191257,
-0.00158152248003427));
#49427=CARTESIAN_POINT('Ctrl Pts',(-0.107477698215336,0.00277625525457795,
-0.00163733766341938));
#49428=CARTESIAN_POINT('Ctrl Pts',(-0.107472373507598,0.0028702464941069,
-0.00186926883315237));
#49429=CARTESIAN_POINT('Ctrl Pts',(-0.108639088312426,0.00281072577948568,
-0.00116572585728207));
#49430=CARTESIAN_POINT('Ctrl Pts',(-0.108607647449207,0.00262816948297624,
-0.00125530022942576));
#49431=CARTESIAN_POINT('Ctrl Pts',(-0.10879282120482,0.00265876571215962,
-0.00137744992107526));
#49432=CARTESIAN_POINT('Ctrl Pts',(-0.109155327766085,0.00261238743571347,
-2.5655201442127E-5));
#49433=CARTESIAN_POINT('Ctrl Pts',(-0.109190650203713,0.00243978444592529,
-2.85609443698138E-5));
#49434=CARTESIAN_POINT('Ctrl Pts',(-0.109378050332955,0.00242414178609796,
-3.0306692153495E-5));
#49435=CARTESIAN_POINT('Ctrl Pts',(-0.108676003572727,0.00279905892909026,
0.00113193946402899));
#49436=CARTESIAN_POINT('Ctrl Pts',(-0.108647225777398,0.0026177065043696,
0.00122160652879808));
#49437=CARTESIAN_POINT('Ctrl Pts',(-0.108834689484669,0.00264495997721766,
0.00133750508047803));
#49438=CARTESIAN_POINT('Ctrl Pts',(-0.107908008885461,0.00292602173206305,
0.00143215583134956));
#49439=CARTESIAN_POINT('Ctrl Pts',(-0.107914748354504,0.00272099921368888,
0.00149278542731809));
#49440=CARTESIAN_POINT('Ctrl Pts',(-0.107962875152517,0.00279528411067133,
0.00169267787348776));
#49441=CARTESIAN_POINT('Ctrl Pts',(-0.107521969753009,0.00292791234232008,
0.0014375007351075));
#49442=CARTESIAN_POINT('Ctrl Pts',(-0.107521790582252,0.00272283848633961,
0.00149851530284679));
#49443=CARTESIAN_POINT('Ctrl Pts',(-0.107524929244986,0.00279751942631421,
0.00169899223914127));
#49444=CARTESIAN_POINT('',(-0.107524898928342,0.00279679729590145,0.00169705696579711));
#49445=CARTESIAN_POINT('',(-0.107521969610817,0.00292787381968359,0.00143750579808091));
#49446=CARTESIAN_POINT('Ctrl Pts',(-0.107524898940367,0.0027968083975309,
0.00169705296016689));
#49447=CARTESIAN_POINT('Ctrl Pts',(-0.107521793023731,0.00272496362417165,
0.00149792539327893));
#49448=CARTESIAN_POINT('Ctrl Pts',(-0.107521969720935,0.00292787557066265,
0.00143751167942811));
#49449=CARTESIAN_POINT('',(-0.1075,0.002796875,0.00169723753033423));
#49450=CARTESIAN_POINT('Ctrl Pts',(-0.1075,0.002796875,0.00169723753033422));
#49451=CARTESIAN_POINT('Ctrl Pts',(-0.107055611887274,0.00279685666170103,
0.00169708273941661));
#49452=CARTESIAN_POINT('Ctrl Pts',(-0.106166571917978,0.00264539629297986,
0.00133451307288423));
#49453=CARTESIAN_POINT('Ctrl Pts',(-0.105634115186645,0.00242721165967408,
2.04143110301389E-6));
#49454=CARTESIAN_POINT('Ctrl Pts',(-0.106167803018411,0.00264575759329888,
-0.00133706644457991));
#49455=CARTESIAN_POINT('Ctrl Pts',(-0.107500467412482,0.00287245605236691,
-0.00187753708326945));
#49456=CARTESIAN_POINT('Ctrl Pts',(-0.108832300037928,0.00264566812967151,
-0.00133621021713017));
#49457=CARTESIAN_POINT('Ctrl Pts',(-0.109365991291988,0.00242720638772112,
8.03570480027352E-8));
#49458=CARTESIAN_POINT('Ctrl Pts',(-0.108836219495771,0.00264414723702813,
0.00132712816164603));
#49459=CARTESIAN_POINT('Ctrl Pts',(-0.107960936649035,0.00279406634542393,
0.00169058598422331));
#49460=CARTESIAN_POINT('Ctrl Pts',(-0.107524898928341,0.00279679729590146,
0.00169705696579713));
#49461=CARTESIAN_POINT('',(-0.1075,0.00292794117647059,0.00143766002569487));
#49462=CARTESIAN_POINT('Ctrl Pts',(-0.107499999994363,0.00279686254156731,
0.00169724202650596));
#49463=CARTESIAN_POINT('Ctrl Pts',(-0.107499419575665,0.00272498843318775,
0.00149808548501934));
#49464=CARTESIAN_POINT('Ctrl Pts',(-0.10750000000469,0.00292793913822137,
0.00143765318065731));
#49465=CARTESIAN_POINT('',(-0.106461387737498,0.0028055959699086,0.00103824715834326));
#49466=CARTESIAN_POINT('Ctrl Pts',(-0.106461387737498,0.0028055959699086,
0.00103824715834326));
#49467=CARTESIAN_POINT('Ctrl Pts',(-0.106736591319444,0.00286772732963183,
0.00129598001878312));
#49468=CARTESIAN_POINT('Ctrl Pts',(-0.107118215864697,0.0029279629632896,
0.00143762672627057));
#49469=CARTESIAN_POINT('Ctrl Pts',(-0.1075,0.00292794117647059,0.00143766002569487));
#49470=CARTESIAN_POINT('',(-0.106010550187981,0.00267652225571722,2.02991083284823E-5));
#49471=CARTESIAN_POINT('Ctrl Pts',(-0.106010550187981,0.00267652225571722,
2.02991083284823E-5));
#49472=CARTESIAN_POINT('Ctrl Pts',(-0.106015870916903,0.00267857452642615,
0.000396779691599338));
#49473=CARTESIAN_POINT('Ctrl Pts',(-0.106182572665792,0.00274235049501136,
0.000774645398478084));
#49474=CARTESIAN_POINT('Ctrl Pts',(-0.106458235139285,0.00280488422330894,
0.00103529469620727));
#49475=CARTESIAN_POINT('Ctrl Pts',(-0.106461387737498,0.0028055959699086,
0.00103824715834326));
#49476=CARTESIAN_POINT('',(-0.106452271540698,0.00280353121836822,-0.00102962802751534));
#49477=CARTESIAN_POINT('Ctrl Pts',(-0.106452271540698,0.00280353121836822,
-0.00102962802751534));
#49478=CARTESIAN_POINT('Ctrl Pts',(-0.106176410951726,0.00274067965092877,
-0.000765636240703531));
#49479=CARTESIAN_POINT('Ctrl Pts',(-0.106007742445104,0.00267543025507516,
-0.000375293469170498));
#49480=CARTESIAN_POINT('Ctrl Pts',(-0.106010460392337,0.0026764876204308,
1.39454081176005E-5));
#49481=CARTESIAN_POINT('Ctrl Pts',(-0.106010550187981,0.00267652225571722,
2.02991083284823E-5));
#49482=CARTESIAN_POINT('',(-0.108537924367725,0.00280576092286767,-0.0010389026133577));
#49483=CARTESIAN_POINT('Ctrl Pts',(-0.108537924367725,0.00280576092286767,
-0.0010389026133577));
#49484=CARTESIAN_POINT('Ctrl Pts',(-0.108262632129572,0.00286788646427908,
-0.0012968810167814));
#49485=CARTESIAN_POINT('Ctrl Pts',(-0.107495495107766,0.00298874310808185,
-0.00158006024895331));
#49486=CARTESIAN_POINT('Ctrl Pts',(-0.10672813212967,0.00286638278580766,
-0.00129361981432716));
#49487=CARTESIAN_POINT('Ctrl Pts',(-0.106452271540698,0.00280353121836822,
-0.00102962802751534));
#49488=CARTESIAN_POINT('',(-0.108989447230421,0.00267652109012545,-1.86561674248701E-5));
#49489=CARTESIAN_POINT('Ctrl Pts',(-0.108989447230421,0.00267652109012544,
-1.86561674248702E-5));
#49490=CARTESIAN_POINT('Ctrl Pts',(-0.108984052056729,0.00267855735573627,
-0.000395630752061024));
#49491=CARTESIAN_POINT('Ctrl Pts',(-0.108816891920001,0.00274251464423628,
-0.000775051359103429));
#49492=CARTESIAN_POINT('Ctrl Pts',(-0.108540990422316,0.00280506900251894,
-0.0010360293908021));
#49493=CARTESIAN_POINT('Ctrl Pts',(-0.108537924367725,0.00280576092286767,
-0.0010389026133577));
#49494=CARTESIAN_POINT('',(-0.108548417384113,0.00280336755518862,0.0010289747883925));
#49495=CARTESIAN_POINT('Ctrl Pts',(-0.108548417384113,0.00280336755518862,
0.0010289747883925));
#49496=CARTESIAN_POINT('Ctrl Pts',(-0.108824356164,0.00274048389401599,
0.000765098689612275));
#49497=CARTESIAN_POINT('Ctrl Pts',(-0.108992489802645,0.00267538673953029,
0.000376229036000389));
#49498=CARTESIAN_POINT('Ctrl Pts',(-0.108989532538281,0.00267648889292995,
-1.26954890474506E-5));
#49499=CARTESIAN_POINT('Ctrl Pts',(-0.108989447230421,0.00267652109012544,
-1.86561674248702E-5));
#49500=CARTESIAN_POINT('Ctrl Pts',(-0.107521969610817,0.00292787381968359,
0.0014375057980809));
#49501=CARTESIAN_POINT('Ctrl Pts',(-0.107900770953167,0.00292557966528534,
0.00143215706955921));
#49502=CARTESIAN_POINT('Ctrl Pts',(-0.108277711723193,0.00286505864139896,
0.00128784653432998));
#49503=CARTESIAN_POINT('Ctrl Pts',(-0.108548417384113,0.00280336755518862,
0.0010289747883925));
#49504=CARTESIAN_POINT('Ctrl Pts',(-0.127521969753009,0.00292791234232007,
0.0014375007351075));
#49505=CARTESIAN_POINT('Ctrl Pts',(-0.127521790582252,0.0027228384863398,
0.00149851530284674));
#49506=CARTESIAN_POINT('Ctrl Pts',(-0.127524929244986,0.00279751942631414,
0.0016989922391411));
#49507=CARTESIAN_POINT('Ctrl Pts',(-0.127135930686132,0.00292980295225595,
0.00144284563795753));
#49508=CARTESIAN_POINT('Ctrl Pts',(-0.127128303332053,0.00272468023725761,
0.00150425289890664));
#49509=CARTESIAN_POINT('Ctrl Pts',(-0.127086989041986,0.00279975471284059,
0.00170530652254589));
#49510=CARTESIAN_POINT('Ctrl Pts',(-0.126359755598941,0.00281040271795957,
0.00116400921661829));
#49511=CARTESIAN_POINT('Ctrl Pts',(-0.126391171205071,0.00262787967136648,
0.00125349479954768));
#49512=CARTESIAN_POINT('Ctrl Pts',(-0.126205867042022,0.00265838342822912,
0.00137542120560247));
#49513=CARTESIAN_POINT('Ctrl Pts',(-0.125844810804675,0.00261243102946704,
2.73686784602689E-5));
#49514=CARTESIAN_POINT('Ctrl Pts',(-0.125809482099816,0.00243981891809853,
3.02504277461029E-5));
#49515=CARTESIAN_POINT('Ctrl Pts',(-0.125622107008347,0.00242419343546421,
3.23331464449823E-5));
#49516=CARTESIAN_POINT('Ctrl Pts',(-0.126324661426851,0.00279922894991231,
-0.00113315917795553));
#49517=CARTESIAN_POINT('Ctrl Pts',(-0.126353424833284,0.00261785874660316,
-0.00122287857653872));
#49518=CARTESIAN_POINT('Ctrl Pts',(-0.126166065338315,0.00264516117224187,
-0.00133894667362534));
#49519=CARTESIAN_POINT('Ctrl Pts',(-0.127475667560966,0.00298937709191257,
-0.00158152248003426));
#49520=CARTESIAN_POINT('Ctrl Pts',(-0.127477698215336,0.00277625525457815,
-0.00163733766341933));
#49521=CARTESIAN_POINT('Ctrl Pts',(-0.127472373507598,0.00287024649410682,
-0.00186926883315216));
#49522=CARTESIAN_POINT('Ctrl Pts',(-0.128639088312426,0.00281072577948569,
-0.0011657258572821));
#49523=CARTESIAN_POINT('Ctrl Pts',(-0.128607647449207,0.00262816948297644,
-0.00125530022942571));
#49524=CARTESIAN_POINT('Ctrl Pts',(-0.12879282120482,0.00265876571215961,
-0.00137744992107518));
#49525=CARTESIAN_POINT('Ctrl Pts',(-0.129155327766085,0.00261238743571346,
-2.56552014421315E-5));
#49526=CARTESIAN_POINT('Ctrl Pts',(-0.129190650203713,0.00243978444592542,
-2.85609443698061E-5));
#49527=CARTESIAN_POINT('Ctrl Pts',(-0.129378050332955,0.00242414178609797,
-3.03066921534991E-5));
#49528=CARTESIAN_POINT('Ctrl Pts',(-0.128676003572727,0.00279905892909026,
0.00113193946402897));
#49529=CARTESIAN_POINT('Ctrl Pts',(-0.128647225777398,0.00261770650436977,
0.00122160652879797));
#49530=CARTESIAN_POINT('Ctrl Pts',(-0.12883468948467,0.00264495997721762,
0.00133750508047789));
#49531=CARTESIAN_POINT('Ctrl Pts',(-0.127908008885461,0.00292602173206305,
0.00143215583134956));
#49532=CARTESIAN_POINT('Ctrl Pts',(-0.127914748354504,0.00272099921368907,
0.00149278542731802));
#49533=CARTESIAN_POINT('Ctrl Pts',(-0.127962875152517,0.00279528411067127,
0.00169267787348758));
#49534=CARTESIAN_POINT('Ctrl Pts',(-0.127521969753009,0.00292791234232007,
0.0014375007351075));
#49535=CARTESIAN_POINT('Ctrl Pts',(-0.127521790582252,0.0027228384863398,
0.00149851530284674));
#49536=CARTESIAN_POINT('Ctrl Pts',(-0.127524929244986,0.00279751942631414,
0.0016989922391411));
#49537=CARTESIAN_POINT('',(-0.127524898928342,0.00279679729590145,0.00169705696579711));
#49538=CARTESIAN_POINT('',(-0.127521969610817,0.00292787381968359,0.0014375057980809));
#49539=CARTESIAN_POINT('Ctrl Pts',(-0.127524898940367,0.0027968083975309,
0.00169705296016689));
#49540=CARTESIAN_POINT('Ctrl Pts',(-0.127521793023731,0.00272496362417165,
0.00149792539327892));
#49541=CARTESIAN_POINT('Ctrl Pts',(-0.127521969720935,0.00292787557066265,
0.00143751167942811));
#49542=CARTESIAN_POINT('',(-0.1275,0.002796875,0.00169723753033423));
#49543=CARTESIAN_POINT('Ctrl Pts',(-0.1275,0.002796875,0.00169723753033422));
#49544=CARTESIAN_POINT('Ctrl Pts',(-0.127055611887274,0.00279685666170104,
0.00169708273941661));
#49545=CARTESIAN_POINT('Ctrl Pts',(-0.126166571917978,0.00264539629297987,
0.00133451307288423));
#49546=CARTESIAN_POINT('Ctrl Pts',(-0.125634115186645,0.00242721165967408,
2.04143110301003E-6));
#49547=CARTESIAN_POINT('Ctrl Pts',(-0.126167803018411,0.00264575759329888,
-0.0013370664445799));
#49548=CARTESIAN_POINT('Ctrl Pts',(-0.127500467412481,0.00287245605236691,
-0.00187753708326946));
#49549=CARTESIAN_POINT('Ctrl Pts',(-0.128832300037928,0.00264566812967151,
-0.00133621021713016));
#49550=CARTESIAN_POINT('Ctrl Pts',(-0.129365991291988,0.00242720638772113,
8.03570479970567E-8));
#49551=CARTESIAN_POINT('Ctrl Pts',(-0.128836219495771,0.00264414723702813,
0.00132712816164604));
#49552=CARTESIAN_POINT('Ctrl Pts',(-0.127960936649035,0.00279406634542393,
0.00169058598422331));
#49553=CARTESIAN_POINT('Ctrl Pts',(-0.127524898928341,0.00279679729590146,
0.00169705696579713));
#49554=CARTESIAN_POINT('',(-0.1275,0.00292794117647059,0.00143766002569487));
#49555=CARTESIAN_POINT('Ctrl Pts',(-0.127499999994363,0.00279686254156731,
0.00169724202650597));
#49556=CARTESIAN_POINT('Ctrl Pts',(-0.127499419575665,0.00272498843318775,
0.00149808548501933));
#49557=CARTESIAN_POINT('Ctrl Pts',(-0.12750000000469,0.00292793913822137,
0.00143765318065731));
#49558=CARTESIAN_POINT('',(-0.126461387737499,0.0028055959699088,0.00103824715834409));
#49559=CARTESIAN_POINT('Ctrl Pts',(-0.126461387737499,0.0028055959699088,
0.00103824715834409));
#49560=CARTESIAN_POINT('Ctrl Pts',(-0.126736591319445,0.00286772732963196,
0.00129598001878342));
#49561=CARTESIAN_POINT('Ctrl Pts',(-0.127118215864698,0.0029279629632896,
0.00143762672627057));
#49562=CARTESIAN_POINT('Ctrl Pts',(-0.1275,0.00292794117647059,0.00143766002569487));
#49563=CARTESIAN_POINT('',(-0.126010550187981,0.00267652225571722,2.02991083269042E-5));
#49564=CARTESIAN_POINT('Ctrl Pts',(-0.126010550187981,0.00267652225571722,
2.02991083269042E-5));
#49565=CARTESIAN_POINT('Ctrl Pts',(-0.126015870916903,0.00267857452642598,
0.000396779691598294));
#49566=CARTESIAN_POINT('Ctrl Pts',(-0.126182572665792,0.00274235049501134,
0.000774645398478129));
#49567=CARTESIAN_POINT('Ctrl Pts',(-0.126458235139285,0.00280488422330907,
0.00103529469620783));
#49568=CARTESIAN_POINT('Ctrl Pts',(-0.126461387737499,0.0028055959699088,
0.00103824715834409));
#49569=CARTESIAN_POINT('',(-0.126452271540698,0.00280353121836822,-0.00102962802751534));
#49570=CARTESIAN_POINT('Ctrl Pts',(-0.126452271540698,0.00280353121836822,
-0.00102962802751534));
#49571=CARTESIAN_POINT('Ctrl Pts',(-0.126176410951726,0.00274067965092877,
-0.000765636240703523));
#49572=CARTESIAN_POINT('Ctrl Pts',(-0.126007742445104,0.00267543025507525,
-0.000375293469171025));
#49573=CARTESIAN_POINT('Ctrl Pts',(-0.126010460392337,0.00267648762043079,
1.39454081165485E-5));
#49574=CARTESIAN_POINT('Ctrl Pts',(-0.126010550187981,0.00267652225571722,
2.02991083269042E-5));
#49575=CARTESIAN_POINT('',(-0.128537924367724,0.00280576092286786,-0.00103890261335849));
#49576=CARTESIAN_POINT('Ctrl Pts',(-0.128537924367724,0.00280576092286786,
-0.00103890261335849));
#49577=CARTESIAN_POINT('Ctrl Pts',(-0.128262632129572,0.0028678864642792,
-0.00129688101678168));
#49578=CARTESIAN_POINT('Ctrl Pts',(-0.127495495107765,0.00298874310808179,
-0.00158006024895316));
#49579=CARTESIAN_POINT('Ctrl Pts',(-0.12672813212967,0.00286638278580766,
-0.00129361981432715));
#49580=CARTESIAN_POINT('Ctrl Pts',(-0.126452271540698,0.00280353121836822,
-0.00102962802751534));
#49581=CARTESIAN_POINT('',(-0.128989447230421,0.00267652109012544,-1.86561674238163E-5));
#49582=CARTESIAN_POINT('Ctrl Pts',(-0.128989447230421,0.00267652109012544,
-1.86561674238163E-5));
#49583=CARTESIAN_POINT('Ctrl Pts',(-0.128984052056729,0.00267855735573615,
-0.000395630752060325));
#49584=CARTESIAN_POINT('Ctrl Pts',(-0.128816891920002,0.00274251464423628,
-0.000775051359103574));
#49585=CARTESIAN_POINT('Ctrl Pts',(-0.128540990422315,0.00280506900251906,
-0.00103602939080263));
#49586=CARTESIAN_POINT('Ctrl Pts',(-0.128537924367724,0.00280576092286786,
-0.00103890261335849));
#49587=CARTESIAN_POINT('',(-0.128548417384113,0.00280336755518862,0.0010289747883925));
#49588=CARTESIAN_POINT('Ctrl Pts',(-0.128548417384113,0.00280336755518862,
0.0010289747883925));
#49589=CARTESIAN_POINT('Ctrl Pts',(-0.128824356164,0.00274048389401599,
0.00076509868961228));
#49590=CARTESIAN_POINT('Ctrl Pts',(-0.128992489802645,0.00267538673953035,
0.00037622903600074));
#49591=CARTESIAN_POINT('Ctrl Pts',(-0.128989532538281,0.00267648889292995,
-1.26954890467481E-5));
#49592=CARTESIAN_POINT('Ctrl Pts',(-0.128989447230421,0.00267652109012544,
-1.86561674238163E-5));
#49593=CARTESIAN_POINT('Ctrl Pts',(-0.127521969610817,0.00292787381968359,
0.0014375057980809));
#49594=CARTESIAN_POINT('Ctrl Pts',(-0.127900770953167,0.00292557966528534,
0.00143215706955922));
#49595=CARTESIAN_POINT('Ctrl Pts',(-0.128277711723193,0.00286505864139897,
0.00128784653432999));
#49596=CARTESIAN_POINT('Ctrl Pts',(-0.128548417384113,0.00280336755518862,
0.0010289747883925));
#49597=CARTESIAN_POINT('Origin',(0.0125,0.013,-4.59242549680257E-18));
#49598=CARTESIAN_POINT('',(0.00634842519685039,0.0128,-0.0108815498639327));
#49599=CARTESIAN_POINT('',(0.00595472440944882,0.0132,-0.0106493834302149));
#49600=CARTESIAN_POINT('Ctrl Pts',(0.00634842519685039,0.0128,-0.0108815498639327));
#49601=CARTESIAN_POINT('Ctrl Pts',(0.00634842519685039,0.0130276434464512,
-0.0108815498639327));
#49602=CARTESIAN_POINT('Ctrl Pts',(0.00614779345682715,0.0132,-0.0107680466496751));
#49603=CARTESIAN_POINT('Ctrl Pts',(0.00595472440944882,0.0132,-0.0106493834302149));
#49604=CARTESIAN_POINT('',(0.00634842519685039,0.0012,-0.0108815498639328));
#49605=CARTESIAN_POINT('',(0.00634842519685039,0.013,-0.0108815498639327));
#49606=CARTESIAN_POINT('',(0.0063484251968504,0.0012,0.0108815498639327));
#49607=CARTESIAN_POINT('Origin',(0.0125,0.0012,-4.59242549680257E-18));
#49608=CARTESIAN_POINT('',(0.0063484251968504,0.0132,0.0108815498639327));
#49609=CARTESIAN_POINT('',(0.0063484251968504,0.013,0.0108815498639327));
#49610=CARTESIAN_POINT('',(0.0125,0.0132,-0.0125));
#49611=CARTESIAN_POINT('Origin',(0.0125,0.0132,-4.59242549680257E-18));
#49612=CARTESIAN_POINT('Origin',(0.0125,0.0132,-4.59242549680257E-18));
#49613=CARTESIAN_POINT('Origin',(-0.00501982557395217,0.0101715728752538,
-2.16840434497101E-19));
#49614=CARTESIAN_POINT('',(-0.00501982557395217,0.013,-0.001));
#49615=CARTESIAN_POINT('Origin',(-0.00501982557395217,0.013,-2.16840434497101E-19));
#49616=CARTESIAN_POINT('',(-0.00501982557395217,0.0132,-0.001));
#49617=CARTESIAN_POINT('',(-0.00501982557395217,0.0101715728752538,-0.001));
#49618=CARTESIAN_POINT('Origin',(-0.00501982557395217,0.0132,-2.16840434497101E-19));
#49619=CARTESIAN_POINT('Origin',(0.00396253460616978,-0.0267643850402721,
0.));
#49620=CARTESIAN_POINT('',(-0.00847413551306003,0.0128,0.00451935750764788));
#49621=CARTESIAN_POINT('',(-0.000426041560703258,0.0128,0.0124834192096569));
#49622=CARTESIAN_POINT('Origin',(0.00396253460616978,0.0128,0.));
#49623=CARTESIAN_POINT('',(-0.000426041560703258,0.0012,0.0124834192096569));
#49624=CARTESIAN_POINT('',(-0.000426041560703259,-0.0267643850402721,0.0124834192096569));
#49625=CARTESIAN_POINT('',(-0.00847413551306003,0.0012,0.00451935750764788));
#49626=CARTESIAN_POINT('Origin',(0.00396253460616978,0.0012,0.));
#49627=CARTESIAN_POINT('',(-0.00847413551306003,-0.0267643850402721,0.00451935750764788));
#49628=CARTESIAN_POINT('Origin',(0.00396253460616978,-0.0267643850402721,
0.));
#49629=CARTESIAN_POINT('',(-0.00918425288415922,0.001,-0.00150244288430738));
#49630=CARTESIAN_POINT('',(-0.00918425288415922,0.0128,-0.00150244288430738));
#49631=CARTESIAN_POINT('',(-0.00918425288415922,0.007,-0.00150244288430738));
#49632=CARTESIAN_POINT('',(-0.00918425288415922,0.0128,0.00150244288430738));
#49633=CARTESIAN_POINT('Origin',(0.00396253460616978,0.0128,0.));
#49634=CARTESIAN_POINT('',(-0.00918425288415922,0.001,0.00150244288430738));
#49635=CARTESIAN_POINT('',(-0.00918425288415922,0.007,0.00150244288430738));
#49636=CARTESIAN_POINT('Origin',(0.00396253460616978,0.001,0.));
#49637=CARTESIAN_POINT('Origin',(0.00625,0.013,-2.29621274840129E-18));
#49638=CARTESIAN_POINT('',(-0.000359710594690624,0.013,-0.0122947390492059));
#49639=CARTESIAN_POINT('',(0.00585,0.013,-0.0108197735650983));
#49640=CARTESIAN_POINT('Origin',(0.,0.013,0.));
#49641=CARTESIAN_POINT('',(0.0060484,0.013,0.0109392347739684));
#49642=CARTESIAN_POINT('Origin',(0.0125,0.013,-4.59242549680257E-18));
#49643=CARTESIAN_POINT('',(0.000266151447280837,0.013,0.0124971662150709));
#49644=CARTESIAN_POINT('Origin',(0.,0.013,0.));
#49645=CARTESIAN_POINT('',(-0.00828616193994173,0.013,0.00445104985208033));
#49646=CARTESIAN_POINT('Origin',(0.00396253460616978,0.013,0.));
#49647=CARTESIAN_POINT('',(-0.00880510120094866,0.013,0.00421409688951767));
#49648=CARTESIAN_POINT('Origin',(-0.00866210908617835,0.013,0.00458766516321543));
#49649=CARTESIAN_POINT('',(-0.00895326315945259,0.013,0.00173913195070769));
#49650=CARTESIAN_POINT('Origin',(-0.00926982557395217,0.013,0.003));
#49651=CARTESIAN_POINT('',(-0.00895326315945259,0.013,-0.00173913195070769));
#49652=CARTESIAN_POINT('Origin',(0.00396253460616978,0.013,0.));
#49653=CARTESIAN_POINT('',(-0.00880510120094866,0.013,-0.00421409688951767));
#49654=CARTESIAN_POINT('Origin',(-0.00926982557395217,0.013,-0.003));
#49655=CARTESIAN_POINT('',(-0.00828616193994173,0.013,-0.00445104985208033));
#49656=CARTESIAN_POINT('Origin',(-0.00866210908617835,0.013,-0.00458766516321543));
#49657=CARTESIAN_POINT('Origin',(0.00396253460616978,0.013,0.));
#49658=CARTESIAN_POINT('',(0.,0.013,0.0115));
#49659=CARTESIAN_POINT('Origin',(0.,0.013,0.011));
#49660=CARTESIAN_POINT('',(0.,0.013,-0.0105));
#49661=CARTESIAN_POINT('Origin',(0.,0.013,-0.011));
#49662=CARTESIAN_POINT('',(-0.00926982557395217,0.013,-0.0025));
#49663=CARTESIAN_POINT('Origin',(-0.00926982557395217,0.013,-0.003));
#49664=CARTESIAN_POINT('',(-0.00926982557395217,0.013,0.0035));
#49665=CARTESIAN_POINT('Origin',(-0.00926982557395217,0.013,0.003));
#49666=CARTESIAN_POINT('Origin',(0.,0.013,0.));
#49667=CARTESIAN_POINT('',(0.00615157480314961,0.0130279409847639,0.0108815498639327));
#49668=CARTESIAN_POINT('Ctrl Pts',(0.00604840000000001,0.013,0.0109392347739684));
#49669=CARTESIAN_POINT('Ctrl Pts',(0.00605844545062544,0.013,0.0109336805551571));
#49670=CARTESIAN_POINT('Ctrl Pts',(0.00606848366139432,0.0130007331928852,
0.0109281121725045));
#49671=CARTESIAN_POINT('Ctrl Pts',(0.0061039365412421,0.0130059660120152,
0.0109083825874413));
#49672=CARTESIAN_POINT('Ctrl Pts',(0.00612881666876444,0.0130145598482818,
0.0108944155280892));
#49673=CARTESIAN_POINT('Ctrl Pts',(0.00615157480314961,0.013027940984764,
0.0108815498639328));
#49674=CARTESIAN_POINT('',(0.00615157480314961,0.0012,0.0108815498639327));
#49675=CARTESIAN_POINT('',(0.00615157480314961,0.013,0.0108815498639327));
#49676=CARTESIAN_POINT('',(-0.000365559547449821,0.0012,0.0124946535052905));
#49677=CARTESIAN_POINT('Origin',(0.,0.0012,0.));
#49678=CARTESIAN_POINT('',(-0.000365559547449821,0.0128603449921863,0.0124946535052905));
#49679=CARTESIAN_POINT('',(-0.000365559547449821,0.013,0.0124946535052905));
#49680=CARTESIAN_POINT('Ctrl Pts',(-0.000365559547449479,0.0128603449921859,
0.0124946535052905));
#49681=CARTESIAN_POINT('Ctrl Pts',(-0.000355817464249198,0.0128695697559461,
0.0124949385321241));
#49682=CARTESIAN_POINT('Ctrl Pts',(-0.00034473067538757,0.0128777448000062,
0.0124952504075834));
#49683=CARTESIAN_POINT('Ctrl Pts',(-0.000293723387019724,0.012910410477147,
0.0124966125421717));
#49684=CARTESIAN_POINT('Ctrl Pts',(-0.000243928646755985,0.0129282527769246,
0.012497667010507));
#49685=CARTESIAN_POINT('Ctrl Pts',(-0.000103079663471278,0.0129721021830651,
0.012500028589373));
#49686=CARTESIAN_POINT('Ctrl Pts',(3.8406604879568E-5,0.0129933569155071,
0.0125008701719831));
#49687=CARTESIAN_POINT('Ctrl Pts',(0.000215988889848001,0.0129995665030976,
0.0124981591951788));
#49688=CARTESIAN_POINT('Ctrl Pts',(0.000241141730008187,0.013,0.0124976988456156));
#49689=CARTESIAN_POINT('Ctrl Pts',(0.000266151447280838,0.013,0.0124971662150709));
#49690=CARTESIAN_POINT('Origin',(0.,0.013,0.));
#49691=CARTESIAN_POINT('',(-0.000365559547449821,0.0012,-0.0124946535052905));
#49692=CARTESIAN_POINT('',(0.0061515748031496,0.0012,-0.0108815498639327));
#49693=CARTESIAN_POINT('Origin',(0.,0.0012,0.));
#49694=CARTESIAN_POINT('',(0.0061515748031496,0.0128,-0.0108815498639327));
#49695=CARTESIAN_POINT('',(0.0061515748031496,0.013,-0.0108815498639328));
#49696=CARTESIAN_POINT('',(-0.00036555954744982,0.0128,-0.0124946535052905));
#49697=CARTESIAN_POINT('Origin',(0.,0.0128,0.));
#49698=CARTESIAN_POINT('',(-0.00036555954744982,0.013,-0.0124946535052905));
#49699=CARTESIAN_POINT('Origin',(-0.14,0.0075,0.));
#49700=CARTESIAN_POINT('',(-0.0399999969037804,0.00997686116634681,-0.00434340405242746));
#49701=CARTESIAN_POINT('',(-0.0399999963113939,0.00997613772986841,0.00434381651807744));
#49702=CARTESIAN_POINT('Ctrl Pts',(-0.04,0.00997615395078692,0.0043438072715076));
#49703=CARTESIAN_POINT('Ctrl Pts',(-0.04,0.0107382262196358,0.00390939383155763));
#49704=CARTESIAN_POINT('Ctrl Pts',(-0.04,0.0113831176353465,0.00327045662389616));
#49705=CARTESIAN_POINT('Ctrl Pts',(-0.04,0.0118237356861523,0.00251236616753416));
#49706=CARTESIAN_POINT('Ctrl Pts',(-0.04,0.0122643368146118,0.00175430482634162));
#49707=CARTESIAN_POINT('Ctrl Pts',(-0.04,0.012500474596807,0.000877315234985374));
#49708=CARTESIAN_POINT('Ctrl Pts',(-0.04,0.0125005474735341,4.15581768158591E-7));
#49709=CARTESIAN_POINT('Ctrl Pts',(-0.04,0.0125006203502613,-0.000876484072272305));
#49710=CARTESIAN_POINT('Ctrl Pts',(-0.04,0.0122646283392576,-0.00175351290185706));
#49711=CARTESIAN_POINT('Ctrl Pts',(-0.04,0.0118241532168882,-0.00251164746737131));
#49712=CARTESIAN_POINT('Ctrl Pts',(-0.04,0.0113836611778392,-0.00326981114944385));
#49713=CARTESIAN_POINT('Ctrl Pts',(-0.04,0.0107388759723705,-0.00390885553816552));
#49714=CARTESIAN_POINT('Ctrl Pts',(-0.04,0.00997687591821936,-0.00434339564002003));
#49715=CARTESIAN_POINT('',(-0.04,0.0075,-0.005));
#49716=CARTESIAN_POINT('Origin',(-0.04,0.00750000000000001,7.7715611723761E-18));
#49717=CARTESIAN_POINT('',(-0.0399999990786921,0.00503252942117453,-0.00434874567463202));
#49718=CARTESIAN_POINT('Origin',(-0.04,0.00750000000000002,-4.9960036108132E-18));
#49719=CARTESIAN_POINT('',(-0.0399999989166323,0.00503323066735753,0.00434914348573771));
#49720=CARTESIAN_POINT('Ctrl Pts',(-0.04,0.00503252942117453,-0.00434874567463202));
#49721=CARTESIAN_POINT('Ctrl Pts',(-0.04,0.00426802397510403,-0.00391496664116614));
#49722=CARTESIAN_POINT('Ctrl Pts',(-0.04,0.00362078375203728,-0.00327557207983672));
#49723=CARTESIAN_POINT('Ctrl Pts',(-0.04,0.00317856541491556,-0.00251633280931734));
#49724=CARTESIAN_POINT('Ctrl Pts',(-0.04,0.00273636410682584,-0.00175712277573535));
#49725=CARTESIAN_POINT('Ctrl Pts',(-0.04,0.00249937673440971,-0.000878295009110667));
#49726=CARTESIAN_POINT('Ctrl Pts',(-0.04,0.00249944757726906,4.03157137211354E-7));
#49727=CARTESIAN_POINT('Ctrl Pts',(-0.04,0.00249951842012842,0.000879101323554153));
#49728=CARTESIAN_POINT('Ctrl Pts',(-0.04,0.00273664749617628,0.00175789086588404));
#49729=CARTESIAN_POINT('Ctrl Pts',(-0.04,0.00317897121753076,0.00251702958693044));
#49730=CARTESIAN_POINT('Ctrl Pts',(-0.04,0.00362131197246112,0.00327619754187586));
#49731=CARTESIAN_POINT('Ctrl Pts',(-0.04,0.0042686552861704,0.00391548773053193));
#49732=CARTESIAN_POINT('Ctrl Pts',(-0.04,0.00503323066735754,0.0043491434857377));
#49733=CARTESIAN_POINT('',(-0.04,0.0075,0.005));
#49734=CARTESIAN_POINT('Origin',(-0.04,0.0075,0.));
#49735=CARTESIAN_POINT('',(-0.139,0.0075,0.005));
#49736=CARTESIAN_POINT('',(-0.14,0.0075,0.005));
#49737=CARTESIAN_POINT('',(-0.139,0.0075,-0.005));
#49738=CARTESIAN_POINT('Origin',(-0.139,0.0075,0.));
#49739=CARTESIAN_POINT('Origin',(-0.139,0.0075,0.));
#49740=CARTESIAN_POINT('Origin',(-0.04,0.0075,0.));
#49741=CARTESIAN_POINT('Ctrl Pts',(-0.127524898928341,0.00279679729590146,
0.00169705696579713));
#49742=CARTESIAN_POINT('Ctrl Pts',(-0.127516599909907,0.00279684927353385,
0.00169718012669082));
#49743=CARTESIAN_POINT('Ctrl Pts',(-0.127508299977955,0.00279687534251024,
0.00169724042141337));
#49744=CARTESIAN_POINT('Ctrl Pts',(-0.1275,0.002796875,0.00169723753033422));
#49745=CARTESIAN_POINT('Ctrl Pts',(-0.107524898928341,0.00279679729590146,
0.00169705696579713));
#49746=CARTESIAN_POINT('Ctrl Pts',(-0.107516599909907,0.00279684927353385,
0.00169718012669082));
#49747=CARTESIAN_POINT('Ctrl Pts',(-0.107508299977955,0.00279687534251023,
0.00169724042141337));
#49748=CARTESIAN_POINT('Ctrl Pts',(-0.1075,0.002796875,0.00169723753033422));
#49749=CARTESIAN_POINT('Ctrl Pts',(-0.0875248989283412,0.00279679729590146,
0.00169705696579712));
#49750=CARTESIAN_POINT('Ctrl Pts',(-0.0875165999099073,0.00279684927353385,
0.00169718012669082));
#49751=CARTESIAN_POINT('Ctrl Pts',(-0.0875082999779549,0.00279687534251024,
0.00169724042141337));
#49752=CARTESIAN_POINT('Ctrl Pts',(-0.0875,0.002796875,0.00169723753033423));
#49753=CARTESIAN_POINT('Ctrl Pts',(-0.0675248989283412,0.00279679729590146,
0.00169705696579713));
#49754=CARTESIAN_POINT('Ctrl Pts',(-0.0675165999099073,0.00279684927353385,
0.00169718012669082));
#49755=CARTESIAN_POINT('Ctrl Pts',(-0.0675082999779549,0.00279687534251024,
0.00169724042141337));
#49756=CARTESIAN_POINT('Ctrl Pts',(-0.0675,0.002796875,0.00169723753033423));
#49757=CARTESIAN_POINT('Ctrl Pts',(-0.0475248989283412,0.00279679729590146,
0.00169705696579713));
#49758=CARTESIAN_POINT('Ctrl Pts',(-0.0475165999099073,0.00279684927353385,
0.00169718012669083));
#49759=CARTESIAN_POINT('Ctrl Pts',(-0.0475082999779549,0.00279687534251024,
0.00169724042141337));
#49760=CARTESIAN_POINT('Ctrl Pts',(-0.0475,0.002796875,0.00169723753033423));
#49761=CARTESIAN_POINT('Origin',(0.,0.015,0.));
#49762=CARTESIAN_POINT('',(-5.65991084816151E-17,0.0148,-0.0165));
#49763=CARTESIAN_POINT('',(-5.65991084816151E-17,0.0002,-0.0165));
#49764=CARTESIAN_POINT('',(-5.65991084816151E-17,0.015,-0.0165));
#49765=CARTESIAN_POINT('',(-0.00839639405880103,0.0002,-0.0142038926639612));
#49766=CARTESIAN_POINT('Origin',(0.,0.0002,0.));
#49767=CARTESIAN_POINT('',(-0.00839639405880103,0.0148,-0.0142038926639612));
#49768=CARTESIAN_POINT('',(-0.00839639405880103,0.015,-0.0142038926639612));
#49769=CARTESIAN_POINT('Origin',(0.,0.0148,0.));
#49770=CARTESIAN_POINT('Origin',(-5.76094420909117E-17,0.015,-0.0165));
#49771=CARTESIAN_POINT('',(0.0125,0.0148,-0.0165));
#49772=CARTESIAN_POINT('',(0.0125,0.0002,-0.0165));
#49773=CARTESIAN_POINT('',(0.0125,0.015,-0.0165));
#49774=CARTESIAN_POINT('',(-5.73013858584659E-17,0.0002,-0.0165));
#49775=CARTESIAN_POINT('',(-5.76094420909117E-17,0.0148,-0.0165));
#49776=CARTESIAN_POINT('Origin',(0.,0.015,0.));
#49777=CARTESIAN_POINT('',(-0.00839639405880104,0.0148,0.0142038926639612));
#49778=CARTESIAN_POINT('',(-0.00839639405880104,0.0002,0.0142038926639612));
#49779=CARTESIAN_POINT('',(-0.00839639405880104,0.015,0.0142038926639612));
#49780=CARTESIAN_POINT('',(0.,0.0002,0.0165));
#49781=CARTESIAN_POINT('Origin',(0.,0.0002,0.));
#49782=CARTESIAN_POINT('',(0.,0.0148,0.0165));
#49783=CARTESIAN_POINT('',(0.,0.015,0.0165));
#49784=CARTESIAN_POINT('Origin',(0.,0.0148,0.));
#49785=CARTESIAN_POINT('Origin',(1.72828326272735E-16,0.015,0.0165));
#49786=CARTESIAN_POINT('',(0.0125000000000002,0.0002,0.0165));
#49787=CARTESIAN_POINT('',(1.72828326272735E-16,0.0002,0.0165));
#49788=CARTESIAN_POINT('',(0.0125000000000002,0.0148,0.0165));
#49789=CARTESIAN_POINT('',(0.0125000000000002,0.015,0.0165));
#49790=CARTESIAN_POINT('',(5.55111512312575E-20,0.0148,0.0165));
#49791=CARTESIAN_POINT('Origin',(0.0125,0.015,-4.59242549680257E-18));
#49792=CARTESIAN_POINT('Origin',(0.0125,0.0002,-4.59242549680257E-18));
#49793=CARTESIAN_POINT('Origin',(0.0125,0.0148,-4.59242549680257E-18));
#49794=CARTESIAN_POINT('Origin',(0.0125,0.015,-4.59242549680257E-18));
#49795=CARTESIAN_POINT('',(-0.0166089107357434,0.015,-0.00911686983553521));
#49796=CARTESIAN_POINT('',(-0.00376723863546634,0.015,-0.00239186662703728));
#49797=CARTESIAN_POINT('',(-0.00376723863546634,0.015,-0.00239186662703728));
#49798=CARTESIAN_POINT('',(-0.00376723863546634,0.015,0.00239186662703728));
#49799=CARTESIAN_POINT('Origin',(-0.00501982557395217,0.015,-2.16840434497101E-19));
#49800=CARTESIAN_POINT('',(-0.0166089107357433,0.015,0.00911686983553521));
#49801=CARTESIAN_POINT('',(-0.0169270413562866,0.015,0.00928347037066553));
#49802=CARTESIAN_POINT('',(-0.00829461958536103,0.015,0.0140317242680344));
#49803=CARTESIAN_POINT('',(-0.00829461958536103,0.015,0.0140317242680344));
#49804=CARTESIAN_POINT('',(-5.55111512312578E-20,0.015,0.0163));
#49805=CARTESIAN_POINT('Origin',(0.,0.015,0.));
#49806=CARTESIAN_POINT('',(0.0125000000000002,0.015,0.0163));
#49807=CARTESIAN_POINT('',(0.0125000000000002,0.015,0.0163));
#49808=CARTESIAN_POINT('',(0.0125,0.015,-0.0163));
#49809=CARTESIAN_POINT('Origin',(0.0125,0.015,-4.59242549680257E-18));
#49810=CARTESIAN_POINT('',(-5.5913058681838E-17,0.015,-0.0163));
#49811=CARTESIAN_POINT('',(0.0125,0.015,-0.0163));
#49812=CARTESIAN_POINT('',(-0.00829461958536102,0.015,-0.0140317242680344));
#49813=CARTESIAN_POINT('Origin',(0.,0.015,0.));
#49814=CARTESIAN_POINT('',(-0.0169180511005122,0.015,-0.00893412666903227));
#49815=CARTESIAN_POINT('',(0.,0.015,0.0115));
#49816=CARTESIAN_POINT('Origin',(0.,0.015,0.011));
#49817=CARTESIAN_POINT('',(0.,0.015,-0.0105));
#49818=CARTESIAN_POINT('Origin',(0.,0.015,-0.011));
#49819=CARTESIAN_POINT('',(0.0125,0.015,-0.0092));
#49820=CARTESIAN_POINT('Origin',(0.0125,0.015,-4.59242549680257E-18));
#49821=CARTESIAN_POINT('Origin',(0.0125,0.,-4.59242549680257E-18));
#49822=CARTESIAN_POINT('',(-0.0306415078475588,-1.19605085394936E-7,-0.000938136006279154));
#49823=CARTESIAN_POINT('',(-0.0206310823726759,0.,-0.00685120104972884));
#49824=CARTESIAN_POINT('Ctrl Pts',(-0.03064150786828,6.06630742267791E-51,
-0.000938136151692983));
#49825=CARTESIAN_POINT('Ctrl Pts',(-0.0289673468934464,7.16790888657192E-28,
-0.00191390121462454));
#49826=CARTESIAN_POINT('Ctrl Pts',(-0.0272875529435704,-1.0309211203299E-17,
-0.00288012983552212));
#49827=CARTESIAN_POINT('Ctrl Pts',(-0.0256190528013343,1.02955830966733E-17,
-0.00386547850042675));
#49828=CARTESIAN_POINT('Ctrl Pts',(-0.0239505526590982,3.09003774046027E-17,
-0.00485082716533138));
#49829=CARTESIAN_POINT('Ctrl Pts',(-0.022293347014245,1.90239552262182E-25,
-0.00585529628600419));
#49830=CARTESIAN_POINT('Ctrl Pts',(-0.0206310823726766,-1.73472347597923E-20,
-0.0068512010497298));
#49831=CARTESIAN_POINT('',(-0.018277353250021,3.08514507815582E-8,-0.00813059850575379));
#49832=CARTESIAN_POINT('Ctrl Pts',(-0.0206310823726745,0.,-0.00685120104972968));
#49833=CARTESIAN_POINT('Ctrl Pts',(-0.0198643807345651,1.57511708648874E-27,
-0.0073105513809931));
#49834=CARTESIAN_POINT('Ctrl Pts',(-0.0190726109028725,0.,-0.0077237863538248));
#49835=CARTESIAN_POINT('Ctrl Pts',(-0.0182773531828187,0.,-0.00813059853874281));
#49836=CARTESIAN_POINT('',(-0.00829461958536102,0.,-0.0140317242680344));
#49837=CARTESIAN_POINT('',(0.00096849183839154,0.,-0.0195074579675537));
#49838=CARTESIAN_POINT('',(-5.5913058681838E-17,0.,-0.0163));
#49839=CARTESIAN_POINT('Origin',(0.,0.,0.));
#49840=CARTESIAN_POINT('',(0.0125,0.,-0.0163));
#49841=CARTESIAN_POINT('',(0.0125,0.,-0.0163));
#49842=CARTESIAN_POINT('',(0.0125000000000002,0.,0.0163));
#49843=CARTESIAN_POINT('Origin',(0.0125,0.,-4.59242549680257E-18));
#49844=CARTESIAN_POINT('',(0.,0.,0.0163));
#49845=CARTESIAN_POINT('',(0.0125,0.,0.0163));
#49846=CARTESIAN_POINT('',(-0.00829461958536103,0.,0.0140317242680344));
#49847=CARTESIAN_POINT('Origin',(0.,0.,0.));
#49848=CARTESIAN_POINT('',(-0.0183185438988578,2.99066327258402E-17,0.00810624909661309));
#49849=CARTESIAN_POINT('',(0.000968491838391539,0.,0.0195074579675537));
#49850=CARTESIAN_POINT('',(-0.0206729454446971,0.,0.0068262100906602));
#49851=CARTESIAN_POINT('Ctrl Pts',(-0.0183185440091374,0.,0.00810624927278113));
#49852=CARTESIAN_POINT('Ctrl Pts',(-0.0191139452258369,0.,0.00769907071789008));
#49853=CARTESIAN_POINT('Ctrl Pts',(-0.0199059893503628,2.20596951890412E-24,
0.00728571135373499));
#49854=CARTESIAN_POINT('Ctrl Pts',(-0.0206729454446971,6.6121838851786E-30,
0.00682621009066024));
#49855=CARTESIAN_POINT('',(-0.0306415862453137,-8.66279905141487E-8,0.000938073089450988));
#49856=CARTESIAN_POINT('Ctrl Pts',(-0.0206729454446971,-2.71050543121376E-20,
0.00682621009066024));
#49857=CARTESIAN_POINT('Ctrl Pts',(-0.0223282407769415,-2.71050543121376E-20,
0.00583448409485697));
#49858=CARTESIAN_POINT('Ctrl Pts',(-0.0239784617686096,-6.77626357803436E-21,
0.00483419474493695));
#49859=CARTESIAN_POINT('Ctrl Pts',(-0.0256400041972464,2.42311502295287E-35,
0.00385301122208682));
#49860=CARTESIAN_POINT('Ctrl Pts',(-0.0273015466258831,6.77626357803439E-21,
0.00287182769923668));
#49861=CARTESIAN_POINT('Ctrl Pts',(-0.0289744104914885,0.,0.00190975000345643));
#49862=CARTESIAN_POINT('Ctrl Pts',(-0.0306415862989849,0.,0.000938073256321053));
#49863=CARTESIAN_POINT('Ctrl Pts',(-0.0306415862453137,-8.66279905141357E-8,
0.000938073089450988));
#49864=CARTESIAN_POINT('Ctrl Pts',(-0.0308898601383488,2.57926462655969E-8,
0.000793373576933981));
#49865=CARTESIAN_POINT('Ctrl Pts',(-0.0310667270502054,1.08407425174632E-7,
0.000550378915350664));
#49866=CARTESIAN_POINT('Ctrl Pts',(-0.0311372956334381,1.45622331613657E-7,
0.00028264191180899));
#49867=CARTESIAN_POINT('Ctrl Pts',(-0.0311615868604397,1.5843250433844E-7,
0.000190481065837118));
#49868=CARTESIAN_POINT('Ctrl Pts',(-0.0311737818075073,1.66200756503995E-7,
9.53821800403144E-5));
#49869=CARTESIAN_POINT('Ctrl Pts',(-0.0311737532392636,1.64882298400146E-7,
1.60473702184294E-7));
#49870=CARTESIAN_POINT('Ctrl Pts',(-0.0311736711029301,1.61091609846496E-7,
-0.000273610707362422));
#49871=CARTESIAN_POINT('Ctrl Pts',(-0.0310696664268064,9.52873903898754E-8,
-0.000547409293633988));
#49872=CARTESIAN_POINT('Ctrl Pts',(-0.030877772516319,-5.72693113770487E-10,
-0.000750518444677997));
#49873=CARTESIAN_POINT('Ctrl Pts',(-0.0308090257338665,-3.49149621819306E-8,
-0.000823283133174159));
#49874=CARTESIAN_POINT('Ctrl Pts',(-0.0307294370403642,-7.72395171728875E-8,
-0.000886888142082073));
#49875=CARTESIAN_POINT('Ctrl Pts',(-0.0306415078475588,-1.19605085394879E-7,
-0.000938136006279154));
#49876=CARTESIAN_POINT('',(0.00625,0.,-0.0121912878729033));
#49877=CARTESIAN_POINT('',(0.00625,0.,0.0121912878729033));
#49878=CARTESIAN_POINT('Origin',(0.,0.,0.));
#49879=CARTESIAN_POINT('Origin',(0.0125,0.,-4.59242549680257E-18));
#49880=CARTESIAN_POINT('Origin',(0.,0.001,0.));
#49881=CARTESIAN_POINT('',(0.00625,0.001,0.0119660979437743));
#49882=CARTESIAN_POINT('',(0.00625,0.0002,0.0119660979437743));
#49883=CARTESIAN_POINT('',(0.00625,0.001,0.0119660979437743));
#49884=CARTESIAN_POINT('',(0.00625,0.0002,-0.0119660979437743));
#49885=CARTESIAN_POINT('Origin',(0.,0.0002,0.));
#49886=CARTESIAN_POINT('',(0.00625,0.001,-0.0119660979437743));
#49887=CARTESIAN_POINT('',(0.00625,0.001,-0.0119660979437743));
#49888=CARTESIAN_POINT('Origin',(0.,0.001,0.));
#49889=CARTESIAN_POINT('Origin',(0.0125,0.001,-4.59242549680257E-18));
#49890=CARTESIAN_POINT('Origin',(0.0125,0.0002,-4.59242549680257E-18));
#49891=CARTESIAN_POINT('Origin',(0.0125,0.001,-4.59242549680257E-18));
#49892=CARTESIAN_POINT('Origin',(0.00625,0.001,-2.29621274840129E-18));
#49893=CARTESIAN_POINT('',(-0.000371408500209017,0.001,0.0126945679613751));
#49894=CARTESIAN_POINT('',(0.00625,0.001,0.0110556546617557));
#49895=CARTESIAN_POINT('Origin',(0.,0.001,0.));
#49896=CARTESIAN_POINT('',(0.00625,0.001,-0.0110556546617557));
#49897=CARTESIAN_POINT('Origin',(0.0125,0.001,-4.59242549680257E-18));
#49898=CARTESIAN_POINT('',(-0.000371408500209017,0.001,-0.0126945679613751));
#49899=CARTESIAN_POINT('Origin',(0.,0.001,0.));
#49900=CARTESIAN_POINT('',(-0.000492372526715892,0.001,-0.0126720993701079));
#49901=CARTESIAN_POINT('Origin',(-0.000359710594690623,0.001,-0.0122947390492059));
#49902=CARTESIAN_POINT('',(-0.00872901544041542,0.001,-0.00439918826870923));
#49903=CARTESIAN_POINT('Origin',(0.00396253460616978,0.001,0.));
#49904=CARTESIAN_POINT('',(-0.0087336051435635,0.001,-0.00440088102636655));
#49905=CARTESIAN_POINT('Origin',(-0.00866210908617835,0.001,-0.00458766516321543));
#49906=CARTESIAN_POINT('Origin',(-0.00926982557395217,0.001,-0.003));
#49907=CARTESIAN_POINT('',(-0.0087336051435635,0.001,0.00440088102636655));
#49908=CARTESIAN_POINT('Origin',(-0.00926982557395217,0.001,0.003));
#49909=CARTESIAN_POINT('',(-0.00872901544041542,0.001,0.00439918826870923));
#49910=CARTESIAN_POINT('Origin',(-0.00866210908617835,0.001,0.00458766516321543));
#49911=CARTESIAN_POINT('',(-0.000492372526715893,0.001,0.0126720993701079));
#49912=CARTESIAN_POINT('Origin',(0.00396253460616978,0.001,0.));
#49913=CARTESIAN_POINT('Origin',(-0.000359710594690623,0.001,0.0122947390492058));
#49914=CARTESIAN_POINT('Origin',(0.0125,0.0134,-4.59242549680257E-18));
#49915=CARTESIAN_POINT('',(0.0125,0.0134,-0.0123));
#49916=CARTESIAN_POINT('Origin',(0.0125,0.0134,-4.59242549680257E-18));
#49917=CARTESIAN_POINT('',(0.0125,0.0134,-0.0092));
#49918=CARTESIAN_POINT('Origin',(0.0125,0.0134,-4.59242549680257E-18));
#49919=CARTESIAN_POINT('Origin',(0.0125,0.015,-4.59242549680257E-18));
#49920=CARTESIAN_POINT('',(0.0125,0.0148,0.00899999999999999));
#49921=CARTESIAN_POINT('',(0.0125,0.0148,-0.009));
#49922=CARTESIAN_POINT('Origin',(0.0125,0.0148,-4.59242549680257E-18));
#49923=CARTESIAN_POINT('Origin',(0.0125,0.0148,-4.59242549680257E-18));
#49924=CARTESIAN_POINT('',(0.0125,0.0136,0.00899999999999999));
#49925=CARTESIAN_POINT('',(0.0125,0.015,0.00899999999999999));
#49926=CARTESIAN_POINT('',(0.0125,0.0136,-0.009));
#49927=CARTESIAN_POINT('Origin',(0.0125,0.0136,-4.59242549680257E-18));
#49928=CARTESIAN_POINT('Origin',(0.0125,0.0136,-4.59242549680257E-18));
#49929=CARTESIAN_POINT('Origin',(-0.00839639405880103,0.015,0.0142038926639612));
#49930=CARTESIAN_POINT('',(-0.0171157106796651,0.0132,0.00904961418521835));
#49931=CARTESIAN_POINT('',(-0.0175612941370424,0.0132,0.00878621496200997));
#49932=CARTESIAN_POINT('',(-0.0215570023002331,0.0132,0.00642421877717253));
#49933=CARTESIAN_POINT('',(-0.0150672706217452,0.0114767391344914,0.010260629200748));
#49934=CARTESIAN_POINT('Ctrl Pts',(-0.0175612941370424,0.0132,0.00878621496200996));
#49935=CARTESIAN_POINT('Ctrl Pts',(-0.0173229778501341,0.013111161537897,
0.00892709165707185));
#49936=CARTESIAN_POINT('Ctrl Pts',(-0.0170864812350933,0.0130160222101977,
0.00906689268348295));
#49937=CARTESIAN_POINT('Ctrl Pts',(-0.0168527050452293,0.0129128930140674,
0.0092050855759598));
#49938=CARTESIAN_POINT('Ctrl Pts',(-0.0166189288553652,0.012809763817937,
0.00934327846843666));
#49939=CARTESIAN_POINT('Ctrl Pts',(-0.0163878730912532,0.0126986447513118,
0.00947986322663923));
#49940=CARTESIAN_POINT('Ctrl Pts',(-0.0161611109731713,0.0125744273552869,
0.00961390986766));
#49941=CARTESIAN_POINT('Ctrl Pts',(-0.0159343488550895,0.0124502099592619,
0.00974795650868077));
#49942=CARTESIAN_POINT('Ctrl Pts',(-0.0157118803918583,0.0123128942200067,
0.00987946502730567));
#49943=CARTESIAN_POINT('Ctrl Pts',(-0.0155076135681626,0.0121472852270145,
0.0100002139505386));
#49944=CARTESIAN_POINT('Ctrl Pts',(-0.0154054801563147,0.0120644807305183,
0.010060588412155));
#49945=CARTESIAN_POINT('Ctrl Pts',(-0.0153078971638308,0.0119746028996598,
0.0101182729693195));
#49946=CARTESIAN_POINT('Ctrl Pts',(-0.0152234095810172,0.0118644951654366,
0.0101682163936442));
#49947=CARTESIAN_POINT('Ctrl Pts',(-0.0151389219982035,0.0117543874312135,
0.0102181598179688));
#49948=CARTESIAN_POINT('Ctrl Pts',(-0.0150675299392406,0.0116240498354857,
0.0102603620419579));
#49949=CARTESIAN_POINT('Ctrl Pts',(-0.0150672200690482,0.0114767391349546,
0.0102605452165499));
#49950=CARTESIAN_POINT('',(-0.0150696760858911,0.00250000000230064,0.0102591396094456));
#49951=CARTESIAN_POINT('Ctrl Pts',(-0.0150672705003522,0.0114767391348364,
0.0102606292735785));
#49952=CARTESIAN_POINT('Ctrl Pts',(-0.0150659075926703,0.0108260833645536,
0.0102614460562153));
#49953=CARTESIAN_POINT('Ctrl Pts',(-0.0150649244414608,0.0101240231335967,
0.0102620375058781));
#49954=CARTESIAN_POINT('Ctrl Pts',(-0.0150643215473666,0.00937866249945708,
0.0102624001187059));
#49955=CARTESIAN_POINT('Ctrl Pts',(-0.0150640201003195,0.00900598218238727,
0.0102625814251198));
#49956=CARTESIAN_POINT('Ctrl Pts',(-0.0150638137327322,0.00862247676452173,
0.0102627055478026));
#49957=CARTESIAN_POINT('Ctrl Pts',(-0.0150637004162104,0.00822004218836817,
0.0102627735152981));
#49958=CARTESIAN_POINT('Ctrl Pts',(-0.0150635870996886,0.00781760761221461,
0.0102628414827935));
#49959=CARTESIAN_POINT('Ctrl Pts',(-0.015063566834431,0.00739624387777302,
0.0102628532955054));
#49960=CARTESIAN_POINT('Ctrl Pts',(-0.0150636473733159,0.00698836721501205,
0.0102628042599833));
#49961=CARTESIAN_POINT('Ctrl Pts',(-0.0150638084510857,0.00617261388949012,
0.010262706188939));
#49962=CARTESIAN_POINT('Ctrl Pts',(-0.0150643726537689,0.00541080885069056,
0.0102623645778269));
#49963=CARTESIAN_POINT('Ctrl Pts',(-0.0150653755701918,0.00466676809321675,
0.010261759642764));
#49964=CARTESIAN_POINT('Ctrl Pts',(-0.0150663784866148,0.00392272733574294,
0.0102611547077011));
#49965=CARTESIAN_POINT('Ctrl Pts',(-0.015067820129422,0.00319645085959551,
0.0102602864595939));
#49966=CARTESIAN_POINT('Ctrl Pts',(-0.0150696910491641,0.0024999999999077,
0.0102591654099954));
#49967=CARTESIAN_POINT('',(-0.0150726550660005,0.00138682640630969,0.0102573320455256));
#49968=CARTESIAN_POINT('',(-0.015069656672316,0.00249999999999522,0.0102591080098914));
#49969=CARTESIAN_POINT('',(-0.0167335787825944,0.0002,0.00927550507767659));
#49970=CARTESIAN_POINT('Ctrl Pts',(-0.0150726552252303,0.00138682640630866,
0.0102573323146958));
#49971=CARTESIAN_POINT('Ctrl Pts',(-0.0150731971649166,0.00118574953270313,
0.0102570119560962));
#49972=CARTESIAN_POINT('Ctrl Pts',(-0.0152081064597958,0.00103259595613278,
0.0101772625783165));
#49973=CARTESIAN_POINT('Ctrl Pts',(-0.0153485028614304,0.000910488615915601,
0.0100942695889684));
#49974=CARTESIAN_POINT('Ctrl Pts',(-0.0154888992630651,0.000788381275698425,
0.0100112765996203));
#49975=CARTESIAN_POINT('Ctrl Pts',(-0.0156347825636464,0.000697320245644121,
0.00992504012154639));
#49976=CARTESIAN_POINT('Ctrl Pts',(-0.0157861198041517,0.000614449925209533,
0.00983557963792288));
#49977=CARTESIAN_POINT('Ctrl Pts',(-0.0159374570446571,0.000531579604774943,
0.00974611915429937));
#49978=CARTESIAN_POINT('Ctrl Pts',(-0.0160942482158647,0.000456899963464771,
0.0096534346705775));
#49979=CARTESIAN_POINT('Ctrl Pts',(-0.0162528722771886,0.000388514508127937,
0.00955966670445773));
#49980=CARTESIAN_POINT('Ctrl Pts',(-0.0164114963385125,0.000320129052791105,
0.00946589873833796));
#49981=CARTESIAN_POINT('Ctrl Pts',(-0.0165719532869742,0.000258037776486399,
0.00937104729158102));
#49982=CARTESIAN_POINT('Ctrl Pts',(-0.01673357878255,0.000200000000015906,
0.00927550507770282));
#49983=CARTESIAN_POINT('',(-0.00839639405880103,0.0002,0.0142038926639612));
#49984=CARTESIAN_POINT('',(-0.0167106852091834,0.0148,0.009289038231462));
#49985=CARTESIAN_POINT('',(-0.0170198255739522,0.0148,0.00910629506495906));
#49986=CARTESIAN_POINT('',(-0.0167106852091834,0.0136,0.009289038231462));
#49987=CARTESIAN_POINT('',(-0.0167106852091834,0.015,0.009289038231462));
#49988=CARTESIAN_POINT('Origin',(-0.0171157106796651,0.0136,0.00904961418521835));
#49989=CARTESIAN_POINT('Origin',(-0.00839639405880103,0.015,-0.0142038926639612));
#49990=CARTESIAN_POINT('',(-0.0166926437830517,0.0002,-0.00929970311937464));
#49991=CARTESIAN_POINT('',(-0.00839639405880103,0.0002,-0.0142038926639612));
#49992=CARTESIAN_POINT('',(-0.01504752612516,0.00139784887637815,-0.0102721865570626));
#49993=CARTESIAN_POINT('Ctrl Pts',(-0.0166926437830517,0.000199999999999716,
-0.00929970311937462));
#49994=CARTESIAN_POINT('Ctrl Pts',(-0.0165313761725789,0.000258323117271339,
-0.00939503377544802));
#49995=CARTESIAN_POINT('Ctrl Pts',(-0.0163717374471408,0.00032059129430158,
-0.00948940154332222));
#49996=CARTESIAN_POINT('Ctrl Pts',(-0.0162138266410766,0.000389342010301485,
-0.00958274788050075));
#49997=CARTESIAN_POINT('Ctrl Pts',(-0.0160559158350124,0.000458092726301389,
-0.00967609421767928));
#49998=CARTESIAN_POINT('Ctrl Pts',(-0.015899732950897,0.000533325987099894,
-0.00976841912264));
#49999=CARTESIAN_POINT('Ctrl Pts',(-0.0157484005065699,0.000617287381555205,
-0.00985787677108282));
#50000=CARTESIAN_POINT('Ctrl Pts',(-0.0155970680622428,0.000701248776010517,
-0.00994733441952563));
#50001=CARTESIAN_POINT('Ctrl Pts',(-0.0154505860660156,0.000793938331462511,
-0.0100339248065372));
#50002=CARTESIAN_POINT('Ctrl Pts',(-0.0153122611083508,0.000918161762487361,
-0.0101156932963588));
#50003=CARTESIAN_POINT('Ctrl Pts',(-0.015173936150686,0.00104238519351221,
-0.0101974617861805));
#50004=CARTESIAN_POINT('Ctrl Pts',(-0.015043768415608,0.00119814242791505,
-0.0102744082700292));
#50005=CARTESIAN_POINT('Ctrl Pts',(-0.0150475263029645,0.00139784887637434,
-0.0102721868576446));
#50006=CARTESIAN_POINT('',(-0.0150682948691039,0.00250188254723652,-0.0102598985791645));
#50007=CARTESIAN_POINT('',(-0.0150475257696179,0.00139784887638291,-0.0102721859558591));
#50008=CARTESIAN_POINT('',(-0.0151696828310441,0.00750413531507349,-0.0101999796192979));
#50009=CARTESIAN_POINT('Ctrl Pts',(-0.0150682998181951,0.00250188254704829,
-0.0102599069408648));
#50010=CARTESIAN_POINT('Ctrl Pts',(-0.0150967279280264,0.00401291028492777,
-0.0102431021382563));
#50011=CARTESIAN_POINT('Ctrl Pts',(-0.0151305217455447,0.00568032787429946,
-0.0102231254871123));
#50012=CARTESIAN_POINT('Ctrl Pts',(-0.0151696812707501,0.00750413531516336,
-0.0101999769874327));
#50013=CARTESIAN_POINT('',(-0.0152584725567155,0.0114711480137007,-0.0101474887966015));
#50014=CARTESIAN_POINT('Ctrl Pts',(-0.01516968127075,0.00750413531516336,
-0.0101999769874327));
#50015=CARTESIAN_POINT('Ctrl Pts',(-0.0152015623713677,0.00898895812500316,
-0.0101811310069577));
#50016=CARTESIAN_POINT('Ctrl Pts',(-0.0152311595696551,0.0103112956911785,
-0.0101636351172226));
#50017=CARTESIAN_POINT('Ctrl Pts',(-0.0152584728656123,0.0114711480136893,
-0.0101474893182275));
#50018=CARTESIAN_POINT('',(-0.0177200739051674,0.0132,-0.00869235495241383));
#50019=CARTESIAN_POINT('Ctrl Pts',(-0.0152584728656124,0.0114711480136919,
-0.0101474893182275));
#50020=CARTESIAN_POINT('Ctrl Pts',(-0.0152619549961719,0.0116190061218255,
-0.0101454309148705));
#50021=CARTESIAN_POINT('Ctrl Pts',(-0.0153327035891074,0.0117490011390277,
-0.0101036090650828));
#50022=CARTESIAN_POINT('Ctrl Pts',(-0.0154162085456889,0.0118593137698746,
-0.0100542465038534));
#50023=CARTESIAN_POINT('Ctrl Pts',(-0.0154997135022704,0.0119696264007216,
-0.0100048839426239));
#50024=CARTESIAN_POINT('Ctrl Pts',(-0.0155959746753244,0.0120602565912413,
-0.00994798075695177));
#50025=CARTESIAN_POINT('Ctrl Pts',(-0.0156967904973433,0.0121437216331223,
-0.00988838516656967));
#50026=CARTESIAN_POINT('Ctrl Pts',(-0.0158984221413811,0.0123106517168843,
-0.00976919398580547));
#50027=CARTESIAN_POINT('Ctrl Pts',(-0.0161182723237525,0.0124489213294069,
-0.00963923322020681));
#50028=CARTESIAN_POINT('Ctrl Pts',(-0.0163414673925833,0.0125735141295264,
-0.0095072951808101));
#50029=CARTESIAN_POINT('Ctrl Pts',(-0.0165646624614141,0.0126981069296459,
-0.0093753571414134));
#50030=CARTESIAN_POINT('Ctrl Pts',(-0.0167912024035204,0.0128090229374379,
-0.00924144183601202));
#50031=CARTESIAN_POINT('Ctrl Pts',(-0.017021176870325,0.012912202521094,
-0.00910549626866394));
#50032=CARTESIAN_POINT('Ctrl Pts',(-0.0172511513371295,0.0130153821047501,
-0.00896955070131585));
#50033=CARTESIAN_POINT('Ctrl Pts',(-0.0174845603276081,0.0131108252678533,
-0.00883157487262645));
#50034=CARTESIAN_POINT('Ctrl Pts',(-0.017720073905168,0.0132,-0.00869235495241341));
#50035=CARTESIAN_POINT('',(-0.0171157106796651,0.0132,-0.00904961418521835));
#50036=CARTESIAN_POINT('',(-0.0170198255739522,0.0132,-0.00910629506495906));
#50037=CARTESIAN_POINT('',(-0.0167106852091834,0.0136,-0.00928903823146201));
#50038=CARTESIAN_POINT('Origin',(-0.0171157106796651,0.0136,-0.00904961418521834));
#50039=CARTESIAN_POINT('',(-0.0167106852091834,0.0148,-0.00928903823146201));
#50040=CARTESIAN_POINT('',(-0.0167106852091834,0.015,-0.00928903823146201));
#50041=CARTESIAN_POINT('',(-0.00839639405880103,0.0148,-0.0142038926639612));
#50042=CARTESIAN_POINT('Ctrl Pts',(-0.04,0.00503323066735754,0.0043491434857377));
#50043=CARTESIAN_POINT('Ctrl Pts',(-0.0373335531119965,0.00503323066735754,
0.0043491434857377));
#50044=CARTESIAN_POINT('Ctrl Pts',(-0.0349552522444544,0.00493945518810382,
0.0044470975219459));
#50045=CARTESIAN_POINT('Ctrl Pts',(-0.0327211769482695,0.00477742014678961,
0.00468135238095731));
#50046=CARTESIAN_POINT('Ctrl Pts',(-0.04,0.00426866982654043,0.00391549597761299));
#50047=CARTESIAN_POINT('Ctrl Pts',(-0.037357541268117,0.00426866982654043,
0.00391549597761299));
#50048=CARTESIAN_POINT('Ctrl Pts',(-0.0349933516210969,0.00420319701705448,
0.00397919554166179));
#50049=CARTESIAN_POINT('Ctrl Pts',(-0.032766245054209,0.00409006624844954,
0.00414731897802562));
#50050=CARTESIAN_POINT('Ctrl Pts',(-0.04,0.00297384830823641,0.00263671750932495));
#50051=CARTESIAN_POINT('Ctrl Pts',(-0.0374055174496866,0.00297384830823641,
0.00263671750932495));
#50052=CARTESIAN_POINT('Ctrl Pts',(-0.0350694792794186,0.00295630750671264,
0.00265761922721007));
#50053=CARTESIAN_POINT('Ctrl Pts',(-0.0328562262229028,0.00292599858475061,
0.00273220367477735));
#50054=CARTESIAN_POINT('Ctrl Pts',(-0.04,0.00226235348654652,4.2227252587527E-7));
#50055=CARTESIAN_POINT('Ctrl Pts',(-0.0374076766156412,0.00226235348654652,
4.2227252587527E-7));
#50056=CARTESIAN_POINT('Ctrl Pts',(-0.0350724447670342,0.00227115110622434,
-5.69710842301547E-7));
#50057=CARTESIAN_POINT('Ctrl Pts',(-0.0328592699289883,0.00228635233847694,
-1.75243967904944E-6));
#50058=CARTESIAN_POINT('Ctrl Pts',(-0.04,0.00297342320919197,-0.00263598765508364));
#50059=CARTESIAN_POINT('Ctrl Pts',(-0.0374055078715638,0.00297342320919197,
-0.00263598765508364));
#50060=CARTESIAN_POINT('Ctrl Pts',(-0.0350685208298449,0.00295589853021904,
-0.00265886669139246));
#50061=CARTESIAN_POINT('Ctrl Pts',(-0.0328541484702436,0.00292561725632549,
-0.0027358064165028));
#50062=CARTESIAN_POINT('Ctrl Pts',(-0.04,0.00426803851384994,-0.00391497489042477));
#50063=CARTESIAN_POINT('Ctrl Pts',(-0.0373575346994387,0.00426803851384994,
-0.00391497489042477));
#50064=CARTESIAN_POINT('Ctrl Pts',(-0.034991910923473,0.00420258965996815,
-0.00398063923938531));
#50065=CARTESIAN_POINT('Ctrl Pts',(-0.03276310942731,0.00408949996568061,
-0.00415109891161779));
#50066=CARTESIAN_POINT('Ctrl Pts',(-0.04,0.00503252942117453,-0.00434874567463202));
#50067=CARTESIAN_POINT('Ctrl Pts',(-0.037333548178702,0.00503252942117453,
-0.00434874567463202));
#50068=CARTESIAN_POINT('Ctrl Pts',(-0.034953641512335,0.00493878055701564,
-0.00444865672873833));
#50069=CARTESIAN_POINT('Ctrl Pts',(-0.032717667415586,0.00477679114689861,
-0.00468523614631841));
#50070=CARTESIAN_POINT('',(-0.0327968762032639,0.00420554807594454,-0.00417120478069329));
#50071=CARTESIAN_POINT('Ctrl Pts',(-0.0327968795935294,0.00420555000362145,
-0.00417120625622339));
#50072=CARTESIAN_POINT('Ctrl Pts',(-0.0336175849861136,0.00434997248243195,
-0.00420475803964206));
#50073=CARTESIAN_POINT('Ctrl Pts',(-0.0344378865182222,0.0044959788927343,
-0.00423892428362857));
#50074=CARTESIAN_POINT('Ctrl Pts',(-0.0352615686182026,0.00462509266287838,
-0.00426736268617292));
#50075=CARTESIAN_POINT('Ctrl Pts',(-0.0360317364760486,0.00474581797155349,
-0.00429395345895852));
#50076=CARTESIAN_POINT('Ctrl Pts',(-0.0368048362410686,0.00485177839771797,
-0.00431592424605144));
#50077=CARTESIAN_POINT('Ctrl Pts',(-0.0375815336438874,0.00492019429147787,
-0.0043277496851657));
#50078=CARTESIAN_POINT('Ctrl Pts',(-0.0383853608252005,0.00499099992934722,
-0.00433998818288245));
#50079=CARTESIAN_POINT('Ctrl Pts',(-0.0391930521783087,0.00502105452742686,
-0.00434223485095487));
#50080=CARTESIAN_POINT('Ctrl Pts',(-0.0399999990786921,0.00503252942117453,
-0.00434874567463202));
#50081=CARTESIAN_POINT('',(-0.0364391610694964,0.00340557668880199,-0.00293086975220478));
#50082=CARTESIAN_POINT('Ctrl Pts',(-0.0327968763819142,0.00420554873112458,
-0.00417120302188662));
#50083=CARTESIAN_POINT('Ctrl Pts',(-0.0328215632400491,0.00420048893979486,
-0.00416276786668299));
#50084=CARTESIAN_POINT('Ctrl Pts',(-0.0328462592609637,0.00419541111203618,
-0.00415433766263343));
#50085=CARTESIAN_POINT('Ctrl Pts',(-0.0328709631528736,0.00419031601120015,
-0.00414591186122784));
#50086=CARTESIAN_POINT('Ctrl Pts',(-0.0330092657588975,0.00416179152905996,
-0.00409874073950808));
#50087=CARTESIAN_POINT('Ctrl Pts',(-0.0331477652015767,0.00413273014284505,
-0.00405173072279408));
#50088=CARTESIAN_POINT('Ctrl Pts',(-0.0332860718111478,0.00410328863811645,
-0.00400491481922219));
#50089=CARTESIAN_POINT('Ctrl Pts',(-0.0334147601364774,0.00407589458984604,
-0.00396135464340599));
#50090=CARTESIAN_POINT('Ctrl Pts',(-0.0335432958668976,0.00404817007233707,
-0.00391795487705723));
#50091=CARTESIAN_POINT('Ctrl Pts',(-0.0336714989161663,0.00402023339740768,
-0.00387471114131506));
#50092=CARTESIAN_POINT('Ctrl Pts',(-0.0336837720381774,0.00401755896632395,
-0.00387057133615437));
#50093=CARTESIAN_POINT('Ctrl Pts',(-0.0336960424060585,0.00401488256503795,
-0.00386643283303635));
#50094=CARTESIAN_POINT('Ctrl Pts',(-0.0337083098547249,0.00401220430028142,
-0.00386229565129054));
#50095=CARTESIAN_POINT('Ctrl Pts',(-0.0338164503700708,0.00398859475123179,
-0.00382582539751267));
#50096=CARTESIAN_POINT('Ctrl Pts',(-0.0339242916194723,0.00396485019215915,
-0.00378947774226141));
#50097=CARTESIAN_POINT('Ctrl Pts',(-0.0340330956396721,0.00394073017346232,
-0.00375277414638576));
#50098=CARTESIAN_POINT('Ctrl Pts',(-0.0340765868380846,0.00393108890729467,
-0.00373810296633425));
#50099=CARTESIAN_POINT('Ctrl Pts',(-0.0341202308469956,0.00392138799822184,
-0.00372337504059853));
#50100=CARTESIAN_POINT('Ctrl Pts',(-0.0341640923441276,0.00391161467659147,
-0.00370856653712364));
#50101=CARTESIAN_POINT('Ctrl Pts',(-0.0343176842555536,0.00387739096676982,
-0.00365671088916841));
#50102=CARTESIAN_POINT('Ctrl Pts',(-0.0344740450561803,0.00384224880621381,
-0.00360383719676782));
#50103=CARTESIAN_POINT('Ctrl Pts',(-0.0346199413654582,0.00380932113143792,
-0.00355433783745459));
#50104=CARTESIAN_POINT('Ctrl Pts',(-0.0346472426152604,0.00380315944935759,
-0.00354507513313842));
#50105=CARTESIAN_POINT('Ctrl Pts',(-0.0346741609330305,0.00379707968931115,
-0.0035359367135654));
#50106=CARTESIAN_POINT('Ctrl Pts',(-0.0347008875072039,0.00379104028287026,
-0.00352685777939867));
#50107=CARTESIAN_POINT('Ctrl Pts',(-0.0348169862087886,0.00376480544852224,
-0.00348741941136502));
#50108=CARTESIAN_POINT('Ctrl Pts',(-0.0349296502264305,0.00373928845294353,
-0.00344904799014247));
#50109=CARTESIAN_POINT('Ctrl Pts',(-0.0350527857045229,0.00371144178408232,
-0.00340701244398427));
#50110=CARTESIAN_POINT('Ctrl Pts',(-0.0351285266834232,0.00369431321974542,
-0.00338115626131496));
#50111=CARTESIAN_POINT('Ctrl Pts',(-0.0352082756719269,0.00367630004581376,
-0.00335389864567627));
#50112=CARTESIAN_POINT('Ctrl Pts',(-0.0352855219259208,0.00365889457268727,
-0.00332745545077473));
#50113=CARTESIAN_POINT('Ctrl Pts',(-0.0352950361946265,0.00365675077490146,
-0.00332419849462838));
#50114=CARTESIAN_POINT('Ctrl Pts',(-0.0353045108873918,0.00365461653476455,
-0.00332095448530997));
#50115=CARTESIAN_POINT('Ctrl Pts',(-0.0353140452347724,0.00365246957958181,
-0.00331768947106946));
#50116=CARTESIAN_POINT('Ctrl Pts',(-0.0353432155236711,0.003645900980764,
-0.00330770017606563));
#50117=CARTESIAN_POINT('Ctrl Pts',(-0.035372952324594,0.00363921098688231,
-0.00329751177977544));
#50118=CARTESIAN_POINT('Ctrl Pts',(-0.0354060246459562,0.00363178204943183,
-0.00328617448683469));
#50119=CARTESIAN_POINT('Ctrl Pts',(-0.0354499066991535,0.00362192495398237,
-0.00327113158475073));
#50120=CARTESIAN_POINT('Ctrl Pts',(-0.0354996695841126,0.003610770528947,
-0.00325405419777999));
#50121=CARTESIAN_POINT('Ctrl Pts',(-0.0355293049097754,0.00360413703833009,
-0.00324387808159859));
#50122=CARTESIAN_POINT('Ctrl Pts',(-0.0355589402354383,0.00359750354771319,
-0.00323370196541719));
#50123=CARTESIAN_POINT('Ctrl Pts',(-0.035568441838183,0.00359537779213524,
-0.00323043241565654));
#50124=CARTESIAN_POINT('Ctrl Pts',(-0.0355865697128671,0.00359132226877824,
-0.00322419580591136));
#50125=CARTESIAN_POINT('Ctrl Pts',(-0.0356046975875512,0.00358726674542124,
-0.00321795919616619));
#50126=CARTESIAN_POINT('Ctrl Pts',(-0.0356314515535437,0.00358128594405739,
-0.00320875208760797));
#50127=CARTESIAN_POINT('Ctrl Pts',(-0.0356598137894403,0.00357495996564327,
-0.00319898802663048));
#50128=CARTESIAN_POINT('Ctrl Pts',(-0.0357165382612333,0.00356230800881504,
-0.0031794599046755));
#50129=CARTESIAN_POINT('Ctrl Pts',(-0.0357796961244657,0.00354826678936026,
-0.00315771038066871));
#50130=CARTESIAN_POINT('Ctrl Pts',(-0.0358544927611633,0.00353177085984188,
-0.00313195953803351));
#50131=CARTESIAN_POINT('Ctrl Pts',(-0.0358658119065493,0.00352927449325723,
-0.00312806260436819));
#50132=CARTESIAN_POINT('Ctrl Pts',(-0.0358773984533578,0.00352672229526407,
-0.00312407426270795));
#50133=CARTESIAN_POINT('Ctrl Pts',(-0.0358892505658731,0.00352411502968923,
-0.0031199950177777));
#50134=CARTESIAN_POINT('Ctrl Pts',(-0.0360340353943418,0.00349226480058136,
-0.00307016316065143));
#50135=CARTESIAN_POINT('Ctrl Pts',(-0.0362183141856735,0.00345212494100749,
-0.00300676298061814));
#50136=CARTESIAN_POINT('Ctrl Pts',(-0.0364391610694963,0.00340557668880201,
-0.0029308697522048));
#50137=CARTESIAN_POINT('',(-0.0364455123647,0.00340591076454288,0.00292997690155914));
#50138=CARTESIAN_POINT('Ctrl Pts',(-0.0364391610694963,0.00340557668880199,
-0.00293086975220478));
#50139=CARTESIAN_POINT('Ctrl Pts',(-0.0366322171547545,0.00336488594745255,
-0.00286452673010944));
#50140=CARTESIAN_POINT('Ctrl Pts',(-0.0368202498946822,0.00332281518765035,
-0.00279459104114316));
#50141=CARTESIAN_POINT('Ctrl Pts',(-0.0369926649570915,0.00328301199041162,
-0.00272634783401865));
#50142=CARTESIAN_POINT('Ctrl Pts',(-0.0371650800195008,0.00324320879317288,
-0.00265810462689414));
#50143=CARTESIAN_POINT('Ctrl Pts',(-0.0373212896723696,0.00320527811107744,
-0.00259151629192671));
#50144=CARTESIAN_POINT('Ctrl Pts',(-0.0374934455541359,0.00316088800823521,
-0.00250972996224946));
#50145=CARTESIAN_POINT('Ctrl Pts',(-0.0376508819930815,0.0031202932888204,
-0.00243493641835938));
#50146=CARTESIAN_POINT('Ctrl Pts',(-0.0378208106088136,0.00307439159668025,
-0.00234670930103131));
#50147=CARTESIAN_POINT('Ctrl Pts',(-0.0379716858037714,0.00303194552412074,
-0.0022594496374276));
#50148=CARTESIAN_POINT('Ctrl Pts',(-0.037985791806296,0.00302797704933699,
-0.00225129133787787));
#50149=CARTESIAN_POINT('Ctrl Pts',(-0.0379997479104133,0.00302403681227977,
-0.00224314220566623));
#50150=CARTESIAN_POINT('Ctrl Pts',(-0.0380135368744372,0.00302013075314561,
-0.0022350151484838));
#50151=CARTESIAN_POINT('Ctrl Pts',(-0.0381748100482325,0.00297444620769995,
-0.00213996259028189));
#50152=CARTESIAN_POINT('Ctrl Pts',(-0.038312309636301,0.00293311953030676,
-0.00204871414221153));
#50153=CARTESIAN_POINT('Ctrl Pts',(-0.0384600371843599,0.00288577414216096,
-0.00193316908477411));
#50154=CARTESIAN_POINT('Ctrl Pts',(-0.0386051400137966,0.00283926995339588,
-0.00181967695022035));
#50155=CARTESIAN_POINT('Ctrl Pts',(-0.0387586492955602,0.00278795635858161,
-0.00168181136542702));
#50156=CARTESIAN_POINT('Ctrl Pts',(-0.0388855191400815,0.00274380193022642,
-0.00154395937952611));
#50157=CARTESIAN_POINT('Ctrl Pts',(-0.0388878140480774,0.00274300323490941,
-0.00154146581909104));
#50158=CARTESIAN_POINT('Ctrl Pts',(-0.0388901012423995,0.00274220668911971,
-0.0015389723937722));
#50159=CARTESIAN_POINT('Ctrl Pts',(-0.0388923806047438,0.00274141234102353,
-0.00153647927517296));
#50160=CARTESIAN_POINT('Ctrl Pts',(-0.0390206703983249,0.00269670389282599,
-0.00139615859676874));
#50161=CARTESIAN_POINT('Ctrl Pts',(-0.0391239336719105,0.00265838818924466,
-0.00125737015421032));
#50162=CARTESIAN_POINT('Ctrl Pts',(-0.0392167430625687,0.00262253089827314,
-0.00109809991377156));
#50163=CARTESIAN_POINT('Ctrl Pts',(-0.0392749718618309,0.00260003396145177,
-0.000998173443042866));
#50164=CARTESIAN_POINT('Ctrl Pts',(-0.039328684790478,0.00257880129105425,
-0.000889923640323347));
#50165=CARTESIAN_POINT('Ctrl Pts',(-0.0393735992297108,0.00256086087193436,
-0.000777199960031099));
#50166=CARTESIAN_POINT('Ctrl Pts',(-0.0394002727639511,0.00255020651685718,
-0.00071025625557167));
#50167=CARTESIAN_POINT('Ctrl Pts',(-0.0394238946703283,0.00254070596688381,
-0.000641752316417933));
#50168=CARTESIAN_POINT('Ctrl Pts',(-0.0394439206157009,0.00253260235611844,
-0.000572334592845821));
#50169=CARTESIAN_POINT('Ctrl Pts',(-0.0394976674058036,0.00251085341699091,
-0.000386027292550317));
#50170=CARTESIAN_POINT('Ctrl Pts',(-0.0395245481484425,0.00249939378462001,
-0.000193588585587571));
#50171=CARTESIAN_POINT('Ctrl Pts',(-0.0395245044804478,0.00249944756631425,
-5.83969798006665E-7));
#50172=CARTESIAN_POINT('Ctrl Pts',(-0.0395244608124532,0.00249950134800849,
0.000192420645991558));
#50173=CARTESIAN_POINT('Ctrl Pts',(-0.0394974499353326,0.00251105592430073,
0.000385956457755352));
#50174=CARTESIAN_POINT('Ctrl Pts',(-0.0394437750762487,0.00253280713317883,
0.000572917666467489));
#50175=CARTESIAN_POINT('Ctrl Pts',(-0.0394235786421328,0.00254099153951996,
0.000643266239307942));
#50176=CARTESIAN_POINT('Ctrl Pts',(-0.039399665844055,0.0025505954007062,
0.00071267267253678));
#50177=CARTESIAN_POINT('Ctrl Pts',(-0.0393726489689033,0.00256137149458157,
0.000780388259510024));
#50178=CARTESIAN_POINT('Ctrl Pts',(-0.0393278647053818,0.00257923438305918,
0.000892636351656218));
#50179=CARTESIAN_POINT('Ctrl Pts',(-0.0392744071551819,0.0026003385220159,
0.00100020014102538));
#50180=CARTESIAN_POINT('Ctrl Pts',(-0.0392166403478267,0.00262273376753246,
0.00109956726159259));
#50181=CARTESIAN_POINT('Ctrl Pts',(-0.0391240247230632,0.00265863932905144,
0.00125887930208133));
#50182=CARTESIAN_POINT('Ctrl Pts',(-0.0390206909807072,0.00269703396732437,
0.00139746286942015));
#50183=CARTESIAN_POINT('Ctrl Pts',(-0.0388923702372792,0.00274183860381698,
0.00153769715301582));
#50184=CARTESIAN_POINT('Ctrl Pts',(-0.0388899378618459,0.00274268789516454,
0.00154035535477821));
#50185=CARTESIAN_POINT('Ctrl Pts',(-0.0388874965753729,0.0027435396942637,
0.00154301394633622));
#50186=CARTESIAN_POINT('Ctrl Pts',(-0.0388850465184323,0.00274439394252674,
0.00154567272298213));
#50187=CARTESIAN_POINT('Ctrl Pts',(-0.0387582430383768,0.00278860583441763,
0.00168327855809584));
#50188=CARTESIAN_POINT('Ctrl Pts',(-0.0386049180378238,0.00283996495012589,
0.00182099137683305));
#50189=CARTESIAN_POINT('Ctrl Pts',(-0.0384601201429457,0.00288638007257898,
0.00193416251744746));
#50190=CARTESIAN_POINT('Ctrl Pts',(-0.0383125245087059,0.00293369201342276,
0.00204952031522948));
#50191=CARTESIAN_POINT('Ctrl Pts',(-0.038175769856324,0.00297489082212998,
0.00214047070895444));
#50192=CARTESIAN_POINT('Ctrl Pts',(-0.0380152841178011,0.00302046341891065,
0.00223527013525858));
#50193=CARTESIAN_POINT('Ctrl Pts',(-0.0380013638600284,0.00302441630781155,
0.00224349287494253));
#50194=CARTESIAN_POINT('Ctrl Pts',(-0.0379872712832568,0.00302840453802309,
0.00225173873899062));
#50195=CARTESIAN_POINT('Ctrl Pts',(-0.037973024859638,0.00303242184803372,
0.00225999405200227));
#50196=CARTESIAN_POINT('Ctrl Pts',(-0.0378230252000953,0.0030747198415511,
0.00234691370105252));
#50197=CARTESIAN_POINT('Ctrl Pts',(-0.0376540512084115,0.00312046819384517,
0.00243479635430532));
#50198=CARTESIAN_POINT('Ctrl Pts',(-0.0374974436182988,0.00316102158131972,
0.00250941439811513));
#50199=CARTESIAN_POINT('Ctrl Pts',(-0.0373259620072885,0.00320542658245059,
0.00259111939308842));
#50200=CARTESIAN_POINT('Ctrl Pts',(-0.0371698572482878,0.00324337705647934,
0.00265761331386267));
#50201=CARTESIAN_POINT('Ctrl Pts',(-0.0369977736313312,0.00328321943549953,
0.00272576538045062));
#50202=CARTESIAN_POINT('Ctrl Pts',(-0.0368256900143745,0.00332306181451972,
0.00279391744703857));
#50203=CARTESIAN_POINT('Ctrl Pts',(-0.0366381245804503,0.00336517498387712,
0.00286373576666462));
#50204=CARTESIAN_POINT('Ctrl Pts',(-0.0364455123647003,0.00340591076454282,
0.00292997690155905));
#50205=CARTESIAN_POINT('',(-0.0328029016201836,0.0042087665877202,0.00416971706663987));
#50206=CARTESIAN_POINT('Ctrl Pts',(-0.0364455123647,0.00340591076454287,
0.00292997690155913));
#50207=CARTESIAN_POINT('Ctrl Pts',(-0.0362270644193021,0.00345211057323863,
0.00300510318396827));
#50208=CARTESIAN_POINT('Ctrl Pts',(-0.0360444782753564,0.00349201166437273,
0.00306795737029401));
#50209=CARTESIAN_POINT('Ctrl Pts',(-0.035900556669434,0.00352377780582171,
0.00311751449050552));
#50210=CARTESIAN_POINT('Ctrl Pts',(-0.0358866082105257,0.00352685648685669,
0.00312231742089569));
#50211=CARTESIAN_POINT('Ctrl Pts',(-0.0358730242130647,0.00352985940275686,
0.00312699546607101));
#50212=CARTESIAN_POINT('Ctrl Pts',(-0.035859807632643,0.00353278531481164,
0.00313154782206464));
#50213=CARTESIAN_POINT('Ctrl Pts',(-0.0357850143374938,0.0035493431986902,
0.0031573098342184));
#50214=CARTESIAN_POINT('Ctrl Pts',(-0.0357219488060029,0.00356341802743243,
0.00317903667032381));
#50215=CARTESIAN_POINT('Ctrl Pts',(-0.0356653693009525,0.00357608634117101,
0.00319852211497317));
#50216=CARTESIAN_POINT('Ctrl Pts',(-0.0356370795484272,0.0035824204980403,
0.00320826483729785));
#50217=CARTESIAN_POINT('Ctrl Pts',(-0.0356104112237838,0.0035884052174244,
0.00321744556903178));
#50218=CARTESIAN_POINT('Ctrl Pts',(-0.0355924301039697,0.00359244353562749,
0.00322363379433966));
#50219=CARTESIAN_POINT('Ctrl Pts',(-0.0355744489841556,0.00359648185383058,
0.00322982201964753));
#50220=CARTESIAN_POINT('Ctrl Pts',(-0.0355651552515481,0.00359856917227115,
0.00323302126335804));
#50221=CARTESIAN_POINT('Ctrl Pts',(-0.035535592160163,0.0036052117695187,
0.0032431750763029));
#50222=CARTESIAN_POINT('Ctrl Pts',(-0.0355060290687778,0.00361185436676625,
0.00325332888924775));
#50223=CARTESIAN_POINT('Ctrl Pts',(-0.0354562026487998,0.00362306570783562,
0.00327043166439547));
#50224=CARTESIAN_POINT('Ctrl Pts',(-0.0354122937915675,0.00363296676100046,
0.00328548603247098));
#50225=CARTESIAN_POINT('Ctrl Pts',(-0.0353831565381878,0.00363953695009156,
0.00329547588337435));
#50226=CARTESIAN_POINT('Ctrl Pts',(-0.0353566195302761,0.00364552894526491,
0.00330456953780217));
#50227=CARTESIAN_POINT('Ctrl Pts',(-0.0353307849961087,0.00365136731128944,
0.00331341831473545));
#50228=CARTESIAN_POINT('Ctrl Pts',(-0.0353176877594042,0.0036543271657732,
0.00331790434592494));
#50229=CARTESIAN_POINT('Ctrl Pts',(-0.0353047699888091,0.00365724785862674,
0.00332232776947711));
#50230=CARTESIAN_POINT('Ctrl Pts',(-0.035291777825036,0.0036601865624281,
0.00332677547357952));
#50231=CARTESIAN_POINT('Ctrl Pts',(-0.0352145389456363,0.0036776572618796,
0.00335321723391829));
#50232=CARTESIAN_POINT('Ctrl Pts',(-0.0351347725914307,0.00369574357075716,
0.00338047939885123));
#50233=CARTESIAN_POINT('Ctrl Pts',(-0.0350590289584748,0.00371293866348363,
0.00340633288155524));
#50234=CARTESIAN_POINT('Ctrl Pts',(-0.0349417405437824,0.00373956512814698,
0.00344636679440428));
#50235=CARTESIAN_POINT('Ctrl Pts',(-0.034833966823461,0.00376406627577167,
0.00348306531417552));
#50236=CARTESIAN_POINT('Ctrl Pts',(-0.0347236872682142,0.00378908587494196,
0.00352051902312663));
#50237=CARTESIAN_POINT('Ctrl Pts',(-0.0346915320539729,0.003796381067326,
0.00353143974213713));
#50238=CARTESIAN_POINT('Ctrl Pts',(-0.0346591514393833,0.00380372333820802,
0.00354242837528044));
#50239=CARTESIAN_POINT('Ctrl Pts',(-0.0346262097476452,0.00381118597583179,
0.00355359860795237));
#50240=CARTESIAN_POINT('Ctrl Pts',(-0.0344802911966427,0.00384424248298917,
0.00360307828188067));
#50241=CARTESIAN_POINT('Ctrl Pts',(-0.03432383153918,0.00387953556415316,
0.00365594651514581));
#50242=CARTESIAN_POINT('Ctrl Pts',(-0.0341701782162089,0.00391389558342509,
0.00370777216502179));
#50243=CARTESIAN_POINT('Ctrl Pts',(-0.0341342598584151,0.00392192766136619,
0.00371988704935457));
#50244=CARTESIAN_POINT('Ctrl Pts',(-0.0340984902611279,0.00392991018127384,
0.00373194625001173));
#50245=CARTESIAN_POINT('Ctrl Pts',(-0.034062832762441,0.00393785044789938,
0.00374396324604674));
#50246=CARTESIAN_POINT('Ctrl Pts',(-0.0339459528541134,0.00396387744557068,
0.00378335314849828));
#50247=CARTESIAN_POINT('Ctrl Pts',(-0.0338302896252035,0.00398944666719792,
0.00382228737361244));
#50248=CARTESIAN_POINT('Ctrl Pts',(-0.0337142953371807,0.00401485474041696,
0.00386135192035288));
#50249=CARTESIAN_POINT('Ctrl Pts',(-0.0335847662876927,0.00404322754764296,
0.00390497470294179));
#50250=CARTESIAN_POINT('Ctrl Pts',(-0.0334549040645208,0.00407138715560721,
0.00394874177972471));
#50251=CARTESIAN_POINT('Ctrl Pts',(-0.0333248665632899,0.0040992144746389,
0.00399266634821324));
#50252=CARTESIAN_POINT('Ctrl Pts',(-0.0331886125518466,0.00412837209309429,
0.00403869075348735));
#50253=CARTESIAN_POINT('Ctrl Pts',(-0.0330521528209864,0.00415716609479881,
0.00408489535755997));
#50254=CARTESIAN_POINT('Ctrl Pts',(-0.0329158597169497,0.00418544311210461,
0.00413124843967162));
#50255=CARTESIAN_POINT('Ctrl Pts',(-0.0328781890819101,0.00419325871808455,
0.00414406016665905));
#50256=CARTESIAN_POINT('Ctrl Pts',(-0.0328405345546385,0.00420103452583491,
0.00415688169838706));
#50257=CARTESIAN_POINT('Ctrl Pts',(-0.0328029014491621,0.00420876770681893,
0.00416971455610656));
#50258=CARTESIAN_POINT('Ctrl Pts',(-0.0399999989166323,0.00503323066735753,
0.00434914348573771));
#50259=CARTESIAN_POINT('Ctrl Pts',(-0.039711581140538,0.00502913112529287,
0.00434681829103734));
#50260=CARTESIAN_POINT('Ctrl Pts',(-0.0394894177154315,0.00502523749458704,
0.00434631164359477));
#50261=CARTESIAN_POINT('Ctrl Pts',(-0.0393406143928409,0.00502250803880602,
0.00434618840248981));
#50262=CARTESIAN_POINT('Ctrl Pts',(-0.0392662127315455,0.00502114331091552,
0.00434612678193733));
#50263=CARTESIAN_POINT('Ctrl Pts',(-0.0392101513869168,0.00502006695100079,
0.00434616560492587));
#50264=CARTESIAN_POINT('Ctrl Pts',(-0.0391653212214987,0.00501908324652545,
0.00434615465470367));
#50265=CARTESIAN_POINT('Ctrl Pts',(-0.0391429061387897,0.00501859139428778,
0.00434614917959258));
#50266=CARTESIAN_POINT('Ctrl Pts',(-0.0391232988904322,0.00501812092527449,
0.00434613436931875));
#50267=CARTESIAN_POINT('Ctrl Pts',(-0.0391162722622056,0.00501801715431804,
0.00434616679069379));
#50268=CARTESIAN_POINT('Ctrl Pts',(-0.0391127589480922,0.00501796526883981,
0.00434618300138131));
#50269=CARTESIAN_POINT('Ctrl Pts',(-0.0391123907856138,0.00501800519558459,
0.00434621078025896));
#50270=CARTESIAN_POINT('Ctrl Pts',(-0.0391101702857959,0.00501796303220673,
0.00434621586351736));
#50271=CARTESIAN_POINT('Ctrl Pts',(-0.0391079497859779,0.00501792086882887,
0.00434622094677576));
#50272=CARTESIAN_POINT('Ctrl Pts',(-0.0391038769436897,0.00501779685223246,
0.00434620292056547));
#50273=CARTESIAN_POINT('Ctrl Pts',(-0.039092954313039,0.00501741517263418,
0.0043461308499061));
#50274=CARTESIAN_POINT('Ctrl Pts',(-0.0390711090517377,0.00501665181343761,
0.00434598670858736));
#50275=CARTESIAN_POINT('Ctrl Pts',(-0.0390218648173137,0.00501485005279275,
0.0043456399058556));
#50276=CARTESIAN_POINT('Ctrl Pts',(-0.0389797747097396,0.00501320906924717,
0.00434533586273387));
#50277=CARTESIAN_POINT('Ctrl Pts',(-0.0389376846021655,0.0050115680857016,
0.00434503181961215));
#50278=CARTESIAN_POINT('Ctrl Pts',(-0.0389027483307743,0.00501009839743316,
0.00434475226826703));
#50279=CARTESIAN_POINT('Ctrl Pts',(-0.038866578037483,0.00500850610247983,
0.00434444753378693));
#50280=CARTESIAN_POINT('Ctrl Pts',(-0.0387942374509004,0.00500532151257317,
0.00434383806482675));
#50281=CARTESIAN_POINT('Ctrl Pts',(-0.0387169611433133,0.00500163550461192,
0.00434314683154966));
#50282=CARTESIAN_POINT('Ctrl Pts',(-0.0386401339110594,0.00499761879150246,
0.00434239304998539));
#50283=CARTESIAN_POINT('Ctrl Pts',(-0.0384864794465515,0.00498958536528355,
0.00434088548685686));
#50284=CARTESIAN_POINT('Ctrl Pts',(-0.0383346207956242,0.00498023760043779,
0.00433911356543341));
#50285=CARTESIAN_POINT('Ctrl Pts',(-0.0381870450731536,0.00496998227270427,
0.00433717084775423));
#50286=CARTESIAN_POINT('Ctrl Pts',(-0.0380394693506831,0.00495972694497075,
0.00433522813007506));
#50287=CARTESIAN_POINT('Ctrl Pts',(-0.0378961762638081,0.00494857311330899,
0.00433309893900448));
#50288=CARTESIAN_POINT('Ctrl Pts',(-0.0377495136538368,0.00493598755792319,
0.00433066417381591));
#50289=CARTESIAN_POINT('Ctrl Pts',(-0.0376028510438655,0.00492340200253738,
0.00432822940862735));
#50290=CARTESIAN_POINT('Ctrl Pts',(-0.0374528194588452,0.00490937444928368,
0.00432550627190693));
#50291=CARTESIAN_POINT('Ctrl Pts',(-0.0373028914612309,0.00489425572424894,
0.0043225615854874));
#50292=CARTESIAN_POINT('Ctrl Pts',(-0.0371529634636166,0.0048791369992142,
0.00431961689906786));
#50293=CARTESIAN_POINT('Ctrl Pts',(-0.0370031385604832,0.00486293516907937,
0.00431643738830799));
#50294=CARTESIAN_POINT('Ctrl Pts',(-0.0368471831474604,0.00484485748918042,
0.00431280949290434));
#50295=CARTESIAN_POINT('Ctrl Pts',(-0.0366912277344377,0.00482677980928146,
0.0043091815975007));
#50296=CARTESIAN_POINT('Ctrl Pts',(-0.0365291435108589,0.0048068043540339,
0.00430513969283296));
#50297=CARTESIAN_POINT('Ctrl Pts',(-0.0363823923887819,0.00478786232742212,
0.0043012714753759));
#50298=CARTESIAN_POINT('Ctrl Pts',(-0.0362356412667049,0.00476892030081034,
0.00429740325791884));
#50299=CARTESIAN_POINT('Ctrl Pts',(-0.0361042200002657,0.00475104735615687,
0.00429365574570242));
#50300=CARTESIAN_POINT('Ctrl Pts',(-0.0359631726729839,0.0047311683590897,
0.00428942794780173));
#50301=CARTESIAN_POINT('Ctrl Pts',(-0.0358221253457021,0.00471128936202254,
0.00428520014990104));
#50302=CARTESIAN_POINT('Ctrl Pts',(-0.0356714544382095,0.00468938023788155,
0.00428052580056473));
#50303=CARTESIAN_POINT('Ctrl Pts',(-0.0355174660492713,0.00466619058057617,
0.00427549612867958));
#50304=CARTESIAN_POINT('Ctrl Pts',(-0.0354404718548022,0.00465459575192348,
0.004272981292737));
#50305=CARTESIAN_POINT('Ctrl Pts',(-0.035362648125467,0.00464268212391236,
0.00427037596598903));
#50306=CARTESIAN_POINT('Ctrl Pts',(-0.0352846830820956,0.0046305817879156,
0.00426771571664521));
#50307=CARTESIAN_POINT('Ctrl Pts',(-0.0352067180387242,0.00461848145191885,
0.00426505546730138));
#50308=CARTESIAN_POINT('Ctrl Pts',(-0.0351286115346058,0.00460619582423831,
0.00426233832436842));
#50309=CARTESIAN_POINT('Ctrl Pts',(-0.0350452817127376,0.00459288652142108,
0.00425936094303203));
#50310=CARTESIAN_POINT('Ctrl Pts',(-0.0350036168018035,0.00458623187001247,
0.00425787225236383));
#50311=CARTESIAN_POINT('Ctrl Pts',(-0.0349606463711649,0.00457931863118851,
0.00425632189955588));
#50312=CARTESIAN_POINT('Ctrl Pts',(-0.0349380016209598,0.00457566243006404,
0.00425549928983568));
#50313=CARTESIAN_POINT('Ctrl Pts',(-0.0349153568707547,0.00457200622893958,
0.00425467668011547));
#50314=CARTESIAN_POINT('Ctrl Pts',(-0.0349130374120522,0.00457161034223773,
0.00425457772917389));
#50315=CARTESIAN_POINT('Ctrl Pts',(-0.0349053710842191,0.00457033836329817,
0.00425427430389109));
#50316=CARTESIAN_POINT('Ctrl Pts',(-0.0348900384285529,0.00456779440541904,
0.00425366745332548));
#50317=CARTESIAN_POINT('Ctrl Pts',(-0.0348533188437881,0.0045617414677081,
0.00425224845367909));
#50318=CARTESIAN_POINT('Ctrl Pts',(-0.034813518170537,0.00455512497361659,
0.00425068480677904));
#50319=CARTESIAN_POINT('Ctrl Pts',(-0.0347339168240347,0.00454189198543359,
0.00424755751297895));
#50320=CARTESIAN_POINT('Ctrl Pts',(-0.0346419899576794,0.00452641460551389,
0.00424383939069223));
#50321=CARTESIAN_POINT('Ctrl Pts',(-0.0345234582519701,0.00450632423353793,
0.00423905828357747));
#50322=CARTESIAN_POINT('Ctrl Pts',(-0.0344049265462607,0.00448623386156196,
0.0042342771764627));
#50323=CARTESIAN_POINT('Ctrl Pts',(-0.0342597908811681,0.00446152376856126,
0.00422844041257158));
#50324=CARTESIAN_POINT('Ctrl Pts',(-0.0340916301155351,0.00443270371878135,
0.00422171509726581));
#50325=CARTESIAN_POINT('Ctrl Pts',(-0.033755308584269,0.00437506361922152,
0.00420826446665425));
#50326=CARTESIAN_POINT('Ctrl Pts',(-0.0333269077952901,0.00430084306725824,
0.00419133495359302));
#50327=CARTESIAN_POINT('Ctrl Pts',(-0.0328029052223737,0.0042087689636135,
0.00416971896312806));
#50328=CARTESIAN_POINT('Ctrl Pts',(-0.04,0.00997687591821936,-0.00434339564002003));
#50329=CARTESIAN_POINT('Ctrl Pts',(-0.0366885717327396,0.00997687591821936,
-0.00434339564002003));
#50330=CARTESIAN_POINT('Ctrl Pts',(-0.0338250628738108,0.0101232964422964,
-0.00449314468513572));
#50331=CARTESIAN_POINT('Ctrl Pts',(-0.0311299933513177,0.0103662543728445,
-0.00486696278424518));
#50332=CARTESIAN_POINT('Ctrl Pts',(-0.04,0.0107388615197248,-0.00390886377996825));
#50333=CARTESIAN_POINT('Ctrl Pts',(-0.0367159969968672,0.0107388615197248,
-0.00390886377996825));
#50334=CARTESIAN_POINT('Ctrl Pts',(-0.0338649863625956,0.0108410632031505,
-0.00400561616999478));
#50335=CARTESIAN_POINT('Ctrl Pts',(-0.0311724810188551,0.011010647908647,
-0.00427784708467796));
#50336=CARTESIAN_POINT('Ctrl Pts',(-0.04,0.0120285654953516,-0.00263057838182841));
#50337=CARTESIAN_POINT('Ctrl Pts',(-0.0367708476877013,0.0120285654953516,
-0.00263057838182841));
#50338=CARTESIAN_POINT('Ctrl Pts',(-0.0339449440082147,0.0120559242133456,
-0.00266140852833637));
#50339=CARTESIAN_POINT('Ctrl Pts',(-0.0312576750393058,0.0121013205007559,
-0.00278583369248179));
#50340=CARTESIAN_POINT('Ctrl Pts',(-0.04,0.0127366477880115,4.35202123928724E-7));
#50341=CARTESIAN_POINT('Ctrl Pts',(-0.0367665215704158,0.0127366477880115,
4.35202123928724E-7));
#50342=CARTESIAN_POINT('Ctrl Pts',(-0.033936097062896,0.0127229154815913,
2.59498982767992E-6));
#50343=CARTESIAN_POINT('Ctrl Pts',(-0.0312436761854233,0.0127001287639775,
7.2219948256526E-6));
#50344=CARTESIAN_POINT('Ctrl Pts',(-0.04,0.0120281281938075,0.00263133105653345));
#50345=CARTESIAN_POINT('Ctrl Pts',(-0.0367570493854284,0.0120281281938075,
0.00263133105653345));
#50346=CARTESIAN_POINT('Ctrl Pts',(-0.0339195876897249,0.0120555116847181,
0.00266649147709405));
#50347=CARTESIAN_POINT('Ctrl Pts',(-0.0312212323834849,0.0121009494899832,
0.00280018576913209));
#50348=CARTESIAN_POINT('Ctrl Pts',(-0.04,0.0107382117670507,0.00390940207014268));
#50349=CARTESIAN_POINT('Ctrl Pts',(-0.0366933059897235,0.0107382117670507,
0.00390940207014268));
#50350=CARTESIAN_POINT('Ctrl Pts',(-0.0338229608340258,0.0108404502398202,
0.00401050490853467));
#50351=CARTESIAN_POINT('Ctrl Pts',(-0.0311118088133509,0.0110100966150892,
0.00429203315759127));
#50352=CARTESIAN_POINT('Ctrl Pts',(-0.04,0.00997615395078692,0.0043438072715076));
#50353=CARTESIAN_POINT('Ctrl Pts',(-0.036661434210569,0.00997615395078692,
0.0043438072715076));
#50354=CARTESIAN_POINT('Ctrl Pts',(-0.0337745920634133,0.0101226153439546,
0.00449791927069512));
#50355=CARTESIAN_POINT('Ctrl Pts',(-0.0310569876683288,0.010365641789481,
0.00488105194237219));
#50356=CARTESIAN_POINT('',(-0.0347727610542622,0.012000956525018,-0.00227981334747213));
#50357=CARTESIAN_POINT('',(-0.0312271855506422,0.0110770582020895,-0.00409339326150648));
#50358=CARTESIAN_POINT('Ctrl Pts',(-0.0347727610542622,0.012000956525018,
-0.00227981334747212));
#50359=CARTESIAN_POINT('Ctrl Pts',(-0.0347662162249802,0.0119994708798832,
-0.00228333575096989));
#50360=CARTESIAN_POINT('Ctrl Pts',(-0.0346907936442485,0.0119827318232676,
-0.00232385956332954));
#50361=CARTESIAN_POINT('Ctrl Pts',(-0.0345418896085024,0.0119471677082457,
-0.00240444031058215));
#50362=CARTESIAN_POINT('Ctrl Pts',(-0.0344738490314361,0.0119309169538802,
-0.00244126107582215));
#50363=CARTESIAN_POINT('Ctrl Pts',(-0.0343905139349971,0.0119106560343659,
-0.0024864354481445));
#50364=CARTESIAN_POINT('Ctrl Pts',(-0.0342965588584313,0.011887132404934,
-0.00253740875700026));
#50365=CARTESIAN_POINT('Ctrl Pts',(-0.034236301287015,0.0118720456546244,
-0.00257010020818064));
#50366=CARTESIAN_POINT('Ctrl Pts',(-0.0341731823267349,0.0118560350353544,
-0.00260435876863534));
#50367=CARTESIAN_POINT('Ctrl Pts',(-0.0340949388892498,0.0118357864876751,
-0.00264679134155758));
#50368=CARTESIAN_POINT('Ctrl Pts',(-0.0340646226447708,0.0118279409744727,
-0.00266323228914288));
#50369=CARTESIAN_POINT('Ctrl Pts',(-0.0340320390897621,0.0118194510631183,
-0.00268089710286973));
#50370=CARTESIAN_POINT('Ctrl Pts',(-0.0340002251881336,0.0118111051586246,
-0.00269813252557422));
#50371=CARTESIAN_POINT('Ctrl Pts',(-0.033961994181482,0.0118010758219548,
-0.00271884446363681));
#50372=CARTESIAN_POINT('Ctrl Pts',(-0.0339248656177919,0.0117912519918997,
-0.00273893933469951));
#50373=CARTESIAN_POINT('Ctrl Pts',(-0.0338943260618987,0.0117831360576042,
-0.00275544446672193));
#50374=CARTESIAN_POINT('Ctrl Pts',(-0.0338383730389783,0.0117682664550715,
-0.00278568433116486));
#50375=CARTESIAN_POINT('Ctrl Pts',(-0.0338044172619026,0.0117591280377497,
-0.00280401656801114));
#50376=CARTESIAN_POINT('Ctrl Pts',(-0.0337658113104114,0.0117487234303718,
-0.00282481271370906));
#50377=CARTESIAN_POINT('Ctrl Pts',(-0.0337272053589202,0.0117383188229939,
-0.00284560885940698));
#50378=CARTESIAN_POINT('Ctrl Pts',(-0.0336839476070479,0.0117266082277593,
-0.002868845618102));
#50379=CARTESIAN_POINT('Ctrl Pts',(-0.0336427042610508,0.0117153823389272,
-0.00289094862413562));
#50380=CARTESIAN_POINT('Ctrl Pts',(-0.0336265071504343,0.0117109737013934,
-0.00289962892940737));
#50381=CARTESIAN_POINT('Ctrl Pts',(-0.0336106180654591,0.0117066401691773,
-0.00290813652225827));
#50382=CARTESIAN_POINT('Ctrl Pts',(-0.0335949886689743,0.0117023701389523,
-0.00291649748682474));
#50383=CARTESIAN_POINT('Ctrl Pts',(-0.0335310225595433,0.0116848942741027,
-0.00295071623448586));
#50384=CARTESIAN_POINT('Ctrl Pts',(-0.0334714329877785,0.0116684952021746,
-0.00298246811210692));
#50385=CARTESIAN_POINT('Ctrl Pts',(-0.0334126721852774,0.0116522695073128,
-0.00301364109545719));
#50386=CARTESIAN_POINT('Ctrl Pts',(-0.0333395538442574,0.0116320792471445,
-0.00305243084525968));
#50387=CARTESIAN_POINT('Ctrl Pts',(-0.0332677431191887,0.0116121490182614,
-0.00309030074696719));
#50388=CARTESIAN_POINT('Ctrl Pts',(-0.0332040782600887,0.011594446505781,
-0.00312370844975335));
#50389=CARTESIAN_POINT('Ctrl Pts',(-0.0331902389087889,0.0115905983658092,
-0.00313097055543473));
#50390=CARTESIAN_POINT('Ctrl Pts',(-0.0331767719966812,0.0115868537675826,
-0.00313802634461842));
#50391=CARTESIAN_POINT('Ctrl Pts',(-0.0331634772545252,0.011583157686754,
-0.00314498140164933));
#50392=CARTESIAN_POINT('Ctrl Pts',(-0.0331156124908776,0.0115698507693872,
-0.00317002153834643));
#50393=CARTESIAN_POINT('Ctrl Pts',(-0.0330700704267301,0.0115571966523754,
-0.00319372493591726));
#50394=CARTESIAN_POINT('Ctrl Pts',(-0.0330167657676819,0.0115424264317148,
-0.00322127745264625));
#50395=CARTESIAN_POINT('Ctrl Pts',(-0.032948655400974,0.0115235536884403,
-0.00325648285591949));
#50396=CARTESIAN_POINT('Ctrl Pts',(-0.0328679304816266,0.0115012287484612,
-0.00329790419386068));
#50397=CARTESIAN_POINT('Ctrl Pts',(-0.0327909578303375,0.0114800362569381,
-0.00333705744501196));
#50398=CARTESIAN_POINT('Ctrl Pts',(-0.0327573110869359,0.0114707724689254,
-0.00335417234715916));
#50399=CARTESIAN_POINT('Ctrl Pts',(-0.0327243697723556,0.011461725602602,
-0.00337086051058516));
#50400=CARTESIAN_POINT('Ctrl Pts',(-0.0326918474558674,0.0114528169513001,
-0.00338727608029467));
#50401=CARTESIAN_POINT('Ctrl Pts',(-0.0326499694389777,0.0114413455467393,
-0.00340841391977791));
#50402=CARTESIAN_POINT('Ctrl Pts',(-0.0326087884759492,0.0114301038343232,
-0.00342909906358724));
#50403=CARTESIAN_POINT('Ctrl Pts',(-0.0325676120192666,0.0114189070941222,
-0.00344969210741507));
#50404=CARTESIAN_POINT('Ctrl Pts',(-0.0324324977420077,0.0113821666948313,
-0.00351726504733077));
#50405=CARTESIAN_POINT('Ctrl Pts',(-0.032297606118495,0.0113459495619924,
-0.00358378257787548));
#50406=CARTESIAN_POINT('Ctrl Pts',(-0.0321620057256791,0.0113102703660507,
-0.00364974238539242));
#50407=CARTESIAN_POINT('Ctrl Pts',(-0.0321507718423466,0.0113073145049629,
-0.0036552068591074));
#50408=CARTESIAN_POINT('Ctrl Pts',(-0.0321395333106712,0.0113043623100987,
-0.00366066739946016));
#50409=CARTESIAN_POINT('Ctrl Pts',(-0.0321282891655846,0.0113014137098195,
-0.00366612453785849));
#50410=CARTESIAN_POINT('Ctrl Pts',(-0.0320417758799519,0.0112787269607416,
-0.00370811216513983));
#50411=CARTESIAN_POINT('Ctrl Pts',(-0.0319549400458757,0.0112562481925477,
-0.00374990739672547));
#50412=CARTESIAN_POINT('Ctrl Pts',(-0.031867579817233,0.0112339722338532,
-0.00379165633688003));
#50413=CARTESIAN_POINT('Ctrl Pts',(-0.0317617277771904,0.0112069810536747,
-0.00384224240509021));
#50414=CARTESIAN_POINT('Ctrl Pts',(-0.031655096866317,0.011180287153048,
-0.003892766024649));
#50415=CARTESIAN_POINT('Ctrl Pts',(-0.031547327846147,0.0111538702353446,
-0.00394349975127678));
#50416=CARTESIAN_POINT('Ctrl Pts',(-0.0314418503941371,0.0111280150390655,
-0.0039931546911401));
#50417=CARTESIAN_POINT('Ctrl Pts',(-0.0313352791840738,0.0111024246360599,
-0.00404301369035159));
#50418=CARTESIAN_POINT('Ctrl Pts',(-0.0312271883190323,0.0110770591286335,
-0.0040933922183782));
#50419=CARTESIAN_POINT('Ctrl Pts',(-0.0399999969232478,0.00997687592866901,
-0.00434339563406105));
#50420=CARTESIAN_POINT('Ctrl Pts',(-0.0395738517935777,0.00998089464425918,
-0.00434110392960138));
#50421=CARTESIAN_POINT('Ctrl Pts',(-0.0391781870153202,0.00999130333547632,
-0.00433902484280308));
#50422=CARTESIAN_POINT('Ctrl Pts',(-0.0388078014104782,0.010007542172654,
-0.0043362037413784));
#50423=CARTESIAN_POINT('Ctrl Pts',(-0.0386226084475415,0.0100156615982803,
-0.00433479318944348));
#50424=CARTESIAN_POINT('Ctrl Pts',(-0.0384437358201049,0.0100252444432719,
-0.00433320817237369));
#50425=CARTESIAN_POINT('Ctrl Pts',(-0.0382763937035359,0.0100357889612725,
-0.00433138882420424));
#50426=CARTESIAN_POINT('Ctrl Pts',(-0.0381090515869669,0.0100463334792731,
-0.0043295694760348));
#50427=CARTESIAN_POINT('Ctrl Pts',(-0.037953239061578,0.0100578130509366,
-0.00432747007831575));
#50428=CARTESIAN_POINT('Ctrl Pts',(-0.037788101735501,0.010071778232986,
-0.0043247184724149));
#50429=CARTESIAN_POINT('Ctrl Pts',(-0.0374578270833469,0.0100997085970848,
-0.0043192152606132));
#50430=CARTESIAN_POINT('Ctrl Pts',(-0.0370902617756126,0.0101377503212127,
-0.0043113870511226));
#50431=CARTESIAN_POINT('Ctrl Pts',(-0.036719991551943,0.010182450920575,
-0.0043020261361203));
#50432=CARTESIAN_POINT('Ctrl Pts',(-0.0365348564401082,0.0102048012202561,
-0.00429734567861916));
#50433=CARTESIAN_POINT('Ctrl Pts',(-0.0363490431730722,0.0102287930336494,
-0.00429224677147734));
#50434=CARTESIAN_POINT('Ctrl Pts',(-0.0361629038294802,0.0102541382250016,
-0.00428678656364088));
#50435=CARTESIAN_POINT('Ctrl Pts',(-0.0360698341576842,0.0102668108206777,
-0.00428405645972265));
#50436=CARTESIAN_POINT('Ctrl Pts',(-0.0359766828489092,0.0102798199653733,
-0.00428123305530202));
#50437=CARTESIAN_POINT('Ctrl Pts',(-0.0358785913924785,0.0102939117478491,
-0.0042781242773886));
#50438=CARTESIAN_POINT('Ctrl Pts',(-0.0357804999360477,0.010308003530325,
-0.00427501549947518));
#50439=CARTESIAN_POINT('Ctrl Pts',(-0.0356774693366876,0.0103231880445341,
-0.00427163559790304));
#50440=CARTESIAN_POINT('Ctrl Pts',(-0.0355904281524484,0.0103362437577912,
-0.00426871175137701));
#50441=CARTESIAN_POINT('Ctrl Pts',(-0.0355033869682092,0.0103492994710482,
-0.00426578790485099));
#50442=CARTESIAN_POINT('Ctrl Pts',(-0.0354323335052546,0.0103602105430234,
-0.00426329869026004));
#50443=CARTESIAN_POINT('Ctrl Pts',(-0.0353541216407747,0.0103723925303275,
-0.00426049197487973));
#50444=CARTESIAN_POINT('Ctrl Pts',(-0.0352759097762947,0.0103845745176317,
-0.00425768525949942));
#50445=CARTESIAN_POINT('Ctrl Pts',(-0.0351905405864586,0.0103980370683696,
-0.00425457369612543));
#50446=CARTESIAN_POINT('Ctrl Pts',(-0.0351042461552928,0.010411833918664,
-0.00425136745846616));
#50447=CARTESIAN_POINT('Ctrl Pts',(-0.0349316572929612,0.0104394276192529,
-0.00424495498314762));
#50448=CARTESIAN_POINT('Ctrl Pts',(-0.0347553659619536,0.0104683456523605,
-0.00423814780461085));
#50449=CARTESIAN_POINT('Ctrl Pts',(-0.0345637802517622,0.0105004831389811,
-0.0042304709836301));
#50450=CARTESIAN_POINT('Ctrl Pts',(-0.0343721945415708,0.0105326206256018,
-0.00422279416264936));
#50451=CARTESIAN_POINT('Ctrl Pts',(-0.0341653165318991,0.0105679934601369,
-0.00421426474276195));
#50452=CARTESIAN_POINT('Ctrl Pts',(-0.03396901109119,0.0106019602844291,
-0.00420601505060714));
#50453=CARTESIAN_POINT('Ctrl Pts',(-0.0337727056504808,0.0106359271087213,
-0.00419776535845234));
#50454=CARTESIAN_POINT('Ctrl Pts',(-0.0335869704556112,0.0106684707640346,
-0.00418977769754576));
#50455=CARTESIAN_POINT('Ctrl Pts',(-0.0334035706353302,0.0107005985088829,
-0.00418196081844651));
#50456=CARTESIAN_POINT('Ctrl Pts',(-0.0332201708150493,0.0107327262537313,
-0.00417414393934726));
#50457=CARTESIAN_POINT('Ctrl Pts',(-0.033039107416087,0.0107644457777805,
-0.0041665051414215));
#50458=CARTESIAN_POINT('Ctrl Pts',(-0.0328575587521421,0.0107963002655774,
-0.0041587950627355));
#50459=CARTESIAN_POINT('Ctrl Pts',(-0.0326760100881971,0.0108281547533742,
-0.0041510849840495));
#50460=CARTESIAN_POINT('Ctrl Pts',(-0.032493976134264,0.0108601443570704,
-0.00414330399826378));
#50461=CARTESIAN_POINT('Ctrl Pts',(-0.0323160004717604,0.0108915520131664,
-0.0041354509857575));
#50462=CARTESIAN_POINT('Ctrl Pts',(-0.0322270126405086,0.0109072558412144,
-0.00413152447950437));
#50463=CARTESIAN_POINT('Ctrl Pts',(-0.0321390390296874,0.0109228115832411,
-0.00412757802328178));
#50464=CARTESIAN_POINT('Ctrl Pts',(-0.032058751349319,0.0109368485082703,
-0.00412412547505019));
#50465=CARTESIAN_POINT('Ctrl Pts',(-0.0319784636689506,0.0109508854332996,
-0.00412067292681859));
#50466=CARTESIAN_POINT('Ctrl Pts',(-0.0319058625544242,0.0109634080368383,
-0.00411771731119518));
#50467=CARTESIAN_POINT('Ctrl Pts',(-0.0318233652299006,0.0109774606394118,
-0.00411453809373492));
#50468=CARTESIAN_POINT('Ctrl Pts',(-0.0316583705808533,0.0110055658445589,
-0.00410817965881439));
#50469=CARTESIAN_POINT('Ctrl Pts',(-0.0314537906056737,0.0110397887429251,
-0.00410092050257926));
#50470=CARTESIAN_POINT('Ctrl Pts',(-0.0312272002437396,0.0110770530880674,
-0.00409339712395557));
#50471=CARTESIAN_POINT('',(-0.0311805491196909,0.0110755203513828,0.00410667728630412));
#50472=CARTESIAN_POINT('Ctrl Pts',(-0.0311805648084427,0.0110755143676243,
0.00410668200447306));
#50473=CARTESIAN_POINT('Ctrl Pts',(-0.0313371568854333,0.0110497540541028,
0.00411147974496858));
#50474=CARTESIAN_POINT('Ctrl Pts',(-0.0315032409861522,0.0110220279747615,
0.00411696689026756));
#50475=CARTESIAN_POINT('Ctrl Pts',(-0.0316901958519466,0.010990269889629,
0.00412364605205666));
#50476=CARTESIAN_POINT('Ctrl Pts',(-0.031877150717741,0.0109585118044965,
0.00413032521384576));
#50477=CARTESIAN_POINT('Ctrl Pts',(-0.0320849742587853,0.0109227073742163,
0.0041381857078831));
#50478=CARTESIAN_POINT('Ctrl Pts',(-0.03227706278129,0.0108894139580456,
0.00414560009689503));
#50479=CARTESIAN_POINT('Ctrl Pts',(-0.0324691513037948,0.0108561205418749,
0.00415301448590696));
#50480=CARTESIAN_POINT('Ctrl Pts',(-0.0326455063356221,0.0108253481113506,
0.00415998828010131));
#50481=CARTESIAN_POINT('Ctrl Pts',(-0.0328258638881128,0.0107939394614203,
0.00416708628235608));
#50482=CARTESIAN_POINT('Ctrl Pts',(-0.0330062214406034,0.01076253081149,
0.00417418428461086));
#50483=CARTESIAN_POINT('Ctrl Pts',(-0.0331905823077373,0.0107304917967662,
0.00418141299511146));
#50484=CARTESIAN_POINT('Ctrl Pts',(-0.0333738417105198,0.0106983687695328,
0.00418895670506269));
#50485=CARTESIAN_POINT('Ctrl Pts',(-0.0337403605160849,0.0106341227150661,
0.00420404412496513));
#50486=CARTESIAN_POINT('Ctrl Pts',(-0.0341024613721,0.0105694464301792,
0.00422028417680778));
#50487=CARTESIAN_POINT('Ctrl Pts',(-0.0344647676792294,0.0105081464292615,
0.0042345923946209));
#50488=CARTESIAN_POINT('Ctrl Pts',(-0.0348270739863588,0.0104468464283438,
0.00424890061243402));
#50489=CARTESIAN_POINT('Ctrl Pts',(-0.0351895922052,0.0103889807025132,
0.00426136261367898));
#50490=CARTESIAN_POINT('Ctrl Pts',(-0.0355611770151797,0.0103340570263314,
0.00427288930827505));
#50491=CARTESIAN_POINT('Ctrl Pts',(-0.0359327618251594,0.0102791333501495,
0.00428441600287112));
#50492=CARTESIAN_POINT('Ctrl Pts',(-0.0363134177233673,0.0102271929237579,
0.00429506336753169));
#50493=CARTESIAN_POINT('Ctrl Pts',(-0.0366843211943214,0.0101825886185625,
0.00430403705182438));
#50494=CARTESIAN_POINT('Ctrl Pts',(-0.0370552246652755,0.0101379843133672,
0.00431301073611707));
#50495=CARTESIAN_POINT('Ctrl Pts',(-0.0374163694815425,0.0101006527765711,
0.00432021620435609));
#50496=CARTESIAN_POINT('Ctrl Pts',(-0.037785030861159,0.0100697780674643,
0.00432610688485246));
#50497=CARTESIAN_POINT('Ctrl Pts',(-0.0378771962060632,0.0100620593901876,
0.00432757955497655));
#50498=CARTESIAN_POINT('Ctrl Pts',(-0.0379698317952406,0.0100547517233659,
0.0043289821701388));
#50499=CARTESIAN_POINT('Ctrl Pts',(-0.0380529341974252,0.0100486088393398,
0.0043301407721085));
#50500=CARTESIAN_POINT('Ctrl Pts',(-0.0381360365996097,0.0100424659553138,
0.00433129937407819));
#50501=CARTESIAN_POINT('Ctrl Pts',(-0.0382096052190389,0.0100374751681415,
0.00433219261129474));
#50502=CARTESIAN_POINT('Ctrl Pts',(-0.0382877151654865,0.0100326093935622,
0.00433301336685188));
#50503=CARTESIAN_POINT('Ctrl Pts',(-0.0384439350583817,0.0100228778444037,
0.00433465487796617));
#50504=CARTESIAN_POINT('Ctrl Pts',(-0.0386183217531855,0.0100136844537418,
0.00433607137582392));
#50505=CARTESIAN_POINT('Ctrl Pts',(-0.0388006428457909,0.0100058927764429,
0.00433731100066326));
#50506=CARTESIAN_POINT('Ctrl Pts',(-0.0391652846248559,0.00999030943920216,
0.00433979024758051));
#50507=CARTESIAN_POINT('Ctrl Pts',(-0.0395616602579697,0.00998027460548254,
0.00434145834687895));
#50508=CARTESIAN_POINT('Ctrl Pts',(-0.0399999963064522,0.00997615396455589,
0.0043438072636588));
#50509=CARTESIAN_POINT('',(-0.034761114924408,0.0120023525649548,0.00228080342275957));
#50510=CARTESIAN_POINT('Ctrl Pts',(-0.0311805519738734,0.0110755212028574,
0.00410667612600569));
#50511=CARTESIAN_POINT('Ctrl Pts',(-0.0312918893531326,0.0111015040086574,
0.00405492486269926));
#50512=CARTESIAN_POINT('Ctrl Pts',(-0.0314017335980751,0.0111277460894534,
0.00400366400621591));
#50513=CARTESIAN_POINT('Ctrl Pts',(-0.0315104679833535,0.0111542739003986,
0.00395259289717512));
#50514=CARTESIAN_POINT('Ctrl Pts',(-0.0316184123909562,0.0111806089813405,
0.00390189283024682));
#50515=CARTESIAN_POINT('Ctrl Pts',(-0.0317252674010335,0.0112072263396688,
0.00385137641012631));
#50516=CARTESIAN_POINT('Ctrl Pts',(-0.0318313013275745,0.01123412287288,
0.0038008189377741));
#50517=CARTESIAN_POINT('Ctrl Pts',(-0.0319182047370657,0.0112561667650172,
0.00375938298547096));
#50518=CARTESIAN_POINT('Ctrl Pts',(-0.0320045596728881,0.0112783978373286,
0.00371791719079459));
#50519=CARTESIAN_POINT('Ctrl Pts',(-0.0320905660624497,0.0113008209554723,
0.00367628081283267));
#50520=CARTESIAN_POINT('Ctrl Pts',(-0.0321026129250342,0.0113039617479688,
0.00367044883073946));
#50521=CARTESIAN_POINT('Ctrl Pts',(-0.0321146523625482,0.0113071063118642,
0.00366461350737955));
#50522=CARTESIAN_POINT('Ctrl Pts',(-0.0321266856106329,0.0113102547460609,
0.00365877417887169));
#50523=CARTESIAN_POINT('Ctrl Pts',(-0.0322628118099773,0.0113458714289443,
0.00359271673611796));
#50524=CARTESIAN_POINT('Ctrl Pts',(-0.0323981143072709,0.0113819863572385,
0.00352616264000121));
#50525=CARTESIAN_POINT('Ctrl Pts',(-0.0325337400951053,0.0114186401173113,
0.0034585154464424));
#50526=CARTESIAN_POINT('Ctrl Pts',(-0.0325752451621761,0.0114298571343293,
0.0034378136215856));
#50527=CARTESIAN_POINT('Ctrl Pts',(-0.0326167633897675,0.0114411208131778,
0.00341701578897169));
#50528=CARTESIAN_POINT('Ctrl Pts',(-0.0326590147018697,0.0114526223625216,
0.00339574828950089));
#50529=CARTESIAN_POINT('Ctrl Pts',(-0.0326918978185774,0.0114615737245165,
0.00337919633803755));
#50530=CARTESIAN_POINT('Ctrl Pts',(-0.0327252236306174,0.0114706688758631,
0.00336236029861347));
#50531=CARTESIAN_POINT('Ctrl Pts',(-0.032759291126813,0.0114799895158526,
0.00334507974729073));
#50532=CARTESIAN_POINT('Ctrl Pts',(-0.0328371317369472,0.0115012861881837,
0.00330559552307026));
#50533=CARTESIAN_POINT('Ctrl Pts',(-0.0329189086742722,0.0115237573151514,
0.00326375361780902));
#50534=CARTESIAN_POINT('Ctrl Pts',(-0.0329874853269181,0.011542635819523,
0.00322841091201546));
#50535=CARTESIAN_POINT('Ctrl Pts',(-0.0330410365704526,0.0115573779707679,
0.00320081192938659));
#50536=CARTESIAN_POINT('Ctrl Pts',(-0.0330865025860455,0.0115699282316569,
0.0031772185812425));
#50537=CARTESIAN_POINT('Ctrl Pts',(-0.0331343405503289,0.0115831402852154,
0.00315226931100933));
#50538=CARTESIAN_POINT('Ctrl Pts',(-0.0331477629274199,0.0115868473234991,
0.00314526904420802));
#50539=CARTESIAN_POINT('Ctrl Pts',(-0.0331613648801142,0.0115906045911974,
0.00313816443928055));
#50540=CARTESIAN_POINT('Ctrl Pts',(-0.0331753611862401,0.0115944707197936,
0.00313084263796009));
#50541=CARTESIAN_POINT('Ctrl Pts',(-0.0332392409659126,0.0116121159070799,
0.00309742560271175));
#50542=CARTESIAN_POINT('Ctrl Pts',(-0.0333116000603191,0.0116320643618833,
0.00305938956895168));
#50543=CARTESIAN_POINT('Ctrl Pts',(-0.0333856189510863,0.011652363846843,
0.003020250876743));
#50544=CARTESIAN_POINT('Ctrl Pts',(-0.0334451841017341,0.0116686994318155,
0.00298875483467318));
#50545=CARTESIAN_POINT('Ctrl Pts',(-0.0335058104640706,0.0116852674860886,
0.00295655835990366));
#50546=CARTESIAN_POINT('Ctrl Pts',(-0.0335705269574241,0.0117028231560492,
0.00292205539953335));
#50547=CARTESIAN_POINT('Ctrl Pts',(-0.0335862306930179,0.011707083114909,
0.0029136831077298));
#50548=CARTESIAN_POINT('Ctrl Pts',(-0.0336021740916453,0.011711400593777,
0.00290517547569836));
#50549=CARTESIAN_POINT('Ctrl Pts',(-0.0336183971299517,0.0117157849409566,
0.00289651104597295));
#50550=CARTESIAN_POINT('Ctrl Pts',(-0.0336599369421521,0.0117270112572004,
0.00287432538772449));
#50551=CARTESIAN_POINT('Ctrl Pts',(-0.0337033263306569,0.0117386749950227,
0.00285109918914621));
#50552=CARTESIAN_POINT('Ctrl Pts',(-0.0337432769783829,0.0117493627271154,
0.00282965588400019));
#50553=CARTESIAN_POINT('Ctrl Pts',(-0.033783227626109,0.0117600504592081,
0.00280821257885418));
#50554=CARTESIAN_POINT('Ctrl Pts',(-0.0338197408500964,0.0117697936031173,
0.002788570552052));
#50555=CARTESIAN_POINT('Ctrl Pts',(-0.0338738318307421,0.0117840620682984,
0.00275943958532525));
#50556=CARTESIAN_POINT('Ctrl Pts',(-0.0339053976158736,0.0117923886931939,
0.00274243967470438));
#50557=CARTESIAN_POINT('Ctrl Pts',(-0.0339429792784883,0.0118022560787779,
0.00272217110902682));
#50558=CARTESIAN_POINT('Ctrl Pts',(-0.0339811690594926,0.0118121985860684,
0.00270155561106871));
#50559=CARTESIAN_POINT('Ctrl Pts',(-0.0340084211072455,0.0118192935124163,
0.00268684448887767));
#50560=CARTESIAN_POINT('Ctrl Pts',(-0.0340359888280535,0.0118264291801899,
0.00267195442002909));
#50561=CARTESIAN_POINT('Ctrl Pts',(-0.0340619844400523,0.0118331194661837,
0.00265790946211028));
#50562=CARTESIAN_POINT('Ctrl Pts',(-0.0341587801244567,0.0118580310093955,
0.00260561250852268));
#50563=CARTESIAN_POINT('Ctrl Pts',(-0.0342355350435881,0.011877303956768,
0.00256410000912341));
#50564=CARTESIAN_POINT('Ctrl Pts',(-0.0343090494548926,0.0118954720904133,
0.00252436942052295));
#50565=CARTESIAN_POINT('Ctrl Pts',(-0.034377765982074,0.0119124544892019,
0.00248723183044974));
#50566=CARTESIAN_POINT('Ctrl Pts',(-0.034440217823129,0.0119275695818341,
0.00245350394200026));
#50567=CARTESIAN_POINT('Ctrl Pts',(-0.0344945167249313,0.0119405224469314,
0.00242421468177289));
#50568=CARTESIAN_POINT('Ctrl Pts',(-0.0346443687635191,0.0119762692700891,
0.00234338329829906));
#50569=CARTESIAN_POINT('Ctrl Pts',(-0.0347320363953884,0.0119958065028771,
0.00229639230335554));
#50570=CARTESIAN_POINT('Ctrl Pts',(-0.034761114924408,0.0120023525649548,
0.00228080342275955));
#50571=CARTESIAN_POINT('Ctrl Pts',(-0.0347611149244081,0.0120023525649548,
0.00228080342275953));
#50572=CARTESIAN_POINT('Ctrl Pts',(-0.0350057465916318,0.0120574232361325,
0.00214965738323656));
#50573=CARTESIAN_POINT('Ctrl Pts',(-0.0352219305060277,0.0121119430756711,
0.00201136019321215));
#50574=CARTESIAN_POINT('Ctrl Pts',(-0.0354113877997593,0.0121652746629532,
0.00186094727113069));
#50575=CARTESIAN_POINT('Ctrl Pts',(-0.035506116446625,0.0121919404565942,
0.00178574081008997));
#50576=CARTESIAN_POINT('Ctrl Pts',(-0.0355941613778847,0.0122182229392589,
0.00170746180636983));
#50577=CARTESIAN_POINT('Ctrl Pts',(-0.0356727119988853,0.0122425351472171,
0.00163017986048025));
#50578=CARTESIAN_POINT('Ctrl Pts',(-0.035751262619886,0.0122668473551753,
0.00155289791459067));
#50579=CARTESIAN_POINT('Ctrl Pts',(-0.0358203219212352,0.0122894914949874,
0.00147671829736536));
#50580=CARTESIAN_POINT('Ctrl Pts',(-0.0358906376015656,0.0123143053868271,
0.00138469040033681));
#50581=CARTESIAN_POINT('Ctrl Pts',(-0.0359459581526986,0.0123338276067057,
0.00131228785855225));
#50582=CARTESIAN_POINT('Ctrl Pts',(-0.0360023350087833,0.0123544331983604,
0.0012299870285152));
#50583=CARTESIAN_POINT('Ctrl Pts',(-0.0360519439610623,0.0123733252959181,
0.00114522311741257));
#50584=CARTESIAN_POINT('Ctrl Pts',(-0.0360653909104063,0.0123784461675993,
0.00112224710267254));
#50585=CARTESIAN_POINT('Ctrl Pts',(-0.0360783784191254,0.0123834476159398,
0.00109909132918738));
#50586=CARTESIAN_POINT('Ctrl Pts',(-0.0360908073487765,0.0123882936272754,
0.00107590835554495));
#50587=CARTESIAN_POINT('Ctrl Pts',(-0.0361490895171189,0.0124110177118409,
0.000967197950833359));
#50588=CARTESIAN_POINT('Ctrl Pts',(-0.0361957250440342,0.012430415454159,
0.000858097457749819));
#50589=CARTESIAN_POINT('Ctrl Pts',(-0.0362335563872392,0.0124469446125988,
0.000743163630492097));
#50590=CARTESIAN_POINT('Ctrl Pts',(-0.0362517959565832,0.0124549137912221,
0.000687750754959665));
#50591=CARTESIAN_POINT('Ctrl Pts',(-0.0362680632461128,0.0124621879064148,
0.000630954362927607));
#50592=CARTESIAN_POINT('Ctrl Pts',(-0.0362821925945658,0.0124686133356257,
0.00057313845736941));
#50593=CARTESIAN_POINT('Ctrl Pts',(-0.0363266756201778,0.0124888423315418,
0.000391118287346746));
#50594=CARTESIAN_POINT('Ctrl Pts',(-0.036349052138052,0.0125003225965748,
0.000198997572025257));
#50595=CARTESIAN_POINT('Ctrl Pts',(-0.0363499678593351,0.0125005306980164,
7.1125461161381E-6));
#50596=CARTESIAN_POINT('Ctrl Pts',(-0.0363509068618171,0.0125007440902066,
-0.000189650943952258));
#50597=CARTESIAN_POINT('Ctrl Pts',(-0.0363293598144398,0.0124891685314849,
-0.000386265257023896));
#50598=CARTESIAN_POINT('Ctrl Pts',(-0.03628465461844,0.0124684484641288,
-0.000572491284554948));
#50599=CARTESIAN_POINT('Ctrl Pts',(-0.0362719151674783,0.0124625439540131,
-0.00062555932938664));
#50600=CARTESIAN_POINT('Ctrl Pts',(-0.0362573645944939,0.0124559208607803,
-0.000677787987754251));
#50601=CARTESIAN_POINT('Ctrl Pts',(-0.0362410960019726,0.0124486802760739,
-0.000728972235372414));
#50602=CARTESIAN_POINT('Ctrl Pts',(-0.0362044168877487,0.0124323556780397,
-0.00084437206866398));
#50603=CARTESIAN_POINT('Ctrl Pts',(-0.036158683752071,0.0124130217471169,
-0.000954369431566533));
#50604=CARTESIAN_POINT('Ctrl Pts',(-0.0361014308319117,0.0123903467940526,
-0.00106374449995132));
#50605=CARTESIAN_POINT('Ctrl Pts',(-0.0360874771524456,0.012384820455377,
-0.00109040138734813));
#50606=CARTESIAN_POINT('Ctrl Pts',(-0.0360727920550754,0.0123790911585592,
-0.00111700811362443));
#50607=CARTESIAN_POINT('Ctrl Pts',(-0.0360575232042416,0.0123732120918076,
-0.00114334700138639));
#50608=CARTESIAN_POINT('Ctrl Pts',(-0.0360101428950575,0.0123549689375955,
-0.00122507840732604));
#50609=CARTESIAN_POINT('Ctrl Pts',(-0.0359567194207932,0.0123352136600716,
-0.00130421953635196));
#50610=CARTESIAN_POINT('Ctrl Pts',(-0.03590398794558,0.0123163797963791,
-0.00137439251461595));
#50611=CARTESIAN_POINT('Ctrl Pts',(-0.035834263144592,0.0122914765029953,
-0.00146717954407812));
#50612=CARTESIAN_POINT('Ctrl Pts',(-0.0357652787954704,0.0122685831489911,
-0.00154443052208826));
#50613=CARTESIAN_POINT('Ctrl Pts',(-0.0356867706045274,0.0122440124521361,
-0.0016226400606878));
#50614=CARTESIAN_POINT('Ctrl Pts',(-0.0356082624135844,0.0122194417552811,
-0.00170084959928734));
#50615=CARTESIAN_POINT('Ctrl Pts',(-0.0355202275951528,0.012192895300252,
-0.00177991418021254));
#50616=CARTESIAN_POINT('Ctrl Pts',(-0.0354253661890923,0.0121659334521712,
-0.00185587673631822));
#50617=CARTESIAN_POINT('Ctrl Pts',(-0.0352356433769715,0.0121120097560096,
-0.00200780184852956));
#50618=CARTESIAN_POINT('Ctrl Pts',(-0.0350186221148744,0.0120567658180567,
-0.00214749180977129));
#50619=CARTESIAN_POINT('Ctrl Pts',(-0.0347727610542622,0.012000956525018,
-0.00227981334747214));
#50620=CARTESIAN_POINT('Ctrl Pts',(-0.04,0.00410701437367704,-0.00382361007903213));
#50621=CARTESIAN_POINT('Ctrl Pts',(-0.0301131479141235,0.00410701437367704,
-0.00382361007903213));
#50622=CARTESIAN_POINT('Ctrl Pts',(-0.0242064812039311,0.00227260406699975,
-0.00565754282198516));
#50623=CARTESIAN_POINT('Ctrl Pts',(-0.0150880182599324,0.00043817569586083,
-0.0102482507131694));
#50624=CARTESIAN_POINT('Ctrl Pts',(-0.04,0.00441551938950954,-0.00399865527756543));
#50625=CARTESIAN_POINT('Ctrl Pts',(-0.03014220946428,0.00441551938950954,
-0.00399865527756543));
#50626=CARTESIAN_POINT('Ctrl Pts',(-0.0242279866368223,0.00277049415159215,
-0.00567110613607142));
#50627=CARTESIAN_POINT('Ctrl Pts',(-0.0151029086749286,0.00112545046390722,
-0.0102394484928933));
#50628=CARTESIAN_POINT('Ctrl Pts',(-0.04,0.00472402440534204,-0.00417370047609873));
#50629=CARTESIAN_POINT('Ctrl Pts',(-0.0301712710144365,0.00472402440534204,
-0.00417370047609873));
#50630=CARTESIAN_POINT('Ctrl Pts',(-0.0242494920697135,0.00326838423618455,
-0.00568466945015768));
#50631=CARTESIAN_POINT('Ctrl Pts',(-0.0151177990899248,0.00181272523195361,
-0.0102306462726171));
#50632=CARTESIAN_POINT('Ctrl Pts',(-0.04,0.00503252942117453,-0.00434874567463202));
#50633=CARTESIAN_POINT('Ctrl Pts',(-0.030200332564593,0.00503252942117453,
-0.00434874567463202));
#50634=CARTESIAN_POINT('Ctrl Pts',(-0.0242709975026047,0.00376627432077694,
-0.00569823276424395));
#50635=CARTESIAN_POINT('Ctrl Pts',(-0.015132689504921,0.0025,-0.0102218440523409));
#50636=CARTESIAN_POINT('Ctrl Pts',(-0.04,0.00521956265744013,-0.00445486800099385));
#50637=CARTESIAN_POINT('Ctrl Pts',(-0.0302179513244113,0.00521956265744013,
-0.00445486800099385));
#50638=CARTESIAN_POINT('Ctrl Pts',(-0.0242840353156208,0.00406812352596598,
-0.00570645561443391));
#50639=CARTESIAN_POINT('Ctrl Pts',(-0.0151417169189439,0.00291666494051817,
-0.0102165076472256));
#50640=CARTESIAN_POINT('Ctrl Pts',(-0.04,0.00560724895560903,-0.00464290068538419));
#50641=CARTESIAN_POINT('Ctrl Pts',(-0.0302531888727876,0.00560724895560903,
-0.00464290068538419));
#50642=CARTESIAN_POINT('Ctrl Pts',(-0.0243101706144599,0.00467874072064833,
-0.00571926407880603));
#50643=CARTESIAN_POINT('Ctrl Pts',(-0.0151597764656002,0.00375021261144434,
-0.0102058320476674));
#50644=CARTESIAN_POINT('Ctrl Pts',(-0.04,0.00622010312641127,-0.00484777123182973));
#50645=CARTESIAN_POINT('Ctrl Pts',(-0.030289515056412,0.00622010312641127,
-0.00484777123182973));
#50646=CARTESIAN_POINT('Ctrl Pts',(-0.0243413031901115,0.00561041051155431,
-0.00572840549436799));
#50647=CARTESIAN_POINT('Ctrl Pts',(-0.0151868693264875,0.00500069755002587,
-0.0101898165551843));
#50648=CARTESIAN_POINT('Ctrl Pts',(-0.04,0.00685442072891309,-0.00497216498332829));
#50649=CARTESIAN_POINT('Ctrl Pts',(-0.0303161560626962,0.00685442072891309,
-0.00497216498332829));
#50650=CARTESIAN_POINT('Ctrl Pts',(-0.0243678035878454,0.00655264832435518,
-0.00572893819065769));
#50651=CARTESIAN_POINT('Ctrl Pts',(-0.0152139550980222,0.00625085527589332,
-0.0101738052534537));
#50652=CARTESIAN_POINT('Ctrl Pts',(-0.04,0.00728473228062269,-0.005));
#50653=CARTESIAN_POINT('Ctrl Pts',(-0.0303257372905531,0.00728471479311311,
-0.005));
#50654=CARTESIAN_POINT('Ctrl Pts',(-0.0243815314752158,0.00718424112369502,
-0.005724907257076));
#50655=CARTESIAN_POINT('Ctrl Pts',(-0.015232000484084,0.00708374935728818,
-0.0101631380246945));
#50656=CARTESIAN_POINT('Ctrl Pts',(-0.04,0.00749999999999979,-0.005));
#50657=CARTESIAN_POINT('Ctrl Pts',(-0.0303290418474347,0.0075,-0.005));
#50658=CARTESIAN_POINT('Ctrl Pts',(-0.0243876928299813,0.0075,-0.00572224175535161));
#50659=CARTESIAN_POINT('Ctrl Pts',(-0.0152410184731965,0.00749997928621807,
-0.0101578071909577));
#50660=CARTESIAN_POINT('',(-0.0153166288848674,0.00749997934066271,-0.0101211250654636));
#50661=CARTESIAN_POINT('',(-0.0152002984431706,0.00249860370283979,-0.0101883828166932));
#50662=CARTESIAN_POINT('Ctrl Pts',(-0.015200302987251,0.00249860372052335,
-0.010188391982339));
#50663=CARTESIAN_POINT('Ctrl Pts',(-0.0152383462555177,0.00403177811962914,
-0.0101665731553613));
#50664=CARTESIAN_POINT('Ctrl Pts',(-0.0152771294947074,0.00569890335868286,
-0.010144166971735));
#50665=CARTESIAN_POINT('Ctrl Pts',(-0.0153166288848674,0.00749997934066271,
-0.0101211250654636));
#50666=CARTESIAN_POINT('',(-0.0151728897383989,0.00139471190135993,-0.0102040357394328));
#50667=CARTESIAN_POINT('',(-0.0151728647969064,0.0013947315415857,-0.0102039854802522));
#50668=CARTESIAN_POINT('',(-0.0264247148113527,0.00412797976408685,-0.00580905681399726));
#50669=CARTESIAN_POINT('Ctrl Pts',(-0.015172889738406,0.00139471190135982,
-0.0102040357394293));
#50670=CARTESIAN_POINT('Ctrl Pts',(-0.0153640466907317,0.00139164697469342,
-0.0101088087777892));
#50671=CARTESIAN_POINT('Ctrl Pts',(-0.0155523144542564,0.00138937495703902,
-0.010015498686153));
#50672=CARTESIAN_POINT('Ctrl Pts',(-0.0157270793130222,0.00138796132752518,
-0.00992929088300855));
#50673=CARTESIAN_POINT('Ctrl Pts',(-0.0158387317023676,0.00138705819909317,
-0.00987421512424748));
#50674=CARTESIAN_POINT('Ctrl Pts',(-0.0159421944236299,0.00138650141184947,
-0.00982334442246595));
#50675=CARTESIAN_POINT('Ctrl Pts',(-0.016044808187784,0.00138620424068754,
-0.00977303537098498));
#50676=CARTESIAN_POINT('Ctrl Pts',(-0.0161409303235507,0.00138592586938902,
-0.00972590900819523));
#50677=CARTESIAN_POINT('Ctrl Pts',(-0.016241951248696,0.00138584744702312,
-0.0096765029580068));
#50678=CARTESIAN_POINT('Ctrl Pts',(-0.0163580264003874,0.00138615564543367,
-0.00961995244320662));
#50679=CARTESIAN_POINT('Ctrl Pts',(-0.0164981544591239,0.00138652770822528,
-0.00955168362129225));
#50680=CARTESIAN_POINT('Ctrl Pts',(-0.0166503211155925,0.001387535621787,
-0.0094778791870578));
#50681=CARTESIAN_POINT('Ctrl Pts',(-0.0167914691573054,0.00138908714879256,
-0.00940974092434808));
#50682=CARTESIAN_POINT('Ctrl Pts',(-0.0169946940172579,0.00139132103638031,
-0.00931163549738969));
#50683=CARTESIAN_POINT('Ctrl Pts',(-0.0171844689503031,0.00139465213309412,
-0.00922066972026411));
#50684=CARTESIAN_POINT('Ctrl Pts',(-0.0173610695246576,0.001398705432113,
-0.00913648779519181));
#50685=CARTESIAN_POINT('Ctrl Pts',(-0.017480860043453,0.0014014548387561,
-0.00907938607559399));
#50686=CARTESIAN_POINT('Ctrl Pts',(-0.0175941508771455,0.00140451717652119,
-0.00902560988865672));
#50687=CARTESIAN_POINT('Ctrl Pts',(-0.0177050956254356,0.00140798029570822,
-0.00897315003992925));
#50688=CARTESIAN_POINT('Ctrl Pts',(-0.017772581403461,0.00141008685141575,
-0.00894123961820105));
#50689=CARTESIAN_POINT('Ctrl Pts',(-0.0178405165978862,0.00141240430644739,
-0.00890920270627398));
#50690=CARTESIAN_POINT('Ctrl Pts',(-0.0178988704357995,0.00141453537558346,
-0.00888174239928231));
#50691=CARTESIAN_POINT('Ctrl Pts',(-0.0179464182169222,0.00141627180993745,
-0.00885936723574392));
#50692=CARTESIAN_POINT('Ctrl Pts',(-0.0179891513800797,0.00141789221730591,
-0.00883928301160839));
#50693=CARTESIAN_POINT('Ctrl Pts',(-0.0180512194881658,0.00142043815040328,
-0.0088101886104058));
#50694=CARTESIAN_POINT('Ctrl Pts',(-0.0181250746488341,0.00142346756927483,
-0.00877556903295086));
#50695=CARTESIAN_POINT('Ctrl Pts',(-0.0182194266673454,0.00142766991273628,
-0.00873147419872672));
#50696=CARTESIAN_POINT('Ctrl Pts',(-0.0183003383205456,0.00143163411086214,
-0.00869379760743843));
#50697=CARTESIAN_POINT('Ctrl Pts',(-0.0184171707451642,0.00143735821685176,
-0.00863939447343388));
#50698=CARTESIAN_POINT('Ctrl Pts',(-0.0185254060865838,0.00144331181171606,
-0.00858924034070737));
#50699=CARTESIAN_POINT('Ctrl Pts',(-0.0186347757749826,0.00144997327833353,
-0.00853878889151528));
#50700=CARTESIAN_POINT('Ctrl Pts',(-0.018693175629497,0.0014535302847309,
-0.00851184945942952));
#50701=CARTESIAN_POINT('Ctrl Pts',(-0.0187510592544907,0.0014572490992189,
-0.00848521670979728));
#50702=CARTESIAN_POINT('Ctrl Pts',(-0.0188082658532537,0.00146111809363485,
-0.00845896220693822));
#50703=CARTESIAN_POINT('Ctrl Pts',(-0.0189299079947893,0.00146934499012099,
-0.00840313553620804));
#50704=CARTESIAN_POINT('Ctrl Pts',(-0.0190484922899703,0.00147829167063493,
-0.00834903053934462));
#50705=CARTESIAN_POINT('Ctrl Pts',(-0.0191557127031988,0.00148709445690661,
-0.00830034702239981));
#50706=CARTESIAN_POINT('Ctrl Pts',(-0.0192629331164272,0.00149589724317828,
-0.00825166350545499));
#50707=CARTESIAN_POINT('Ctrl Pts',(-0.0193587928518425,0.00150422786878183,
-0.00820832664749509));
#50708=CARTESIAN_POINT('Ctrl Pts',(-0.019478661225813,0.00151594892376546,
-0.00815447593113739));
#50709=CARTESIAN_POINT('Ctrl Pts',(-0.0195350531068573,0.00152146307496695,
-0.00812914194945058));
#50710=CARTESIAN_POINT('Ctrl Pts',(-0.0195967582311657,0.00152771365395053,
-0.00810149537074743));
#50711=CARTESIAN_POINT('Ctrl Pts',(-0.0196600682347633,0.00153443781289968,
-0.00807322828599476));
#50712=CARTESIAN_POINT('Ctrl Pts',(-0.0197313319862307,0.00154200673984564,
-0.00804140995732551));
#50713=CARTESIAN_POINT('Ctrl Pts',(-0.0198046286135981,0.00155018308598661,
-0.00800880776207714));
#50714=CARTESIAN_POINT('Ctrl Pts',(-0.0198746319117117,0.00155840063442004,
-0.00797779417403623));
#50715=CARTESIAN_POINT('Ctrl Pts',(-0.020040699008046,0.00157789492174793,
-0.00790422140458601));
#50716=CARTESIAN_POINT('Ctrl Pts',(-0.020189696337606,0.00159751834165863,
-0.00783885656312635));
#50717=CARTESIAN_POINT('Ctrl Pts',(-0.0203399517608801,0.00161942796698918,
-0.00777356369181081));
#50718=CARTESIAN_POINT('Ctrl Pts',(-0.0204627449085639,0.00163733315670072,
-0.00772020443851101));
#50719=CARTESIAN_POINT('Ctrl Pts',(-0.0205803987442986,0.00165603419083452,
-0.00766953351201657));
#50720=CARTESIAN_POINT('Ctrl Pts',(-0.0206899501216064,0.00167476087238793,
-0.00762273306682818));
#50721=CARTESIAN_POINT('Ctrl Pts',(-0.0207880478009765,0.00169152966204479,
-0.00758082565151955));
#50722=CARTESIAN_POINT('Ctrl Pts',(-0.0208861318571135,0.0017092486297667,
-0.00753920099683491));
#50723=CARTESIAN_POINT('Ctrl Pts',(-0.0210010048825742,0.0017317941529701,
-0.00749096649832249));
#50724=CARTESIAN_POINT('Ctrl Pts',(-0.02113621012128,0.00175833017249457,
-0.00743419462469013));
#50725=CARTESIAN_POINT('Ctrl Pts',(-0.0212846632902717,0.00179016196917818,
-0.00737263337366511));
#50726=CARTESIAN_POINT('Ctrl Pts',(-0.021419463383592,0.00182188843346957,
-0.00731753419372364));
#50727=CARTESIAN_POINT('Ctrl Pts',(-0.0215086395923106,0.00184287688927745,
-0.00728108365537715));
#50728=CARTESIAN_POINT('Ctrl Pts',(-0.0215942891562261,0.00186422684960349,
-0.00724641235429145));
#50729=CARTESIAN_POINT('Ctrl Pts',(-0.0216779850746412,0.00188622057174032,
-0.00721285036718868));
#50730=CARTESIAN_POINT('Ctrl Pts',(-0.021765752732351,0.00190928427081698,
-0.00717765561633489));
#50731=CARTESIAN_POINT('Ctrl Pts',(-0.0218514083708002,0.00193287245044484,
-0.00714365232694369));
#50732=CARTESIAN_POINT('Ctrl Pts',(-0.0219362391982793,0.00195743414150113,
-0.00711033167457065));
#50733=CARTESIAN_POINT('Ctrl Pts',(-0.0220774356881042,0.00199831579578145,
-0.00705487118581248));
#50734=CARTESIAN_POINT('Ctrl Pts',(-0.0222163758277559,0.00204183958808548,
-0.007001269044706));
#50735=CARTESIAN_POINT('Ctrl Pts',(-0.0223589628768257,0.00209034777808599,
-0.00694744377558152));
#50736=CARTESIAN_POINT('Ctrl Pts',(-0.0225872162011364,0.00216799968052833,
-0.00686128029376652));
#50737=CARTESIAN_POINT('Ctrl Pts',(-0.0228248207747851,0.00225873667442951,
-0.00677476643823198));
#50738=CARTESIAN_POINT('Ctrl Pts',(-0.0230511297423702,0.00235518715086805,
-0.0066960403563144));
#50739=CARTESIAN_POINT('Ctrl Pts',(-0.0231077069842665,0.00237929976997769,
-0.006676358835835));
#50740=CARTESIAN_POINT('Ctrl Pts',(-0.0231635748117954,0.00240377040747212,
-0.00665715528197924));
#50741=CARTESIAN_POINT('Ctrl Pts',(-0.023219476345564,0.0024289001944486,
-0.00663817707029671));
#50742=CARTESIAN_POINT('Ctrl Pts',(-0.0232753778793326,0.00245402998142509,
-0.00661919885861419));
#50743=CARTESIAN_POINT('Ctrl Pts',(-0.0233313130972234,0.0024798189490564,
-0.00660044587602993));
#50744=CARTESIAN_POINT('Ctrl Pts',(-0.0233880311148421,0.00250656652116927,
-0.00658168097578289));
#50745=CARTESIAN_POINT('Ctrl Pts',(-0.0235014671500793,0.00256006166539502,
-0.00654415117528881));
#50746=CARTESIAN_POINT('Ctrl Pts',(-0.0236180513149816,0.00261738621136591,
-0.00650661794344506));
#50747=CARTESIAN_POINT('Ctrl Pts',(-0.0237278917023892,0.00267334490073194,
-0.00647224236002402));
#50748=CARTESIAN_POINT('Ctrl Pts',(-0.0238338075057732,0.00272730419275926,
-0.00643909501212436));
#50749=CARTESIAN_POINT('Ctrl Pts',(-0.0239334197217683,0.00278000891741973,
-0.00640881009814871));
#50750=CARTESIAN_POINT('Ctrl Pts',(-0.0240375209246323,0.00283607172543691,
-0.00637800229702447));
#50751=CARTESIAN_POINT('Ctrl Pts',(-0.0240413782707934,0.00283814906605682,
-0.00637686075062412));
#50752=CARTESIAN_POINT('Ctrl Pts',(-0.0240452417268192,0.00284023114535695,
-0.00637571858570592));
#50753=CARTESIAN_POINT('Ctrl Pts',(-0.0240491118410187,0.00284231820402006,
-0.00637457564477758));
#50754=CARTESIAN_POINT('Ctrl Pts',(-0.0241032697900432,0.00287152427155755,
-0.0063585814561453));
#50755=CARTESIAN_POINT('Ctrl Pts',(-0.0241587067718473,0.00290175501435321,
-0.00634244114415675));
#50756=CARTESIAN_POINT('Ctrl Pts',(-0.0242188370468896,0.00293500164702928,
-0.00632525504927828));
#50757=CARTESIAN_POINT('Ctrl Pts',(-0.0242822586570924,0.00297006809195497,
-0.00630712824361301));
#50758=CARTESIAN_POINT('Ctrl Pts',(-0.0243507542959291,0.00300850547177018,
-0.00628796647954365));
#50759=CARTESIAN_POINT('Ctrl Pts',(-0.0244026806904869,0.00303785624166982,
-0.00627365709734696));
#50760=CARTESIAN_POINT('Ctrl Pts',(-0.0244609125934436,0.00307077112434273,
-0.00625761010308629));
#50761=CARTESIAN_POINT('Ctrl Pts',(-0.0245027620972734,0.00309461595014579,
-0.00624626073921518));
#50762=CARTESIAN_POINT('Ctrl Pts',(-0.0245606802234146,0.00312774433649193,
-0.00623079155141568));
#50763=CARTESIAN_POINT('Ctrl Pts',(-0.024598014513208,0.00314909904629757,
-0.00622082004199969));
#50764=CARTESIAN_POINT('Ctrl Pts',(-0.0246394426369129,0.00317286623215922,
-0.00620987083642133));
#50765=CARTESIAN_POINT('Ctrl Pts',(-0.0246820683894351,0.00319736290427895,
-0.00619875383540347));
#50766=CARTESIAN_POINT('Ctrl Pts',(-0.0247868163902898,0.00325756072555608,
-0.00617143505360567));
#50767=CARTESIAN_POINT('Ctrl Pts',(-0.0248987288283024,0.00332221997852365,
-0.00614300928379103));
#50768=CARTESIAN_POINT('Ctrl Pts',(-0.0250319267246202,0.00339816141664959,
-0.0061105002291567));
#50769=CARTESIAN_POINT('Ctrl Pts',(-0.025040910428721,0.00340328338499874,
-0.00610830761399155));
#50770=CARTESIAN_POINT('Ctrl Pts',(-0.0250499912615901,0.00340845601431403,
-0.00610609669903062));
#50771=CARTESIAN_POINT('Ctrl Pts',(-0.0250591736190017,0.00341368127427967,
-0.00610386674487505));
#50772=CARTESIAN_POINT('Ctrl Pts',(-0.0251318364236611,0.00345503035569324,
-0.00608622043511567));
#50773=CARTESIAN_POINT('Ctrl Pts',(-0.025210875135261,0.00349968439401741,
-0.00606743730546045));
#50774=CARTESIAN_POINT('Ctrl Pts',(-0.0252803579825825,0.00353851440133161,
-0.00605123333538441));
#50775=CARTESIAN_POINT('Ctrl Pts',(-0.0253765429748567,0.00359226671715477,
-0.00602880220602436));
#50776=CARTESIAN_POINT('Ctrl Pts',(-0.0254566923453874,0.0036363488594505,
-0.0060106534133979));
#50777=CARTESIAN_POINT('Ctrl Pts',(-0.0255299124417394,0.0036761538151833,
-0.00599432966967733));
#50778=CARTESIAN_POINT('Ctrl Pts',(-0.0255790076456114,0.00370284365191094,
-0.00598338434775283));
#50779=CARTESIAN_POINT('Ctrl Pts',(-0.0256196248685335,0.00372468467997514,
-0.00597446684985712));
#50780=CARTESIAN_POINT('Ctrl Pts',(-0.0256528411804496,0.0037424500534779,
-0.00596722158133266));
#50781=CARTESIAN_POINT('Ctrl Pts',(-0.0256841652496382,0.00375920338208849,
-0.00596038905600223));
#50782=CARTESIAN_POINT('Ctrl Pts',(-0.0257148294720635,0.00377554739889252,
-0.00595373195874594));
#50783=CARTESIAN_POINT('Ctrl Pts',(-0.0257622051350364,0.00380048230091671,
-0.00594359467047805));
#50784=CARTESIAN_POINT('Ctrl Pts',(-0.0258061642031996,0.00382361897044148,
-0.00593418845391045));
#50785=CARTESIAN_POINT('Ctrl Pts',(-0.0258599297734075,0.00385162737452401,
-0.00592281763862265));
#50786=CARTESIAN_POINT('Ctrl Pts',(-0.0259087270781427,0.00387670604391645,
-0.00591263710437559));
#50787=CARTESIAN_POINT('Ctrl Pts',(-0.0259536558801419,0.0038997965522478,
-0.00590326365209347));
#50788=CARTESIAN_POINT('Ctrl Pts',(-0.0259943389037606,0.00392045407114615,
-0.00589487706119322));
#50789=CARTESIAN_POINT('Ctrl Pts',(-0.0260350849839353,0.0039408431970337,
-0.00588654105989476));
#50790=CARTESIAN_POINT('Ctrl Pts',(-0.0260488265955664,0.00394771942778381,
-0.00588372974425634));
#50791=CARTESIAN_POINT('Ctrl Pts',(-0.0260625759974508,0.00395456380062419,
-0.0058809247125566));
#50792=CARTESIAN_POINT('Ctrl Pts',(-0.0260764997386049,0.00396145957792697,
-0.00587809239311163));
#50793=CARTESIAN_POINT('Ctrl Pts',(-0.0261869194675372,0.00401614530154976,
-0.00585563119235378));
#50794=CARTESIAN_POINT('Ctrl Pts',(-0.0263081686292907,0.00407431886964289,
-0.00583164341641599));
#50795=CARTESIAN_POINT('Ctrl Pts',(-0.0264247242280828,0.00412797324082191,
-0.00580908996388195));
#50796=CARTESIAN_POINT('',(-0.0328171231859669,0.00544959481071556,-0.00491819439550167));
#50797=CARTESIAN_POINT('Ctrl Pts',(-0.0264247148113527,0.00412797976408685,
-0.00580905681399726));
#50798=CARTESIAN_POINT('Ctrl Pts',(-0.0266806623606955,0.004265817161036,
-0.00576358983715232));
#50799=CARTESIAN_POINT('Ctrl Pts',(-0.0271941586176829,0.00451878908321525,
-0.00567666122695133));
#50800=CARTESIAN_POINT('Ctrl Pts',(-0.0279187082618112,0.00481814426352985,
-0.00556288680148345));
#50801=CARTESIAN_POINT('Ctrl Pts',(-0.0287529968670884,0.00509216436953578,
-0.00544119748457045));
#50802=CARTESIAN_POINT('Ctrl Pts',(-0.0293995276465761,0.00524409592488056,
-0.00535269372197882));
#50803=CARTESIAN_POINT('Ctrl Pts',(-0.0298940640370636,0.0053307414006189,
-0.00528612781180627));
#50804=CARTESIAN_POINT('Ctrl Pts',(-0.0304875804327081,0.00541300424438409,
-0.0052085859306323));
#50805=CARTESIAN_POINT('Ctrl Pts',(-0.0311383125186733,0.00547351091878673,
-0.00512782359057905));
#50806=CARTESIAN_POINT('Ctrl Pts',(-0.0320222448303377,0.00549729197974687,
-0.00502013830682495));
#50807=CARTESIAN_POINT('Ctrl Pts',(-0.032554724307738,0.00547129131445063,
-0.00495300644550675));
#50808=CARTESIAN_POINT('Ctrl Pts',(-0.0328171226451392,0.0054495948957978,
-0.00491819447958816));
#50809=CARTESIAN_POINT('Ctrl Pts',(-0.0399999990786919,0.00503253317335571,
-0.00434874780361082));
#50810=CARTESIAN_POINT('Ctrl Pts',(-0.0398079283434003,0.00503365259361514,
-0.00434938296194158));
#50811=CARTESIAN_POINT('Ctrl Pts',(-0.0396323617472513,0.00503489684903665,
-0.00435089211560653));
#50812=CARTESIAN_POINT('Ctrl Pts',(-0.0394783469992459,0.00503629893077916,
-0.00435286393834884));
#50813=CARTESIAN_POINT('Ctrl Pts',(-0.0393243322512405,0.00503770101252167,
-0.00435483576109114));
#50814=CARTESIAN_POINT('Ctrl Pts',(-0.0391918691385965,0.00503927926839014,
-0.00435723757858893));
#50815=CARTESIAN_POINT('Ctrl Pts',(-0.0390658193474297,0.00504149043886893,
-0.00436023263436879));
#50816=CARTESIAN_POINT('Ctrl Pts',(-0.0390027944518462,0.00504259602410833,
-0.00436173016225873));
#50817=CARTESIAN_POINT('Ctrl Pts',(-0.0389413729181224,0.00504386058504307,
-0.00436337471752688));
#50818=CARTESIAN_POINT('Ctrl Pts',(-0.0388715003915693,0.00504548027850166,
-0.00436546028537351));
#50819=CARTESIAN_POINT('Ctrl Pts',(-0.0388016278650162,0.00504709997196025,
-0.00436754585322015));
#50820=CARTESIAN_POINT('Ctrl Pts',(-0.0387233046123729,0.00504906597787632,
-0.00437008823748018));
#50821=CARTESIAN_POINT('Ctrl Pts',(-0.0386461502734439,0.00505118109228873,
-0.0043728342611483));
#50822=CARTESIAN_POINT('Ctrl Pts',(-0.0384918415955858,0.00505541132111354,
-0.00437832630848453));
#50823=CARTESIAN_POINT('Ctrl Pts',(-0.0383422076850759,0.00506025879694506,
-0.00438459512348587));
#50824=CARTESIAN_POINT('Ctrl Pts',(-0.0381946501383217,0.00506566602230368,
-0.00439158507208406));
#50825=CARTESIAN_POINT('Ctrl Pts',(-0.0378995350448133,0.00507648047302089,
-0.00440556496928044));
#50826=CARTESIAN_POINT('Ctrl Pts',(-0.0376127246200382,0.00508955164697904,
-0.00442239696763909));
#50827=CARTESIAN_POINT('Ctrl Pts',(-0.0373174662030721,0.00510514094597655,
-0.00444258389671857));
#50828=CARTESIAN_POINT('Ctrl Pts',(-0.0371698369945891,0.00511293559547531,
-0.00445267736125831));
#50829=CARTESIAN_POINT('Ctrl Pts',(-0.0370200961537913,0.00512135807816629,
-0.00446361373187541));
#50830=CARTESIAN_POINT('Ctrl Pts',(-0.0368619128206017,0.00513094709709688,
-0.00447600706817314));
#50831=CARTESIAN_POINT('Ctrl Pts',(-0.0367037294874121,0.00514053611602746,
-0.00448840040447088));
#50832=CARTESIAN_POINT('Ctrl Pts',(-0.036537106172115,0.00515126175938117,
-0.00450230894043891));
#50833=CARTESIAN_POINT('Ctrl Pts',(-0.0363950645278357,0.00516076588467846,
-0.00451469899300244));
#50834=CARTESIAN_POINT('Ctrl Pts',(-0.0362530228835564,0.00517027000997575,
-0.00452708904556598));
#50835=CARTESIAN_POINT('Ctrl Pts',(-0.0361355575855477,0.00517860019854412,
-0.00453786216343966));
#50836=CARTESIAN_POINT('Ctrl Pts',(-0.0360038343615319,0.00518824122937477,
-0.00455034475502334));
#50837=CARTESIAN_POINT('Ctrl Pts',(-0.0358721111375161,0.00519788226020543,
-0.00456282734660702));
#50838=CARTESIAN_POINT('Ctrl Pts',(-0.0357261339316059,0.00520880455506361,
-0.00457708358477853));
#50839=CARTESIAN_POINT('Ctrl Pts',(-0.0355774733705788,0.0052202231385025,
-0.00459211847497182));
#50840=CARTESIAN_POINT('Ctrl Pts',(-0.0354288128095516,0.0052316417219414,
-0.00460715336516512));
#50841=CARTESIAN_POINT('Ctrl Pts',(-0.0352774671293249,0.00524356784153638,
-0.00462294121804181));
#50842=CARTESIAN_POINT('Ctrl Pts',(-0.0351160105361898,0.00525659897498482,
-0.00464033438166046));
#50843=CARTESIAN_POINT('Ctrl Pts',(-0.0349545539430548,0.00526963010843325,
-0.00465772754527911));
#50844=CARTESIAN_POINT('Ctrl Pts',(-0.0347829889395164,0.00528375105812449,
-0.00467676133373444));
#50845=CARTESIAN_POINT('Ctrl Pts',(-0.0346194848568192,0.00529730904529849,
-0.0046953590234092));
#50846=CARTESIAN_POINT('Ctrl Pts',(-0.0342924766914248,0.00532442501964648,
-0.00473255440275871));
#50847=CARTESIAN_POINT('Ctrl Pts',(-0.0339976954346225,0.005349370351003,
-0.00476779921072633));
#50848=CARTESIAN_POINT('Ctrl Pts',(-0.0337017730542888,0.00537440420893885,
-0.00480443044263055));
#50849=CARTESIAN_POINT('Ctrl Pts',(-0.0334581371642852,0.00539501483748121,
-0.00483458930650848));
#50850=CARTESIAN_POINT('Ctrl Pts',(-0.033213727355736,0.00541565703700328,
-0.00486576883655851));
#50851=CARTESIAN_POINT('Ctrl Pts',(-0.0329721975600362,0.00543630250710774,
-0.0048976089131913));
#50852=CARTESIAN_POINT('Ctrl Pts',(-0.0329203630568065,0.00544073321381913,
-0.00490444208485144));
#50853=CARTESIAN_POINT('Ctrl Pts',(-0.0328686603418303,0.00544516406868864,
-0.00491130527685778));
#50854=CARTESIAN_POINT('Ctrl Pts',(-0.0328171242669787,0.00544959475255144,
-0.00491819426162666));
#50855=CARTESIAN_POINT('Ctrl Pts',(-0.04,0.00749999999999979,-0.005));
#50856=CARTESIAN_POINT('Ctrl Pts',(-0.0303557247091859,0.0075,-0.005));
#50857=CARTESIAN_POINT('Ctrl Pts',(-0.0244205064310119,0.0075,-0.00571826182059907));
#50858=CARTESIAN_POINT('Ctrl Pts',(-0.0153166543938371,0.00749997945719785,
-0.0101211778088248));
#50859=CARTESIAN_POINT('Ctrl Pts',(-0.04,0.0100485913697267,0.00430251487755884));
#50860=CARTESIAN_POINT('Ctrl Pts',(-0.0301947260752482,0.0100485913697267,
0.00430251487755884));
#50861=CARTESIAN_POINT('Ctrl Pts',(-0.0242897188632192,0.0113547636009066,
0.00566740485375001));
#50862=CARTESIAN_POINT('Ctrl Pts',(-0.015132689504921,0.0126609342369608,
0.0102218440523409));
#50863=CARTESIAN_POINT('Ctrl Pts',(-0.04,0.0100244455634135,0.00431627900887509));
#50864=CARTESIAN_POINT('Ctrl Pts',(-0.0301965679597973,0.0100244455634135,
0.00431627900887509));
#50865=CARTESIAN_POINT('Ctrl Pts',(-0.0242906767905071,0.0113158683097808,
0.0056688196752123));
#50866=CARTESIAN_POINT('Ctrl Pts',(-0.015132689504921,0.0126072894913072,
0.0102218440523409));
#50867=CARTESIAN_POINT('Ctrl Pts',(-0.04,0.0100002997571002,0.00433004314019135));
#50868=CARTESIAN_POINT('Ctrl Pts',(-0.0301984098443463,0.0100002997571002,
0.00433004314019135));
#50869=CARTESIAN_POINT('Ctrl Pts',(-0.0242916347177951,0.0112769730186549,
0.00567023449667458));
#50870=CARTESIAN_POINT('Ctrl Pts',(-0.015132689504921,0.0125536447456536,
0.0102218440523409));
#50871=CARTESIAN_POINT('Ctrl Pts',(-0.04,0.00997615395078692,0.0043438072715076));
#50872=CARTESIAN_POINT('Ctrl Pts',(-0.0302002517288954,0.00997615395078692,
0.0043438072715076));
#50873=CARTESIAN_POINT('Ctrl Pts',(-0.024292592645083,0.011238077727529,
0.00567164931813686));
#50874=CARTESIAN_POINT('Ctrl Pts',(-0.015132689504921,0.0125,0.0102218440523409));
#50875=CARTESIAN_POINT('Ctrl Pts',(-0.04,0.00978860990508501,0.00445071531338999));
#50876=CARTESIAN_POINT('Ctrl Pts',(-0.030214557918366,0.00978860990508501,
0.00445071531338999));
#50877=CARTESIAN_POINT('Ctrl Pts',(-0.0243000330078826,0.0109359722537311,
0.00568263844550496));
#50878=CARTESIAN_POINT('Ctrl Pts',(-0.015132689504921,0.0120833333333333,
0.0102218440523409));
#50879=CARTESIAN_POINT('Ctrl Pts',(-0.04,0.00939955463535607,0.00464026426357805));
#50880=CARTESIAN_POINT('Ctrl Pts',(-0.0302431702683995,0.00939955463535607,
0.00464026426357805));
#50881=CARTESIAN_POINT('Ctrl Pts',(-0.0243148560847983,0.010324886351761,
0.00570100281151992));
#50882=CARTESIAN_POINT('Ctrl Pts',(-0.015132689504921,0.0112502172223832,
0.0102218440523409));
#50883=CARTESIAN_POINT('Ctrl Pts',(-0.04,0.00878403081131148,0.00484680862067135));
#50884=CARTESIAN_POINT('Ctrl Pts',(-0.0302697286340305,0.00878403081131148,
0.00484680862067135));
#50885=CARTESIAN_POINT('Ctrl Pts',(-0.0243287164435937,0.00939236853247558,
0.00571836367863856));
#50886=CARTESIAN_POINT('Ctrl Pts',(-0.015132689504921,0.0100007058837482,
0.0102218440523409));
#50887=CARTESIAN_POINT('Ctrl Pts',(-0.04,0.00814718747550223,0.00497205619922113));
#50888=CARTESIAN_POINT('Ctrl Pts',(-0.0302858937355252,0.00814718747550223,
0.00497205619922113));
#50889=CARTESIAN_POINT('Ctrl Pts',(-0.0243371647192728,0.00844902839074704,
0.00572692482666522));
#50890=CARTESIAN_POINT('Ctrl Pts',(-0.015132689504921,0.00875086923557139,
0.0102218440523409));
#50891=CARTESIAN_POINT('Ctrl Pts',(-0.04,0.00771565028284425,0.005));
#50892=CARTESIAN_POINT('Ctrl Pts',(-0.0302893398503779,0.00771565028284425,
0.005));
#50893=CARTESIAN_POINT('Ctrl Pts',(-0.0243389737765017,0.00781637598055064,
0.00572818395833523));
#50894=CARTESIAN_POINT('Ctrl Pts',(-0.015132689504921,0.00791710167825684,
0.0102218440523409));
#50895=CARTESIAN_POINT('Ctrl Pts',(-0.04,0.00728479953731841,0.005));
#50896=CARTESIAN_POINT('Ctrl Pts',(-0.0302893395753294,0.00728479953731841,
0.005));
#50897=CARTESIAN_POINT('Ctrl Pts',(-0.0243389736389774,0.00718428394112105,
0.00572818395833523));
#50898=CARTESIAN_POINT('Ctrl Pts',(-0.015132689504921,0.0070837683449235,
0.0102218440523409));
#50899=CARTESIAN_POINT('Ctrl Pts',(-0.04,0.00685462242848371,0.00497218239515157));
#50900=CARTESIAN_POINT('Ctrl Pts',(-0.0302859072730621,0.00685462242848371,
0.00497218239515157));
#50901=CARTESIAN_POINT('Ctrl Pts',(-0.0243371722033388,0.00655274665477437,
0.00572688218702066));
#50902=CARTESIAN_POINT('Ctrl Pts',(-0.015132689504921,0.00625087081123028,
0.0102218440523409));
#50903=CARTESIAN_POINT('Ctrl Pts',(-0.04,0.00622049631377248,0.00484786604032014));
#50904=CARTESIAN_POINT('Ctrl Pts',(-0.030269763463618,0.00622049631377248,
0.00484786604032014));
#50905=CARTESIAN_POINT('Ctrl Pts',(-0.0243287375276573,0.00561060229378754,
0.00571834998513381));
#50906=CARTESIAN_POINT('Ctrl Pts',(-0.015132689504921,0.00500070790691571,
0.0102218440523409));
#50907=CARTESIAN_POINT('Ctrl Pts',(-0.04,0.00560781375559217,0.00464312151315633));
#50908=CARTESIAN_POINT('Ctrl Pts',(-0.0302432149127319,0.00560781375559217,
0.00464312151315633));
#50909=CARTESIAN_POINT('Ctrl Pts',(-0.0243148866463651,0.0046790161922589,
0.00570121346148063));
#50910=CARTESIAN_POINT('Ctrl Pts',(-0.015132689504921,0.00375021778988959,
0.0102218440523409));
#50911=CARTESIAN_POINT('Ctrl Pts',(-0.04,0.00522022257304718,0.00445520250630582));
#50912=CARTESIAN_POINT('Ctrl Pts',(-0.0302146387773497,0.00522022257304718,
0.00445520250630582));
#50913=CARTESIAN_POINT('Ctrl Pts',(-0.0243000856243898,0.00406844524938924,
0.00568308051796475));
#50914=CARTESIAN_POINT('Ctrl Pts',(-0.015132689504921,0.00291666666666667,
0.0102218440523409));
#50915=CARTESIAN_POINT('Ctrl Pts',(-0.04,0.00503323066735754,0.0043491434857377));
#50916=CARTESIAN_POINT('Ctrl Pts',(-0.0302003506952954,0.00503323066735754,
0.0043491434857377));
#50917=CARTESIAN_POINT('Ctrl Pts',(-0.0242926564701765,0.00376661607994243,
0.00567219736021384));
#50918=CARTESIAN_POINT('Ctrl Pts',(-0.015132689504921,0.0025,0.0102218440523409));
#50919=CARTESIAN_POINT('Ctrl Pts',(-0.04,0.00471683689703473,0.00416968965713194));
#50920=CARTESIAN_POINT('Ctrl Pts',(-0.0301761749956299,0.00471683689703473,
0.00416968965713194));
#50921=CARTESIAN_POINT('Ctrl Pts',(-0.024280086203548,0.00325591553083319,
0.00565378285557991));
#50922=CARTESIAN_POINT('Ctrl Pts',(-0.015132689504921,0.00179499227708115,
0.0102218440523409));
#50923=CARTESIAN_POINT('Ctrl Pts',(-0.04,0.00440044312671191,0.00399023582852618));
#50924=CARTESIAN_POINT('Ctrl Pts',(-0.0301519992959643,0.00440044312671191,
0.00399023582852618));
#50925=CARTESIAN_POINT('Ctrl Pts',(-0.0242675159369196,0.00274521498172396,
0.005635368350946));
#50926=CARTESIAN_POINT('Ctrl Pts',(-0.015132689504921,0.00108998455416231,
0.0102218440523409));
#50927=CARTESIAN_POINT('Ctrl Pts',(-0.04,0.00408404935638909,0.00381078199992041));
#50928=CARTESIAN_POINT('Ctrl Pts',(-0.0301278235962988,0.00408404935638909,
0.00381078199992041));
#50929=CARTESIAN_POINT('Ctrl Pts',(-0.0242549456702911,0.00223451443261473,
0.00561695384631207));
#50930=CARTESIAN_POINT('Ctrl Pts',(-0.015132689504921,0.000384976831243464,
0.0102218440523409));
#50931=CARTESIAN_POINT('',(-0.0151954874261301,0.00138726386665834,0.0101904076586258));
#50932=CARTESIAN_POINT('',(-0.0151988434694278,0.00250046000682414,0.0101890120162147));
#50933=CARTESIAN_POINT('',(-0.0151988171013996,0.00250046001831896,0.0101889589173828));
#50934=CARTESIAN_POINT('',(-0.0152015959590704,0.0114763663518353,0.0101878882534135));
#50935=CARTESIAN_POINT('Ctrl Pts',(-0.0152015961008204,0.0114763663334547,
0.0101878881836326));
#50936=CARTESIAN_POINT('Ctrl Pts',(-0.0152017816534068,0.011398632919723,
0.0101878129849584));
#50937=CARTESIAN_POINT('Ctrl Pts',(-0.0152019618681523,0.0113209171151958,
0.010187739932766));
#50938=CARTESIAN_POINT('Ctrl Pts',(-0.01520213666228,0.0112432182788952,
0.0101876690159898));
#50939=CARTESIAN_POINT('Ctrl Pts',(-0.0152030730346569,0.0108269855086917,
0.0101872891147244));
#50940=CARTESIAN_POINT('Ctrl Pts',(-0.0152038537517294,0.0104112394262679,
0.0101869703999302));
#50941=CARTESIAN_POINT('Ctrl Pts',(-0.0152044807446706,0.0099958840151301,
0.0101867127986388));
#50942=CARTESIAN_POINT('Ctrl Pts',(-0.0152051090343512,0.00957966957078026,
0.0101864546645795));
#50943=CARTESIAN_POINT('Ctrl Pts',(-0.015205583009041,0.00916384747612361,
0.0101862579082725));
#50944=CARTESIAN_POINT('Ctrl Pts',(-0.0152059010693488,0.00874832374241293,
0.0101861245001562));
#50945=CARTESIAN_POINT('Ctrl Pts',(-0.01520621978241,0.00833194723164394,
0.0101859908182471));
#50946=CARTESIAN_POINT('Ctrl Pts',(-0.0152063819377999,0.00791587037027076,
0.0101859207682779));
#50947=CARTESIAN_POINT('Ctrl Pts',(-0.0152063872987604,0.00750000000000001,
0.0101859181580662));
#50948=CARTESIAN_POINT('Ctrl Pts',(-0.0152063926594201,0.00708415296700099,
0.0101859155480011));
#50949=CARTESIAN_POINT('Ctrl Pts',(-0.0152062412439683,0.00666851248133758,
0.0101859801722236));
#50950=CARTESIAN_POINT('Ctrl Pts',(-0.01520593249939,0.00625314726721103,
0.010186109005589));
#50951=CARTESIAN_POINT('Ctrl Pts',(-0.0152056231325436,0.00583694489345328,
0.0101862380986153));
#50952=CARTESIAN_POINT('Ctrl Pts',(-0.0152051558060071,0.00542101895440168,
0.0101864316392808));
#50953=CARTESIAN_POINT('Ctrl Pts',(-0.0152045313571514,0.0050054370581099,
0.0101866883096197));
#50954=CARTESIAN_POINT('Ctrl Pts',(-0.0152039056601427,0.00458902449362444,
0.0101869454929931));
#50955=CARTESIAN_POINT('Ctrl Pts',(-0.0152031221583381,0.0041729573969788,
0.0101872660473249));
#50956=CARTESIAN_POINT('Ctrl Pts',(-0.0152021782357305,0.00375730094918648,
0.0101876505057982));
#50957=CARTESIAN_POINT('Ctrl Pts',(-0.0152012258433854,0.00333791485133816,
0.0101880384139849));
#50958=CARTESIAN_POINT('Ctrl Pts',(-0.0152001103659201,0.00291894870724609,
0.0101884911917733));
#50959=CARTESIAN_POINT('Ctrl Pts',(-0.0151988434694278,0.00250046000682414,
0.0101890120162147));
#50960=CARTESIAN_POINT('',(-0.0312397316217442,0.0094458100603598,0.00513213307870327));
#50961=CARTESIAN_POINT('Ctrl Pts',(-0.0152015959590704,0.0114763663518353,
0.0101878882534135));
#50962=CARTESIAN_POINT('Ctrl Pts',(-0.0164822330050404,0.0115970872170385,
0.00955739480663315));
#50963=CARTESIAN_POINT('Ctrl Pts',(-0.0190840779032895,0.0117290721415925,
0.00834467796691021));
#50964=CARTESIAN_POINT('Ctrl Pts',(-0.0223800331608592,0.0115286687609144,
0.00700184797404235));
#50965=CARTESIAN_POINT('Ctrl Pts',(-0.024989720469363,0.0104626073224454,
0.00625685260897244));
#50966=CARTESIAN_POINT('Ctrl Pts',(-0.0269857198322412,0.0097622199194132,
0.00582377715676942));
#50967=CARTESIAN_POINT('Ctrl Pts',(-0.0290810941162661,0.00943689998545597,
0.00544737164840719));
#50968=CARTESIAN_POINT('Ctrl Pts',(-0.0305231562376279,0.00939584156846951,
0.00523939408016512));
#50969=CARTESIAN_POINT('Ctrl Pts',(-0.0312397316217442,0.0094458100603598,
0.00513213307870327));
#50970=CARTESIAN_POINT('Ctrl Pts',(-0.0399999963113939,0.00997613772986841,
0.00434381651807744));
#50971=CARTESIAN_POINT('Ctrl Pts',(-0.0395727207349401,0.00997285044000123,
0.00434569041850028));
#50972=CARTESIAN_POINT('Ctrl Pts',(-0.0391774221470677,0.00996743224495432,
0.00435266025984037));
#50973=CARTESIAN_POINT('Ctrl Pts',(-0.0388081300295977,0.00995937345471727,
0.00436370338220723));
#50974=CARTESIAN_POINT('Ctrl Pts',(-0.038623483760588,0.00995534405501007,
0.0043692249496786));
#50975=CARTESIAN_POINT('Ctrl Pts',(-0.0384453396441767,0.00995066250224038,
0.00437577831952124));
#50976=CARTESIAN_POINT('Ctrl Pts',(-0.0382796892328055,0.0099455119793533,
0.00438289030257414));
#50977=CARTESIAN_POINT('Ctrl Pts',(-0.0381140388214343,0.00994036145646621,
0.00439000228562705));
#50978=CARTESIAN_POINT('Ctrl Pts',(-0.0379608807865865,0.00993471250155751,
0.00439761931275741));
#50979=CARTESIAN_POINT('Ctrl Pts',(-0.0377962431644136,0.00992758518542438,
0.00440693404825424));
#50980=CARTESIAN_POINT('Ctrl Pts',(-0.0376316055422407,0.00992045786929125,
0.00441624878375107));
#50981=CARTESIAN_POINT('Ctrl Pts',(-0.0374554905385062,0.00991188455435292,
0.00442732222488304));
#50982=CARTESIAN_POINT('Ctrl Pts',(-0.0372779553803839,0.00990245493066738,
0.00443955772907257));
#50983=CARTESIAN_POINT('Ctrl Pts',(-0.0371004202222617,0.00989302530698183,
0.0044517932332621));
#50984=CARTESIAN_POINT('Ctrl Pts',(-0.0369214637592435,0.00988272837523341,
0.00446516860036496));
#50985=CARTESIAN_POINT('Ctrl Pts',(-0.0367394606492448,0.00987155476925158,
0.00447975421625176));
#50986=CARTESIAN_POINT('Ctrl Pts',(-0.0365574575392462,0.00986038116326974,
0.00449433983213856));
#50987=CARTESIAN_POINT('Ctrl Pts',(-0.0363724078513935,0.00984832902852278,
0.00451013306105462));
#50988=CARTESIAN_POINT('Ctrl Pts',(-0.0361807646956626,0.00983512789932526,
0.00452749358356716));
#50989=CARTESIAN_POINT('Ctrl Pts',(-0.0360849431177971,0.0098285273347265,
0.00453617384482344));
#50990=CARTESIAN_POINT('Ctrl Pts',(-0.0359874734742924,0.00982164264879878,
0.00454525213533095));
#50991=CARTESIAN_POINT('Ctrl Pts',(-0.035893843336345,0.00981489791188518,
0.00455418267100008));
#50992=CARTESIAN_POINT('Ctrl Pts',(-0.0358470282673713,0.00981152554342839,
0.00455864793883465));
#50993=CARTESIAN_POINT('Ctrl Pts',(-0.0358011728108698,0.00980818594822577,
0.00456307163081677));
#50994=CARTESIAN_POINT('Ctrl Pts',(-0.0357484897779608,0.00980428569995241,
0.00456823103120321));
#50995=CARTESIAN_POINT('Ctrl Pts',(-0.0356958067450518,0.00980038545167904,
0.00457339043158964));
#50996=CARTESIAN_POINT('Ctrl Pts',(-0.0356362972078298,0.0097959327453508,
0.00457930316019586));
#50997=CARTESIAN_POINT('Ctrl Pts',(-0.0356018745250502,0.00979334381551296,
0.00458274850248771));
#50998=CARTESIAN_POINT('Ctrl Pts',(-0.0355674518422706,0.00979075488567512,
0.00458619384477956));
#50999=CARTESIAN_POINT('Ctrl Pts',(-0.035558114721345,0.00979002055266094,
0.004587151616026));
#51000=CARTESIAN_POINT('Ctrl Pts',(-0.0355408565612769,0.00978866582053624,
0.00458891568512121));
#51001=CARTESIAN_POINT('Ctrl Pts',(-0.0355235984012088,0.00978731108841154,
0.00459067975421642));
#51002=CARTESIAN_POINT('Ctrl Pts',(-0.0354984196904949,0.00978533935191339,
0.00459325763773581));
#51003=CARTESIAN_POINT('Ctrl Pts',(-0.0354733783364266,0.00978335509992397,
0.00459584349182381));
#51004=CARTESIAN_POINT('Ctrl Pts',(-0.0354232956282899,0.00977938659594515,
0.00460101519999981));
#51005=CARTESIAN_POINT('Ctrl Pts',(-0.035373761755283,0.00977536405827277,
0.00460620989793128));
#51006=CARTESIAN_POINT('Ctrl Pts',(-0.0353190429282953,0.00977087262090177,
0.00461201651237702));
#51007=CARTESIAN_POINT('Ctrl Pts',(-0.0352096052743198,0.00976188974615977,
0.00462362974126851));
#51008=CARTESIAN_POINT('Ctrl Pts',(-0.0350794285821523,0.0097510360376019,
0.00463770164690174));
#51009=CARTESIAN_POINT('Ctrl Pts',(-0.0349328736445292,0.00973875823053989,
0.00465393589977913));
#51010=CARTESIAN_POINT('Ctrl Pts',(-0.0347863187069061,0.00972648042347788,
0.00467017015265652));
#51011=CARTESIAN_POINT('Ctrl Pts',(-0.0346233849589686,0.00971277610529657,
0.00468856026966512));
#51012=CARTESIAN_POINT('Ctrl Pts',(-0.0344434237965824,0.00969774093599419,
0.00470937315437457));
#51013=CARTESIAN_POINT('Ctrl Pts',(-0.0342634626341962,0.00968270576669181,
0.00473018603908403));
#51014=CARTESIAN_POINT('Ctrl Pts',(-0.0340664737728119,0.00966633834195001,
0.00475341814438052));
#51015=CARTESIAN_POINT('Ctrl Pts',(-0.0338507957444424,0.00964862558079126,
0.00477957655683347));
#51016=CARTESIAN_POINT('Ctrl Pts',(-0.033635117716073,0.00963091281963251,
0.00480573496928642));
#51017=CARTESIAN_POINT('Ctrl Pts',(-0.0334007516791016,0.00961186312715902,
0.00483483833198576));
#51018=CARTESIAN_POINT('Ctrl Pts',(-0.0331551679662072,0.00959217322514504,
0.00486632682771846));
#51019=CARTESIAN_POINT('Ctrl Pts',(-0.0330760295422204,0.00958582822858368,
0.00487647387654605));
#51020=CARTESIAN_POINT('Ctrl Pts',(-0.0329957316495097,0.00957941374634901,
0.00488686539521972));
#51021=CARTESIAN_POINT('Ctrl Pts',(-0.0329117016047792,0.00957272879821522,
0.00489785656965405));
#51022=CARTESIAN_POINT('Ctrl Pts',(-0.0328653499124219,0.0095690413235707,
0.00490391939560707));
#51023=CARTESIAN_POINT('Ctrl Pts',(-0.0328178634923766,0.00956527148213439,
0.00491016513951892));
#51024=CARTESIAN_POINT('Ctrl Pts',(-0.0327688172992972,0.00956138477500662,
0.0049166573228122));
#51025=CARTESIAN_POINT('Ctrl Pts',(-0.0326308562556758,0.00955045193520946,
0.00493491905377004));
#51026=CARTESIAN_POINT('Ctrl Pts',(-0.0324805400366365,0.00953861874307939,
0.00495519116579573));
#51027=CARTESIAN_POINT('Ctrl Pts',(-0.0323568441831232,0.00952894684544298,
0.00497213739513634));
#51028=CARTESIAN_POINT('Ctrl Pts',(-0.0322331483296099,0.00951927494780657,
0.00498908362447695));
#51029=CARTESIAN_POINT('Ctrl Pts',(-0.0321360619477995,0.00951173925946108,
0.00500261247870721));
#51030=CARTESIAN_POINT('Ctrl Pts',(-0.0320408372393364,0.00950445735094549,
0.00501598963619049));
#51031=CARTESIAN_POINT('Ctrl Pts',(-0.0319456125308732,0.00949717544242991,
0.00502936679367378));
#51032=CARTESIAN_POINT('Ctrl Pts',(-0.0318522535426534,0.00949015539818618,
0.00504262417088863));
#51033=CARTESIAN_POINT('Ctrl Pts',(-0.0317610696020343,0.00948339134457126,
0.00505571215967831));
#51034=CARTESIAN_POINT('Ctrl Pts',(-0.031578701720796,0.00946986323734143,
0.00508188813725767));
#51035=CARTESIAN_POINT('Ctrl Pts',(-0.0314050335764244,0.00945735900266527,
0.00510738446670119));
#51036=CARTESIAN_POINT('Ctrl Pts',(-0.0312397480889472,0.00944581580409354,
0.00513212950872993));
#51037=CARTESIAN_POINT('',(-0.0328230358245329,0.00544566815053618,0.00491342083293496));
#51038=CARTESIAN_POINT('Ctrl Pts',(-0.0328230369063753,0.00544566823007687,
0.004913420741839));
#51039=CARTESIAN_POINT('Ctrl Pts',(-0.0328639380316224,0.00544232996851928,
0.00490802387191221));
#51040=CARTESIAN_POINT('Ctrl Pts',(-0.0329048023388109,0.00543898823253315,
0.0049026586055584));
#51041=CARTESIAN_POINT('Ctrl Pts',(-0.0329456376870304,0.00543564306204493,
0.00489732356927106));
#51042=CARTESIAN_POINT('Ctrl Pts',(-0.0334983654612919,0.00539036443166469,
0.0048251110656123));
#51043=CARTESIAN_POINT('Ctrl Pts',(-0.0340455908507357,0.00534450047275511,
0.00475826196747422));
#51044=CARTESIAN_POINT('Ctrl Pts',(-0.0346080623193213,0.00529790266814098,
0.00469454242292275));
#51045=CARTESIAN_POINT('Ctrl Pts',(-0.0352120889970945,0.00524786223287521,
0.00462611529914093));
#51046=CARTESIAN_POINT('Ctrl Pts',(-0.0358336884751567,0.00519690059485905,
0.0045615118622913));
#51047=CARTESIAN_POINT('Ctrl Pts',(-0.0364254518271606,0.00515762208071706,
0.00451052778445893));
#51048=CARTESIAN_POINT('Ctrl Pts',(-0.0367213335031625,0.00513798282364607,
0.00448503574554275));
#51049=CARTESIAN_POINT('Ctrl Pts',(-0.0370097554634641,0.00512128557881895,
0.00446291352900774));
#51050=CARTESIAN_POINT('Ctrl Pts',(-0.0373032936896531,0.00510605563371512,
0.00444304865414545));
#51051=CARTESIAN_POINT('Ctrl Pts',(-0.037596831915842,0.00509082568861129,
0.00442318377928316));
#51052=CARTESIAN_POINT('Ctrl Pts',(-0.0378954859573303,0.00507705411343856,
0.00440558951191052));
#51053=CARTESIAN_POINT('Ctrl Pts',(-0.0382016060804483,0.00506597225077648,
0.00439128773751753));
#51054=CARTESIAN_POINT('Ctrl Pts',(-0.0383546661420073,0.00506043131944544,
0.00438413685032104));
#51055=CARTESIAN_POINT('Ctrl Pts',(-0.0385095939076617,0.00505554447971043,
0.00437784345578198));
#51056=CARTESIAN_POINT('Ctrl Pts',(-0.0386482553555084,0.00505173469434079,
0.00437294110524465));
#51057=CARTESIAN_POINT('Ctrl Pts',(-0.0387869168033552,0.00504792490897116,
0.00436803875470732));
#51058=CARTESIAN_POINT('Ctrl Pts',(-0.0389093103817168,0.00504523305797351,
0.00436445359723158));
#51059=CARTESIAN_POINT('Ctrl Pts',(-0.0390446531092923,0.00504293774392477,
0.00436126274908846));
#51060=CARTESIAN_POINT('Ctrl Pts',(-0.0393153385644433,0.00503834711582729,
0.00435488105280222));
#51061=CARTESIAN_POINT('Ctrl Pts',(-0.0396378214009135,0.00503522981875482,
0.00435027737761781));
#51062=CARTESIAN_POINT('Ctrl Pts',(-0.0399999989166321,0.00503323485180867,
0.00434914585909333));
#51063=CARTESIAN_POINT('',(-0.0264682077184971,0.00413293976380557,0.00578983210446623));
#51064=CARTESIAN_POINT('Ctrl Pts',(-0.0328230352836106,0.00544566811076599,
0.00491342087848311));
#51065=CARTESIAN_POINT('Ctrl Pts',(-0.0317248902824274,0.00553525857937583,
0.00505830862461719));
#51066=CARTESIAN_POINT('Ctrl Pts',(-0.0306169938636662,0.00546790864877236,
0.00518271767823649));
#51067=CARTESIAN_POINT('Ctrl Pts',(-0.0295432381737695,0.00525773711428087,
0.00532646011294394));
#51068=CARTESIAN_POINT('Ctrl Pts',(-0.0294386032779061,0.00523725640639555,
0.00534046746566699));
#51069=CARTESIAN_POINT('Ctrl Pts',(-0.0293344280137762,0.00521502239184281,
0.00535450046456667));
#51070=CARTESIAN_POINT('Ctrl Pts',(-0.029230698113076,0.00519108565783119,
0.00536858848140193));
#51071=CARTESIAN_POINT('Ctrl Pts',(-0.0288021936660945,0.0050922038802439,
0.00542678556654621));
#51072=CARTESIAN_POINT('Ctrl Pts',(-0.0283812536935357,0.00496418264609604,
0.00548594698764365));
#51073=CARTESIAN_POINT('Ctrl Pts',(-0.0279671299999509,0.00481124380670639,
0.00554783288921987));
#51074=CARTESIAN_POINT('Ctrl Pts',(-0.0274527576160298,0.00462128240959336,
0.005624699775172));
#51075=CARTESIAN_POINT('Ctrl Pts',(-0.0269519544474792,0.0043856239194066,
0.00570367476051854));
#51076=CARTESIAN_POINT('Ctrl Pts',(-0.0264682077184971,0.00413293976380557,
0.00578983210446623));
#51077=CARTESIAN_POINT('Ctrl Pts',(-0.0264682077184971,0.00413293976380557,
0.00578983210446622));
#51078=CARTESIAN_POINT('Ctrl Pts',(-0.0255345075599796,0.00370448613396262,
0.00596797782102129));
#51079=CARTESIAN_POINT('Ctrl Pts',(-0.0242258662820284,0.00284076935409089,
0.00627087795151936));
#51080=CARTESIAN_POINT('Ctrl Pts',(-0.022409245668868,0.00204459924778921,
0.00690371256898279));
#51081=CARTESIAN_POINT('Ctrl Pts',(-0.0204776433343773,0.00155987639176132,
0.00768508726377031));
#51082=CARTESIAN_POINT('Ctrl Pts',(-0.0180574935154255,0.00137301442411395,
0.00878450427407825));
#51083=CARTESIAN_POINT('Ctrl Pts',(-0.0161475216239444,0.00137134461148134,
0.00971405996459154));
#51084=CARTESIAN_POINT('Ctrl Pts',(-0.0151954862452661,0.00138726386753766,
0.0101904052898562));
#51085=CARTESIAN_POINT('Ctrl Pts',(-0.04,0.00749999999999979,-0.005));
#51086=CARTESIAN_POINT('Ctrl Pts',(-0.0303290418474347,0.0075,-0.005));
#51087=CARTESIAN_POINT('Ctrl Pts',(-0.0243876928299813,0.0075,-0.00572224175535161));
#51088=CARTESIAN_POINT('Ctrl Pts',(-0.0152410184731965,0.00749997928621807,
-0.0101578071909577));
#51089=CARTESIAN_POINT('Ctrl Pts',(-0.04,0.00771571946746142,-0.005));
#51090=CARTESIAN_POINT('Ctrl Pts',(-0.030332352871244,0.00771570651417863,
-0.005));
#51091=CARTESIAN_POINT('Ctrl Pts',(-0.0243938667366865,0.00781640214171287,
-0.00571957082345507));
#51092=CARTESIAN_POINT('Ctrl Pts',(-0.015250055386927,0.00791708269062151,
-0.0101524651702489));
#51093=CARTESIAN_POINT('Ctrl Pts',(-0.04,0.00814739511140643,-0.0049720382424295));
#51094=CARTESIAN_POINT('Ctrl Pts',(-0.0303359967783258,0.00814739511140643,
-0.0049720382424295));
#51095=CARTESIAN_POINT('Ctrl Pts',(-0.0244048070000265,0.00844913472747877,
-0.00571297156313869));
#51096=CARTESIAN_POINT('Ctrl Pts',(-0.0152681197724132,0.00875085370023442,
-0.010141786710297));
#51097=CARTESIAN_POINT('Ctrl Pts',(-0.04,0.00878443578896302,-0.00484671062820502));
#51098=CARTESIAN_POINT('Ctrl Pts',(-0.0303292164550866,0.00878443578896302,
-0.00484671062820502));
#51099=CARTESIAN_POINT('Ctrl Pts',(-0.0244153222548556,0.00939257582974028,
-0.00569640045348333));
#51100=CARTESIAN_POINT('Ctrl Pts',(-0.0152951986997117,0.0100006955268584,
-0.0101257794544224));
#51101=CARTESIAN_POINT('Ctrl Pts',(-0.04,0.00940013645719661,-0.00464003578100023));
#51102=CARTESIAN_POINT('Ctrl Pts',(-0.0303128163764084,0.00940013645719661,
-0.00464003578100023));
#51103=CARTESIAN_POINT('Ctrl Pts',(-0.024421239683557,0.0103251841843068,
-0.00567102489989924));
#51104=CARTESIAN_POINT('Ctrl Pts',(-0.0153222705788916,0.0112502120439379,
-0.0101097763649254));
#51105=CARTESIAN_POINT('Ctrl Pts',(-0.04,0.00978928948362159,-0.0044503691604976));
#51106=CARTESIAN_POINT('Ctrl Pts',(-0.030290878085034,0.00978928948362159,
-0.0044503691604976));
#51107=CARTESIAN_POINT('Ctrl Pts',(-0.0244198128798258,0.0109363202673876,
-0.00564731163699517));
#51108=CARTESIAN_POINT('Ctrl Pts',(-0.0153403208502169,0.0120833316071848,
-0.0100991062483243));
#51109=CARTESIAN_POINT('Ctrl Pts',(-0.04,0.00997687591821936,-0.00434339564002003));
#51110=CARTESIAN_POINT('Ctrl Pts',(-0.0302799089538077,0.00997687591821936,
-0.00434339564002003));
#51111=CARTESIAN_POINT('Ctrl Pts',(-0.0244191294928241,0.0112384475634125,
-0.00563364610458802));
#51112=CARTESIAN_POINT('Ctrl Pts',(-0.0153493483390368,0.0125,-0.010093769798994));
#51113=CARTESIAN_POINT('Ctrl Pts',(-0.04,0.00998137799264972,-0.00434082827552856));
#51114=CARTESIAN_POINT('Ctrl Pts',(-0.0302796456946583,0.00998137799264972,
-0.00434082827552856));
#51115=CARTESIAN_POINT('Ctrl Pts',(-0.024419113091536,0.0112456986185171,
-0.00563331813181025));
#51116=CARTESIAN_POINT('Ctrl Pts',(-0.0153495649987685,0.0125100000414276,
-0.01009364172421));
#51117=CARTESIAN_POINT('Ctrl Pts',(-0.04,0.00998588006708007,-0.00433826091103709));
#51118=CARTESIAN_POINT('Ctrl Pts',(-0.0302793824355088,0.00998588006708007,
-0.00433826091103709));
#51119=CARTESIAN_POINT('Ctrl Pts',(-0.024419096690248,0.0112529496736217,
-0.00563299015903248));
#51120=CARTESIAN_POINT('Ctrl Pts',(-0.0153497816585002,0.0125200000828552,
-0.0100935136494261));
#51121=CARTESIAN_POINT('Ctrl Pts',(-0.04,0.00999038214151043,-0.00433569354654562));
#51122=CARTESIAN_POINT('Ctrl Pts',(-0.0302791191763594,0.00999038214151043,
-0.00433569354654562));
#51123=CARTESIAN_POINT('Ctrl Pts',(-0.0244190802889599,0.0112602007287263,
-0.0056326621862547));
#51124=CARTESIAN_POINT('Ctrl Pts',(-0.0153499983182319,0.0125300001242828,
-0.0100933855746422));
#51125=CARTESIAN_POINT('',(-0.0312862171088903,0.00944638115495657,-0.00512344456391754));
#51126=CARTESIAN_POINT('',(-0.0153993022433853,0.0114667765373308,-0.0100716954734317));
#51127=CARTESIAN_POINT('Ctrl Pts',(-0.0312862115324821,0.00944637453608856,
-0.00512344689700562));
#51128=CARTESIAN_POINT('Ctrl Pts',(-0.0309637776590882,0.00942387733413622,
-0.0051712822208625));
#51129=CARTESIAN_POINT('Ctrl Pts',(-0.0306252671936168,0.00941459983377785,
-0.00522057750595682));
#51130=CARTESIAN_POINT('Ctrl Pts',(-0.0302766727676078,0.0094192040795314,
-0.00527223065634118));
#51131=CARTESIAN_POINT('Ctrl Pts',(-0.0301023755546034,0.00942150620240818,
-0.00529805723153336));
#51132=CARTESIAN_POINT('Ctrl Pts',(-0.0299255532958684,0.00942727365630772,
-0.00532444668236705));
#51133=CARTESIAN_POINT('Ctrl Pts',(-0.0297403618928456,0.00943736002554799,
-0.00535253435011197));
#51134=CARTESIAN_POINT('Ctrl Pts',(-0.029556761151514,0.0094473597600909,
-0.00538038076488105));
#51135=CARTESIAN_POINT('Ctrl Pts',(-0.0293649521540202,0.00946162638074927,
-0.00541002676602812));
#51136=CARTESIAN_POINT('Ctrl Pts',(-0.0291876741818143,0.00947800447060625,
-0.00543813008769592));
#51137=CARTESIAN_POINT('Ctrl Pts',(-0.0291861382986962,0.00947814636545876,
-0.00543837356643599));
#51138=CARTESIAN_POINT('Ctrl Pts',(-0.0291846035006668,0.0094782883980757,
-0.00543861692592945));
#51139=CARTESIAN_POINT('Ctrl Pts',(-0.0291830698022148,0.0094784305660575,
-0.00543886016370823));
#51140=CARTESIAN_POINT('Ctrl Pts',(-0.0290045102947476,0.00949498234960806,
-0.00546717891040807));
#51141=CARTESIAN_POINT('Ctrl Pts',(-0.0288408630926145,0.00951330253321414,
-0.00549375476339945));
#51142=CARTESIAN_POINT('Ctrl Pts',(-0.0286701482711043,0.00953506074917197,
-0.00552219615883888));
#51143=CARTESIAN_POINT('Ctrl Pts',(-0.028508184501729,0.00955570361216557,
-0.00554917961329769));
#51144=CARTESIAN_POINT('Ctrl Pts',(-0.0283399114830045,0.00957969213306091,
-0.00557789203041364));
#51145=CARTESIAN_POINT('Ctrl Pts',(-0.0281683704016501,0.00960696702812576,
-0.00560802085849635));
#51146=CARTESIAN_POINT('Ctrl Pts',(-0.0281591018784983,0.00960844071591165,
-0.0056096487469206));
#51147=CARTESIAN_POINT('Ctrl Pts',(-0.0281498237908751,0.00960992389677818,
-0.00561128075793803));
#51148=CARTESIAN_POINT('Ctrl Pts',(-0.0281405366360636,0.00961141669311603,
-0.00561291680941586));
#51149=CARTESIAN_POINT('Ctrl Pts',(-0.0279593635666388,0.00964053804406211,
-0.00564483277011575));
#51150=CARTESIAN_POINT('Ctrl Pts',(-0.0277747902540233,0.00967354473406514,
-0.00567833500513236));
#51151=CARTESIAN_POINT('Ctrl Pts',(-0.0276041796877202,0.0097071526084523,
-0.0057101570143216));
#51152=CARTESIAN_POINT('Ctrl Pts',(-0.0274515130799449,0.00973722577618398,
-0.00573863214514608));
#51153=CARTESIAN_POINT('Ctrl Pts',(-0.0273100027030909,0.0097677872656343,
-0.00576563349689761));
#51154=CARTESIAN_POINT('Ctrl Pts',(-0.0271674409538542,0.00980147476959505,
-0.00579334150457946));
#51155=CARTESIAN_POINT('Ctrl Pts',(-0.0271506846889891,0.00980543429409607,
-0.00579659821767458));
#51156=CARTESIAN_POINT('Ctrl Pts',(-0.0271339143954177,0.00980943896688865,
-0.00579986504241665));
#51157=CARTESIAN_POINT('Ctrl Pts',(-0.0271171104745114,0.00981349342444696,
-0.00580314598638567));
#51158=CARTESIAN_POINT('Ctrl Pts',(-0.0269573393483396,0.00985204307328881,
-0.00583434109351309));
#51159=CARTESIAN_POINT('Ctrl Pts',(-0.0267945505097115,0.00989516287810736,
-0.00586677365462162));
#51160=CARTESIAN_POINT('Ctrl Pts',(-0.0266247015642492,0.00994409565256879,
-0.00590153635079375));
#51161=CARTESIAN_POINT('Ctrl Pts',(-0.0264784296662473,0.00998623597775886,
-0.00593147357256995));
#51162=CARTESIAN_POINT('Ctrl Pts',(-0.02632699118218,0.0100328896891732,
-0.00596318698623446));
#51163=CARTESIAN_POINT('Ctrl Pts',(-0.0261854108087996,0.0100788793244123,
-0.005993548729033));
#51164=CARTESIAN_POINT('Ctrl Pts',(-0.0260760741453728,0.0101143952165463,
-0.0060169958465547));
#51165=CARTESIAN_POINT('Ctrl Pts',(-0.0259768435751314,0.0101478543253226,
-0.00603864076498111));
#51166=CARTESIAN_POINT('Ctrl Pts',(-0.0258650339339585,0.0101868563097126,
-0.00606350292810076));
#51167=CARTESIAN_POINT('Ctrl Pts',(-0.0257714448770845,0.0102195025010159,
-0.00608431353417914));
#51168=CARTESIAN_POINT('Ctrl Pts',(-0.0256712562003281,0.0102555305630453,
-0.00610698811533278));
#51169=CARTESIAN_POINT('Ctrl Pts',(-0.0255880677504924,0.0102861067539666,
-0.00612610003138942));
#51170=CARTESIAN_POINT('Ctrl Pts',(-0.025525742218938,0.0103090147100091,
-0.0061404188500428));
#51171=CARTESIAN_POINT('Ctrl Pts',(-0.0254695370675074,0.0103300005111268,
-0.00615347166176308));
#51172=CARTESIAN_POINT('Ctrl Pts',(-0.0254073476614081,0.0103535531862672,
-0.00616807571128237));
#51173=CARTESIAN_POINT('Ctrl Pts',(-0.0253535877382479,0.0103739134065231,
-0.00618070025023894));
#51174=CARTESIAN_POINT('Ctrl Pts',(-0.02529536568145,0.0103962193642769,
-0.0061944786610525));
#51175=CARTESIAN_POINT('Ctrl Pts',(-0.0252255351681319,0.0104234572923136,
-0.00621124134451748));
#51176=CARTESIAN_POINT('Ctrl Pts',(-0.0251985237534633,0.0104339933020599,
-0.00621772538383666));
#51177=CARTESIAN_POINT('Ctrl Pts',(-0.0251697766855383,0.0104452709085224,
-0.00622465763411363));
#51178=CARTESIAN_POINT('Ctrl Pts',(-0.0251388823553466,0.0104574636526724,
-0.00623215469285687));
#51179=CARTESIAN_POINT('Ctrl Pts',(-0.0250835008335655,0.0104793205021827,
-0.00624559400419674));
#51180=CARTESIAN_POINT('Ctrl Pts',(-0.0250212132534462,0.010504071707771,
-0.00626089235119378));
#51181=CARTESIAN_POINT('Ctrl Pts',(-0.0249682462297451,0.0105251887155644,
-0.00627405373492803));
#51182=CARTESIAN_POINT('Ctrl Pts',(-0.0249152792060441,0.0105463057233577,
-0.00628721511866228));
#51183=CARTESIAN_POINT('Ctrl Pts',(-0.0248716198962152,0.010563783125094,
-0.0062981968652453));
#51184=CARTESIAN_POINT('Ctrl Pts',(-0.0248308177276274,0.0105801367421535,
-0.006308532384367));
#51185=CARTESIAN_POINT('Ctrl Pts',(-0.0247900155590396,0.0105964903592131,
-0.00631886790348869));
#51186=CARTESIAN_POINT('Ctrl Pts',(-0.0247520767790388,0.010611722753729,
-0.00632857766546725));
#51187=CARTESIAN_POINT('Ctrl Pts',(-0.0247266465107074,0.0106219494716524,
-0.00633511323708019));
#51188=CARTESIAN_POINT('Ctrl Pts',(-0.0247012162423761,0.0106321761895758,
-0.00634164880869312));
#51189=CARTESIAN_POINT('Ctrl Pts',(-0.0246882845826022,0.0106373932110363,
-0.00634497791720677));
#51190=CARTESIAN_POINT('Ctrl Pts',(-0.0246557765988998,0.0106503533471222,
-0.00635343174145392));
#51191=CARTESIAN_POINT('Ctrl Pts',(-0.0246232686151974,0.010663313483208,
-0.00636188556570107));
#51192=CARTESIAN_POINT('Ctrl Pts',(-0.0245712030177206,0.0106840242428176,
-0.0063755247135945));
#51193=CARTESIAN_POINT('Ctrl Pts',(-0.0245254529294777,0.0107021203012,
-0.00638766004577755));
#51194=CARTESIAN_POINT('Ctrl Pts',(-0.0244797028412348,0.0107202163595824,
-0.0063997953779606));
#51195=CARTESIAN_POINT('Ctrl Pts',(-0.0244402539648504,0.0107356922099638,
-0.00641038150709176));
#51196=CARTESIAN_POINT('Ctrl Pts',(-0.024401787931292,0.0107507207636909,
-0.00642078275342784));
#51197=CARTESIAN_POINT('Ctrl Pts',(-0.0243591309274041,0.0107673867158431,
-0.00643231724150351));
#51198=CARTESIAN_POINT('Ctrl Pts',(-0.0243176756195971,0.010783475382793,
-0.00644363819738632));
#51199=CARTESIAN_POINT('Ctrl Pts',(-0.0242760142822199,0.0107994740995014,
-0.00645512973178214));
#51200=CARTESIAN_POINT('Ctrl Pts',(-0.0242425392407811,0.0108123291286123,
-0.00646436322293515));
#51201=CARTESIAN_POINT('Ctrl Pts',(-0.0242089312259155,0.0108251258562557,
-0.00647370735869068));
#51202=CARTESIAN_POINT('Ctrl Pts',(-0.024174459610266,0.010838108471594,
-0.00648337374583902));
#51203=CARTESIAN_POINT('Ctrl Pts',(-0.0240197131328595,0.0108963887103726,
-0.00652676710969123));
#51204=CARTESIAN_POINT('Ctrl Pts',(-0.0238475900116139,0.0109583780048465,
-0.00657681974123949));
#51205=CARTESIAN_POINT('Ctrl Pts',(-0.0236840952009517,0.0110132374264567,
-0.00662623310201612));
#51206=CARTESIAN_POINT('Ctrl Pts',(-0.023559442320716,0.0110550637381547,
-0.00666390718915064));
#51207=CARTESIAN_POINT('Ctrl Pts',(-0.02343984587656,0.0110929839294159,
-0.00670106327199141));
#51208=CARTESIAN_POINT('Ctrl Pts',(-0.0233211950613739,0.0111283428589419,
-0.00673881179428615));
#51209=CARTESIAN_POINT('Ctrl Pts',(-0.0232842233788922,0.0111393607277469,
-0.00675057426197967));
#51210=CARTESIAN_POINT('Ctrl Pts',(-0.0232473428984237,0.0111501264223963,
-0.00676239639079376));
#51211=CARTESIAN_POINT('Ctrl Pts',(-0.0232104306701419,0.011160684460551,
-0.00677431468288953));
#51212=CARTESIAN_POINT('Ctrl Pts',(-0.0230550584291699,0.0112051257236427,
-0.0068244815743961));
#51213=CARTESIAN_POINT('Ctrl Pts',(-0.0228991648663235,0.011246033504623,
-0.00687629484282091));
#51214=CARTESIAN_POINT('Ctrl Pts',(-0.0227355114221791,0.0112845271283102,
-0.00693227480508791));
#51215=CARTESIAN_POINT('Ctrl Pts',(-0.0225718579780346,0.0113230207519974,
-0.0069882547673549));
#51216=CARTESIAN_POINT('Ctrl Pts',(-0.0224004800995218,0.0113591090087216,
-0.00704849884169404));
#51217=CARTESIAN_POINT('Ctrl Pts',(-0.0222392771988294,0.0113895631001835,
-0.00710647929768051));
#51218=CARTESIAN_POINT('Ctrl Pts',(-0.0220780742981369,0.0114200171916454,
-0.00716445975366698));
#51219=CARTESIAN_POINT('Ctrl Pts',(-0.0219269954221904,0.0114448262895038,
-0.00722004153282126));
#51220=CARTESIAN_POINT('Ctrl Pts',(-0.0217673568540159,0.0114682300935694,
-0.00727984153866872));
#51221=CARTESIAN_POINT('Ctrl Pts',(-0.0216875375699287,0.0114799319956022,
-0.00730974154159246));
#51222=CARTESIAN_POINT('Ctrl Pts',(-0.021605583025283,0.0114912832570369,
-0.00734070775038529));
#51223=CARTESIAN_POINT('Ctrl Pts',(-0.0215184026942123,0.0115023523934568,
-0.00737397795079087));
#51224=CARTESIAN_POINT('Ctrl Pts',(-0.0214655245275965,0.0115090662431603,
-0.00739415758510492));
#51225=CARTESIAN_POINT('Ctrl Pts',(-0.0214107408238448,0.0115157425792275,
-0.00741518063249471));
#51226=CARTESIAN_POINT('Ctrl Pts',(-0.0213583486924787,0.0115218521168936,
-0.00743539184785046));
#51227=CARTESIAN_POINT('Ctrl Pts',(-0.0213243618199888,0.0115258153852741,
-0.00744850290062213));
#51228=CARTESIAN_POINT('Ctrl Pts',(-0.021291382533558,0.0115295445612725,
-0.00746127024107871));
#51229=CARTESIAN_POINT('Ctrl Pts',(-0.0212605955531625,0.0115329354582865,
-0.00747322299350472));
#51230=CARTESIAN_POINT('Ctrl Pts',(-0.0211639702187287,0.0115435778322313,
-0.00751073686091653));
#51231=CARTESIAN_POINT('Ctrl Pts',(-0.0210875286442459,0.0115512268304107,
-0.00754069354848727));
#51232=CARTESIAN_POINT('Ctrl Pts',(-0.0209983247349625,0.0115594801200226,
-0.00757590331316513));
#51233=CARTESIAN_POINT('Ctrl Pts',(-0.0208728650989734,0.0115710878479657,
-0.00762542361216579));
#51234=CARTESIAN_POINT('Ctrl Pts',(-0.0207377907557496,0.0115819903082155,
-0.00767933231628551));
#51235=CARTESIAN_POINT('Ctrl Pts',(-0.0206016312582355,0.0115913192905921,
-0.00773432223435744));
#51236=CARTESIAN_POINT('Ctrl Pts',(-0.0204234451009791,0.0116035277340071,
-0.00780628520695928));
#51237=CARTESIAN_POINT('Ctrl Pts',(-0.0202354512665399,0.0116136756292872,
-0.00788327400777926));
#51238=CARTESIAN_POINT('Ctrl Pts',(-0.0200394933157728,0.0116214249104022,
-0.00796472599078757));
#51239=CARTESIAN_POINT('Ctrl Pts',(-0.0199107219649714,0.0116265172549231,
-0.00801825115695901));
#51240=CARTESIAN_POINT('Ctrl Pts',(-0.0197826695329107,0.0116304803730488,
-0.00807194545716316));
#51241=CARTESIAN_POINT('Ctrl Pts',(-0.0196449142058159,0.0116335810938962,
-0.00813024414775876));
#51242=CARTESIAN_POINT('Ctrl Pts',(-0.0196207606883723,0.0116341247629989,
-0.00814046602788445));
#51243=CARTESIAN_POINT('Ctrl Pts',(-0.0195962052881846,0.0116346427084887,
-0.00815087403226374));
#51244=CARTESIAN_POINT('Ctrl Pts',(-0.0195711189395796,0.0116351346995956,
-0.00816152452180743));
#51245=CARTESIAN_POINT('Ctrl Pts',(-0.0194932364967061,0.0116366621227324,
-0.00819458976205108));
#51246=CARTESIAN_POINT('Ctrl Pts',(-0.0194102431613973,0.011637893906005,
-0.00823001122447739));
#51247=CARTESIAN_POINT('Ctrl Pts',(-0.0193375775331837,0.0116387231160456,
-0.00826116194303029));
#51248=CARTESIAN_POINT('Ctrl Pts',(-0.0193208662193722,0.0116389138140351,
-0.00826832584494639));
#51249=CARTESIAN_POINT('Ctrl Pts',(-0.0193047009403302,0.0116390852850543,
-0.00827526292998242));
#51250=CARTESIAN_POINT('Ctrl Pts',(-0.0192892688892072,0.0116392393051141,
-0.00828189123357834));
#51251=CARTESIAN_POINT('Ctrl Pts',(-0.0192067338142212,0.0116400630489629,
-0.00831734131924469));
#51252=CARTESIAN_POINT('Ctrl Pts',(-0.0191451581260807,0.0116403309325968,
-0.00834392987291784));
#51253=CARTESIAN_POINT('Ctrl Pts',(-0.0190762821376132,0.0116404432600024,
-0.00837376746968747));
#51254=CARTESIAN_POINT('Ctrl Pts',(-0.0190074061491457,0.011640555587408,
-0.0084036050664571));
#51255=CARTESIAN_POINT('Ctrl Pts',(-0.0189312438411869,0.011640467183901,
-0.00843672720352299));
#51256=CARTESIAN_POINT('Ctrl Pts',(-0.0188545740569457,0.0116400805608009,
-0.00847022736541512));
#51257=CARTESIAN_POINT('Ctrl Pts',(-0.0185478949199809,0.0116385340684007,
-0.00860422801298365));
#51258=CARTESIAN_POINT('Ctrl Pts',(-0.0182334449138913,0.0116327418153481,
-0.00874381723191419));
#51259=CARTESIAN_POINT('Ctrl Pts',(-0.0178774831716006,0.0116210616437134,
-0.00890496724854988));
#51260=CARTESIAN_POINT('Ctrl Pts',(-0.0176995023004553,0.011615221557896,
-0.00898554225686772));
#51261=CARTESIAN_POINT('Ctrl Pts',(-0.0175110655021848,0.0116077564505905,
-0.00907164313857367));
#51262=CARTESIAN_POINT('Ctrl Pts',(-0.0173323249853488,0.0115996854662668,
-0.00915403466834566));
#51263=CARTESIAN_POINT('Ctrl Pts',(-0.0173258280195924,0.0115993920973671,
-0.00915702948427783));
#51264=CARTESIAN_POINT('Ctrl Pts',(-0.0173193437858001,0.0115990978659295,
-0.00916001936559306));
#51265=CARTESIAN_POINT('Ctrl Pts',(-0.0173128720265079,0.0115988027869249,
-0.00916300441835151));
#51266=CARTESIAN_POINT('Ctrl Pts',(-0.016963249681542,0.0115828618025859,
-0.00932426522830298));
#51267=CARTESIAN_POINT('Ctrl Pts',(-0.0166501932368521,0.011564718427035,
-0.00947114780149651));
#51268=CARTESIAN_POINT('Ctrl Pts',(-0.0163378303803881,0.0115430555440284,
-0.009619580783559));
#51269=CARTESIAN_POINT('Ctrl Pts',(-0.0163272006767041,0.0115423183564193,
-0.00962463195588502));
#51270=CARTESIAN_POINT('Ctrl Pts',(-0.0163165717881284,0.0115415774297594,
-0.00962968513938956));
#51271=CARTESIAN_POINT('Ctrl Pts',(-0.0163059450208025,0.0115408327300449,
-0.00963473971397893));
#51272=CARTESIAN_POINT('Ctrl Pts',(-0.015998514756725,0.0115192887154964,
-0.00978096755102024));
#51273=CARTESIAN_POINT('Ctrl Pts',(-0.0156922675390135,0.0114944014941102,
-0.00992875512006374));
#51274=CARTESIAN_POINT('Ctrl Pts',(-0.0153993022433853,0.0114667765373308,
-0.0100716954734317));
#51275=CARTESIAN_POINT('Ctrl Pts',(-0.0153166543934544,0.0074999794584345,
-0.010121177809007));
#51276=CARTESIAN_POINT('Ctrl Pts',(-0.0153260430540535,0.00792901066112673,
-0.0101156468647559));
#51277=CARTESIAN_POINT('Ctrl Pts',(-0.015335030986271,0.00834507843141892,
-0.0101103306587591));
#51278=CARTESIAN_POINT('Ctrl Pts',(-0.0153436173262386,0.00874821533256098,
-0.0101052264670943));
#51279=CARTESIAN_POINT('Ctrl Pts',(-0.0153527877473525,0.00917877540402363,
-0.0100997750655438));
#51280=CARTESIAN_POINT('Ctrl Pts',(-0.0153615002389735,0.00959458555346814,
-0.010094565527106));
#51281=CARTESIAN_POINT('Ctrl Pts',(-0.0153697578474766,0.00999565020811485,
-0.0100895982399535));
#51282=CARTESIAN_POINT('Ctrl Pts',(-0.015378671278209,0.0104285675614914,
-0.0100842364490736));
#51283=CARTESIAN_POINT('Ctrl Pts',(-0.0153870543983629,0.0108443042696742,
-0.0100791569642583));
#51284=CARTESIAN_POINT('Ctrl Pts',(-0.015394903833982,0.0112428257310516,
-0.010074363848708));
#51285=CARTESIAN_POINT('Ctrl Pts',(-0.015396386273589,0.0113180902503411,
-0.0100734586238386));
#51286=CARTESIAN_POINT('Ctrl Pts',(-0.015397849684388,0.0113927406309423,
-0.0100725636187554));
#51287=CARTESIAN_POINT('Ctrl Pts',(-0.0153992941382262,0.0114667764973816,
-0.0100716788736061));
#51288=CARTESIAN_POINT('Ctrl Pts',(-0.0312862281526355,0.00944638107869527,
-0.00512344313018988));
#51289=CARTESIAN_POINT('Ctrl Pts',(-0.0314562756363666,0.00945826354092308,
-0.00509821111361097));
#51290=CARTESIAN_POINT('Ctrl Pts',(-0.0316300000451325,0.00947077019190787,
-0.00507294851419576));
#51291=CARTESIAN_POINT('Ctrl Pts',(-0.0318165997466437,0.00948464848780534,
-0.00504641821905065));
#51292=CARTESIAN_POINT('Ctrl Pts',(-0.0318632496720215,0.00948811806177971,
-0.00503978564526438));
#51293=CARTESIAN_POINT('Ctrl Pts',(-0.0319107047314941,0.00949167410932467,
-0.00503307702218328));
#51294=CARTESIAN_POINT('Ctrl Pts',(-0.0319555148891595,0.00949505711749807,
-0.00502677439109328));
#51295=CARTESIAN_POINT('Ctrl Pts',(-0.0320003250468249,0.00949844012567147,
-0.00502047176000328));
#51296=CARTESIAN_POINT('Ctrl Pts',(-0.0320424889665942,0.00950164756885702,
-0.00501456480075179));
#51297=CARTESIAN_POINT('Ctrl Pts',(-0.0320969589552305,0.00950581482965032,
-0.00500698754389991));
#51298=CARTESIAN_POINT('Ctrl Pts',(-0.032205898932503,0.0095141493512369,
-0.00499183303019616));
#51299=CARTESIAN_POINT('Ctrl Pts',(-0.032364079079264,0.00952635477605135,
-0.0049701229080083));
#51300=CARTESIAN_POINT('Ctrl Pts',(-0.0325078832619222,0.00953752434301051,
-0.00495080406393419));
#51301=CARTESIAN_POINT('Ctrl Pts',(-0.0326516874445805,0.00954869390996967,
-0.00493148521986007));
#51302=CARTESIAN_POINT('Ctrl Pts',(-0.0327811014399474,0.00955879432134487,
-0.00491443693059583));
#51303=CARTESIAN_POINT('Ctrl Pts',(-0.0329095981928218,0.00956888639698524,
-0.0048977528006591));
#51304=CARTESIAN_POINT('Ctrl Pts',(-0.0329276637186178,0.00957030525503992,
-0.00489540715710769));
#51305=CARTESIAN_POINT('Ctrl Pts',(-0.0329457110008698,0.00957172411000436,
-0.00489306911910923));
#51306=CARTESIAN_POINT('Ctrl Pts',(-0.0329637309158827,0.00957314220261207,
-0.00489073980242877));
#51307=CARTESIAN_POINT('Ctrl Pts',(-0.0330738833326562,0.00958181074116154,
-0.00487650111919418));
#51308=CARTESIAN_POINT('Ctrl Pts',(-0.0331830176598123,0.00959045057343606,
-0.00486259022841222));
#51309=CARTESIAN_POINT('Ctrl Pts',(-0.033289018186645,0.00959889021079495,
-0.00484924797714197));
#51310=CARTESIAN_POINT('Ctrl Pts',(-0.0335357006488678,0.00961853077849934,
-0.00481819813717152));
#51311=CARTESIAN_POINT('Ctrl Pts',(-0.0337654170511146,0.00963707680202003,
-0.00479020187725715));
#51312=CARTESIAN_POINT('Ctrl Pts',(-0.0339807978056659,0.00965465621567979,
-0.00476455503025098));
#51313=CARTESIAN_POINT('Ctrl Pts',(-0.0341961785602172,0.00967223562933955,
-0.0047389081832448));
#51314=CARTESIAN_POINT('Ctrl Pts',(-0.0343972246080754,0.00968885149610345,
-0.00471562001397164));
#51315=CARTESIAN_POINT('Ctrl Pts',(-0.0345829605600567,0.00970430948850187,
-0.00469454328516853));
#51316=CARTESIAN_POINT('Ctrl Pts',(-0.0347686965120379,0.00971976748090028,
-0.00467346655636542));
#51317=CARTESIAN_POINT('Ctrl Pts',(-0.0349391223186177,0.00973406623614095,
-0.00465459899770515));
#51318=CARTESIAN_POINT('Ctrl Pts',(-0.0350953496941226,0.00974715838514988,
-0.00463763982327587));
#51319=CARTESIAN_POINT('Ctrl Pts',(-0.0352515770696274,0.0097602505341588,
-0.00462068064884658));
#51320=CARTESIAN_POINT('Ctrl Pts',(-0.0353936065559122,0.00977213873693642,
-0.00460563662168135));
#51321=CARTESIAN_POINT('Ctrl Pts',(-0.0355178737630501,0.00978245291917888,
-0.00459271866193936));
#51322=CARTESIAN_POINT('Ctrl Pts',(-0.035642140970188,0.00979276710142133,
-0.00457980070219737));
#51323=CARTESIAN_POINT('Ctrl Pts',(-0.0357486448359685,0.00980150018491219,
-0.00456899286053882));
#51324=CARTESIAN_POINT('Ctrl Pts',(-0.0358504812553988,0.00980947077143243,
-0.0045589750680604));
#51325=CARTESIAN_POINT('Ctrl Pts',(-0.035901399465114,0.00981345606469256,
-0.00455396617182119));
#51326=CARTESIAN_POINT('Ctrl Pts',(-0.0359511514008514,0.00981725524023119,
-0.00454916449715817));
#51327=CARTESIAN_POINT('Ctrl Pts',(-0.0359830568732576,0.00981967355013075,
-0.00454610807859423));
#51328=CARTESIAN_POINT('Ctrl Pts',(-0.0359990096094606,0.00982088270508053,
-0.00454457986931226));
#51329=CARTESIAN_POINT('Ctrl Pts',(-0.036010500404943,0.00982174404162896,
-0.00454348243588464));
#51330=CARTESIAN_POINT('Ctrl Pts',(-0.0360409115717217,0.00982391760366982,
-0.00454065001146376));
#51331=CARTESIAN_POINT('Ctrl Pts',(-0.0360713227385004,0.00982609116571067,
-0.00453781758704287));
#51332=CARTESIAN_POINT('Ctrl Pts',(-0.0361206549855137,0.00982958271525947,
-0.00453326238401915));
#51333=CARTESIAN_POINT('Ctrl Pts',(-0.0361678405239929,0.00983286823482105,
-0.00452897731231815));
#51334=CARTESIAN_POINT('Ctrl Pts',(-0.0362622116009512,0.0098394392739442,
-0.00452040716891616));
#51335=CARTESIAN_POINT('Ctrl Pts',(-0.0363479935782716,0.00984516645782268,
-0.00451287649901968));
#51336=CARTESIAN_POINT('Ctrl Pts',(-0.0364361982614431,0.00985086055000014,
-0.00450536150740648));
#51337=CARTESIAN_POINT('Ctrl Pts',(-0.0365244029446146,0.00985655464217761,
-0.00449784651579328));
#51338=CARTESIAN_POINT('Ctrl Pts',(-0.0366150308907188,0.00986222133347914,
-0.00449035860128791));
#51339=CARTESIAN_POINT('Ctrl Pts',(-0.0367053796526332,0.0098676622596607,
-0.00448315369924367));
#51340=CARTESIAN_POINT('Ctrl Pts',(-0.0368860771764619,0.00987854411202381,
-0.00446874389515518));
#51341=CARTESIAN_POINT('Ctrl Pts',(-0.0370656574686301,0.00988851651328245,
-0.00445545394930328));
#51342=CARTESIAN_POINT('Ctrl Pts',(-0.0372462195336707,0.00989774443788289,
-0.00444316275356318));
#51343=CARTESIAN_POINT('Ctrl Pts',(-0.0374267815987114,0.00990697236248332,
-0.00443087155782307));
#51344=CARTESIAN_POINT('Ctrl Pts',(-0.037608325543134,0.00991545838883364,
-0.00441958371644594));
#51345=CARTESIAN_POINT('Ctrl Pts',(-0.0377903686107517,0.00992317554436644,
-0.00440939607922095));
#51346=CARTESIAN_POINT('Ctrl Pts',(-0.0385185405140091,0.00995404415093073,
-0.00436864555087132));
#51347=CARTESIAN_POINT('Ctrl Pts',(-0.0392547002352749,0.00997273853647701,
-0.00434575504846055));
#51348=CARTESIAN_POINT('Ctrl Pts',(-0.0399999969037804,0.00997686116634681,
-0.00434340405242746));
#51349=CARTESIAN_POINT('Origin',(-0.14,0.0075,0.));
#51350=CARTESIAN_POINT('',(-0.14,0.0075,-0.004));
#51351=CARTESIAN_POINT('Origin',(-0.14,0.0075,0.));
#51352=CARTESIAN_POINT('Origin',(-0.0475,0.0025,4.33680868994202E-19));
#51353=CARTESIAN_POINT('Ctrl Pts',(-0.0475,0.00292794117647059,0.00143766002569487));
#51354=CARTESIAN_POINT('Ctrl Pts',(-0.0475073233962253,0.00292794075855509,
0.00143766066444556));
#51355=CARTESIAN_POINT('Ctrl Pts',(-0.0475146468511719,0.00292791816889614,
0.00143760919648263));
#51356=CARTESIAN_POINT('Ctrl Pts',(-0.047521969610817,0.00292787381968359,
0.0014375057980809));
#51357=CARTESIAN_POINT('Origin',(-0.0675,0.0025,4.33680868994202E-19));
#51358=CARTESIAN_POINT('Ctrl Pts',(-0.0675,0.00292794117647059,0.00143766002569488));
#51359=CARTESIAN_POINT('Ctrl Pts',(-0.0675073233962253,0.00292794075855509,
0.00143766066444556));
#51360=CARTESIAN_POINT('Ctrl Pts',(-0.0675146468511718,0.00292791816889614,
0.00143760919648264));
#51361=CARTESIAN_POINT('Ctrl Pts',(-0.067521969610817,0.00292787381968359,
0.00143750579808091));
#51362=CARTESIAN_POINT('Origin',(-0.0875,0.0025,4.33680868994202E-19));
#51363=CARTESIAN_POINT('Ctrl Pts',(-0.0875,0.00292794117647059,0.00143766002569487));
#51364=CARTESIAN_POINT('Ctrl Pts',(-0.0875073233962253,0.00292794075855509,
0.00143766066444556));
#51365=CARTESIAN_POINT('Ctrl Pts',(-0.0875146468511718,0.00292791816889614,
0.00143760919648263));
#51366=CARTESIAN_POINT('Ctrl Pts',(-0.087521969610817,0.00292787381968359,
0.00143750579808091));
#51367=CARTESIAN_POINT('Origin',(-0.1075,0.0025,4.33680868994202E-19));
#51368=CARTESIAN_POINT('Ctrl Pts',(-0.1075,0.00292794117647059,0.00143766002569487));
#51369=CARTESIAN_POINT('Ctrl Pts',(-0.107507323396225,0.00292794075855509,
0.00143766066444556));
#51370=CARTESIAN_POINT('Ctrl Pts',(-0.107514646851172,0.00292791816889614,
0.00143760919648263));
#51371=CARTESIAN_POINT('Ctrl Pts',(-0.107521969610817,0.00292787381968359,
0.0014375057980809));
#51372=CARTESIAN_POINT('Origin',(-0.1275,0.0025,4.33680868994202E-19));
#51373=CARTESIAN_POINT('Ctrl Pts',(-0.1275,0.00292794117647059,0.00143766002569487));
#51374=CARTESIAN_POINT('Ctrl Pts',(-0.127507323396225,0.00292794075855509,
0.00143766066444555));
#51375=CARTESIAN_POINT('Ctrl Pts',(-0.127514646851172,0.00292791816889614,
0.00143760919648263));
#51376=CARTESIAN_POINT('Ctrl Pts',(-0.127521969610817,0.00292787381968359,
0.0014375057980809));
#51377=CARTESIAN_POINT('Origin',(0.00396253460616978,-0.0267643850402721,
0.));
#51378=CARTESIAN_POINT('',(-0.00847413551306003,0.0012,-0.00451935750764788));
#51379=CARTESIAN_POINT('',(-0.000426041560703257,0.0012,-0.0124834192096569));
#51380=CARTESIAN_POINT('Origin',(0.00396253460616978,0.0012,0.));
#51381=CARTESIAN_POINT('',(-0.000426041560703257,0.0128,-0.0124834192096569));
#51382=CARTESIAN_POINT('',(-0.000426041560703257,-0.0267643850402721,-0.0124834192096569));
#51383=CARTESIAN_POINT('',(-0.00847413551306003,0.0128,-0.00451935750764788));
#51384=CARTESIAN_POINT('Origin',(0.00396253460616978,0.0128,0.));
#51385=CARTESIAN_POINT('',(-0.00847413551306003,-0.0267643850402721,-0.00451935750764788));
#51386=CARTESIAN_POINT('Origin',(-0.00926982557395217,0.0172426406871193,
-0.003));
#51387=CARTESIAN_POINT('',(-0.0087336051435635,0.0128,-0.00440088102636655));
#51388=CARTESIAN_POINT('',(-0.0087336051435635,0.0172426406871193,-0.00440088102636655));
#51389=CARTESIAN_POINT('Origin',(-0.00926982557395217,0.0128,-0.003));
#51390=CARTESIAN_POINT('Origin',(-0.00926982557395217,0.0172426406871193,
0.003));
#51391=CARTESIAN_POINT('',(-0.0087336051435635,0.0128,0.00440088102636655));
#51392=CARTESIAN_POINT('Origin',(-0.00926982557395217,0.0128,0.003));
#51393=CARTESIAN_POINT('',(-0.0087336051435635,0.0172426406871193,0.00440088102636655));
#51394=CARTESIAN_POINT('Origin',(0.0125,0.0134,-4.59242549680257E-18));
#51395=CARTESIAN_POINT('',(-0.0218619061298847,0.0134036502117966,-0.00614822711587315));
#51396=CARTESIAN_POINT('',(-0.0246662622795289,0.0133985587966785,-0.00446937813281868));
#51397=CARTESIAN_POINT('Ctrl Pts',(-0.0218616087263876,0.0134072500816831,
-0.00614770820245367));
#51398=CARTESIAN_POINT('Ctrl Pts',(-0.0224316181952039,0.0134051358023753,
-0.00580540362823925));
#51399=CARTESIAN_POINT('Ctrl Pts',(-0.0229504127578444,0.0134033860935674,
-0.00549445185996141));
#51400=CARTESIAN_POINT('Ctrl Pts',(-0.0234178523021115,0.0134019533441035,
-0.00521477645854381));
#51401=CARTESIAN_POINT('Ctrl Pts',(-0.0238852918463787,0.0134005205946397,
-0.00493510105712622));
#51402=CARTESIAN_POINT('Ctrl Pts',(-0.0243013762672867,0.0133994057486489,
-0.00468670177378412));
#51403=CARTESIAN_POINT('Ctrl Pts',(-0.0246662622795289,0.0133985587966785,
-0.00446937813281868));
#51404=CARTESIAN_POINT('',(-0.0306437028537828,0.013404764132741,-0.000979164530978816));
#51405=CARTESIAN_POINT('Ctrl Pts',(-0.0246662622795289,0.0133985587966785,
-0.00446937813281868));
#51406=CARTESIAN_POINT('Ctrl Pts',(-0.02484870528565,0.0133981353206933,
-0.00436071631233596));
#51407=CARTESIAN_POINT('Ctrl Pts',(-0.0250183490525746,0.0133977787570224,
-0.00425982399334597));
#51408=CARTESIAN_POINT('Ctrl Pts',(-0.0251749322827964,0.0133974820191827,
-0.00416684462913048));
#51409=CARTESIAN_POINT('Ctrl Pts',(-0.0253315155130181,0.013397185281343,
-0.004073865264915));
#51410=CARTESIAN_POINT('Ctrl Pts',(-0.0254750382134319,0.0133969481647494,
-0.00398879886795332));
#51411=CARTESIAN_POINT('Ctrl Pts',(-0.0256065444454201,0.0133967612769716,
-0.00391103173174672));
#51412=CARTESIAN_POINT('Ctrl Pts',(-0.0257380506774083,0.0133965743891938,
-0.00383326459554012));
#51413=CARTESIAN_POINT('Ctrl Pts',(-0.0258575404382745,0.0133964384141437,
-0.00376279671161932));
#51414=CARTESIAN_POINT('Ctrl Pts',(-0.0259610836783824,0.013396345373031,
-0.00370191490119503));
#51415=CARTESIAN_POINT('Ctrl Pts',(-0.0260128552984361,0.0133962988524746,
-0.00367147399598301));
#51416=CARTESIAN_POINT('Ctrl Pts',(-0.026060640319222,0.0133962626606343,
-0.00364342966218188));
#51417=CARTESIAN_POINT('Ctrl Pts',(-0.0261094483981875,0.01339623361188,
-0.00361486343215608));
#51418=CARTESIAN_POINT('Ctrl Pts',(-0.0261216504179288,0.0133962263496915,
-0.0036077218746497));
#51419=CARTESIAN_POINT('Ctrl Pts',(-0.026133916378215,0.0133962195615091,
-0.00360054769753044));
#51420=CARTESIAN_POINT('Ctrl Pts',(-0.0261453683469057,0.0133962135826212,
-0.00359385233772909));
#51421=CARTESIAN_POINT('Ctrl Pts',(-0.0261568203155964,0.0133962076037333,
-0.00358715697792774));
#51422=CARTESIAN_POINT('Ctrl Pts',(-0.0261674582927879,0.0133962024308566,
-0.00358094043562296));
#51423=CARTESIAN_POINT('Ctrl Pts',(-0.026176404350354,0.0133961982804328,
-0.00357571415486204));
#51424=CARTESIAN_POINT('Ctrl Pts',(-0.0261942964654848,0.0133961899795853,
-0.00356526159334099));
#51425=CARTESIAN_POINT('Ctrl Pts',(-0.026205420924764,0.0133961850720793,
-0.00355877011808311));
#51426=CARTESIAN_POINT('Ctrl Pts',(-0.0262385426891691,0.0133961752170391,
-0.00353948251138114));
#51427=CARTESIAN_POINT('Ctrl Pts',(-0.0262716644535742,0.013396165361999,
-0.00352019490467917));
#51428=CARTESIAN_POINT('Ctrl Pts',(-0.0263267834553753,0.0133961525896145,
-0.00348811104702352));
#51429=CARTESIAN_POINT('Ctrl Pts',(-0.0263761483878874,0.0133961459372958,
-0.00345937581224427));
#51430=CARTESIAN_POINT('Ctrl Pts',(-0.0264255133203996,0.0133961392849771,
-0.00343064057746502));
#51431=CARTESIAN_POINT('Ctrl Pts',(-0.0264691242400881,0.0133961370250713,
-0.00340525406450762));
#51432=CARTESIAN_POINT('Ctrl Pts',(-0.0265137570553487,0.0133961377888301,
-0.00337927420988169));
#51433=CARTESIAN_POINT('Ctrl Pts',(-0.0266030226858698,0.0133961393163476,
-0.00332731450062983));
#51434=CARTESIAN_POINT('Ctrl Pts',(-0.0266963758413186,0.013396154777692,
-0.00327298132539457));
#51435=CARTESIAN_POINT('Ctrl Pts',(-0.0267889834642484,0.0133961847528988,
-0.00321908664941024));
#51436=CARTESIAN_POINT('Ctrl Pts',(-0.0269741987101078,0.0133962447033124,
-0.00311129729744156));
#51437=CARTESIAN_POINT('Ctrl Pts',(-0.0271564318922438,0.0133963600240961,
-0.00300526205486268));
#51438=CARTESIAN_POINT('Ctrl Pts',(-0.0273394739295583,0.0133965307135107,
-0.00289877688381003));
#51439=CARTESIAN_POINT('Ctrl Pts',(-0.0275225159668727,0.0133967014029252,
-0.00279229171275739));
#51440=CARTESIAN_POINT('Ctrl Pts',(-0.0277063668386704,0.0133969284195639,
-0.00268535658059987));
#51441=CARTESIAN_POINT('Ctrl Pts',(-0.0278900176482774,0.013397210548563,
-0.00257856036789178));
#51442=CARTESIAN_POINT('Ctrl Pts',(-0.0280736684578844,0.0133974926775621,
-0.00247176415518369));
#51443=CARTESIAN_POINT('Ctrl Pts',(-0.0282571192073703,0.0133978296700538,
-0.00236510686401149));
#51444=CARTESIAN_POINT('Ctrl Pts',(-0.0284406190592505,0.0133982212239526,
-0.00225844573750197));
#51445=CARTESIAN_POINT('Ctrl Pts',(-0.0288076187630104,0.0133990043317502,
-0.00204512348448318));
#51446=CARTESIAN_POINT('Ctrl Pts',(-0.0291748147033377,0.013400006110592,
-0.00183178560108586));
#51447=CARTESIAN_POINT('Ctrl Pts',(-0.0295420174056225,0.0134012198710319,
-0.0016185646073897));
#51448=CARTESIAN_POINT('Ctrl Pts',(-0.0299092201079074,0.0134024336314718,
-0.00140534361369354));
#51449=CARTESIAN_POINT('Ctrl Pts',(-0.0302764295548016,0.0134038593389672,
-0.00119223948020539));
#51450=CARTESIAN_POINT('Ctrl Pts',(-0.0306437239536334,0.0134054880398384,
-0.000979235456812336));
#51451=CARTESIAN_POINT('',(-0.0306436021829707,0.0134038303428005,0.000979384968266446));
#51452=CARTESIAN_POINT('Ctrl Pts',(-0.0306436988839239,0.0134001848071171,
-0.00097915009888143));
#51453=CARTESIAN_POINT('Ctrl Pts',(-0.0308844167416533,0.013400058464486,
-0.000838923509007557));
#51454=CARTESIAN_POINT('Ctrl Pts',(-0.031065303511043,0.0133999548660539,
-0.000605834760277834));
#51455=CARTESIAN_POINT('Ctrl Pts',(-0.0311468606481766,0.0133999055193688,
-0.000343687857538236));
#51456=CARTESIAN_POINT('Ctrl Pts',(-0.0311814513686478,0.0133998845900247,
-0.000232503839146404));
#51457=CARTESIAN_POINT('Ctrl Pts',(-0.0311988532204896,0.0133998706262688,
-0.000116311864112296));
#51458=CARTESIAN_POINT('Ctrl Pts',(-0.0311987881631695,0.013399869793343,
-2.04344619827451E-7));
#51459=CARTESIAN_POINT('Ctrl Pts',(-0.0311986370453371,0.0133998678585886,
0.000269495000961271));
#51460=CARTESIAN_POINT('Ctrl Pts',(-0.0311014259137929,0.0133999302301344,
0.00054031925079773));
#51461=CARTESIAN_POINT('Ctrl Pts',(-0.0309232168780912,0.0134000273529956,
0.000746743782210436));
#51462=CARTESIAN_POINT('Ctrl Pts',(-0.0308438164757785,0.0134000706257411,
0.000838715498329324));
#51463=CARTESIAN_POINT('Ctrl Pts',(-0.0307490092605827,0.0134001278742394,
0.000917856093433611));
#51464=CARTESIAN_POINT('Ctrl Pts',(-0.0306435804364503,0.0134001832092226,
0.00097927422772854));
#51465=CARTESIAN_POINT('',(-0.0245961457050751,0.0133984902066176,0.00450908869591151));
#51466=CARTESIAN_POINT('Ctrl Pts',(-0.030643579828093,0.0134054497566434,
0.000979354044147875));
#51467=CARTESIAN_POINT('Ctrl Pts',(-0.0302704345009344,0.0134038023831892,
0.00119668648055279));
#51468=CARTESIAN_POINT('Ctrl Pts',(-0.0298972641109317,0.0134023788653426,
0.00141392650844518));
#51469=CARTESIAN_POINT('Ctrl Pts',(-0.0295239969009407,0.0134011751550314,
0.00163111223813555));
#51470=CARTESIAN_POINT('Ctrl Pts',(-0.0291507239793726,0.0133999714263015,
0.00184830129111021));
#51471=CARTESIAN_POINT('Ctrl Pts',(-0.028777354208528,0.0133989876278009,
0.00206543600036375));
#51472=CARTESIAN_POINT('Ctrl Pts',(-0.0284040972083492,0.0133982196073921,
0.00228238672419007));
#51473=CARTESIAN_POINT('Ctrl Pts',(-0.0282174687082596,0.0133978355971879,
0.00239086208610336));
#51474=CARTESIAN_POINT('Ctrl Pts',(-0.0280308683699045,0.0133975054496782,
0.00249929139868863));
#51475=CARTESIAN_POINT('Ctrl Pts',(-0.02784402991443,0.0133972282005621,
0.00260782754683863));
#51476=CARTESIAN_POINT('Ctrl Pts',(-0.0276571914589556,0.013396950951446,
0.00271636369498863));
#51477=CARTESIAN_POINT('Ctrl Pts',(-0.0274701148862677,0.0133967268540346,
0.00282500668007215));
#51478=CARTESIAN_POINT('Ctrl Pts',(-0.0272838802758687,0.0133965560148374,
0.00293312914716413));
#51479=CARTESIAN_POINT('Ctrl Pts',(-0.0270976456654697,0.0133963851756403,
0.00304125161425611));
#51480=CARTESIAN_POINT('Ctrl Pts',(-0.0269122530287835,0.0133962666334186,
0.00314885357996413));
#51481=CARTESIAN_POINT('Ctrl Pts',(-0.026723644556908,0.0133961988639523,
0.00325828413831277));
#51482=CARTESIAN_POINT('Ctrl Pts',(-0.0266293403209695,0.0133961649792191,
0.00331299941748751));
#51483=CARTESIAN_POINT('Ctrl Pts',(-0.0265342321084859,0.0133961444583619,
0.00336817181498661));
#51484=CARTESIAN_POINT('Ctrl Pts',(-0.0264434931177796,0.0133961370186881,
0.00342080412543893));
#51485=CARTESIAN_POINT('Ctrl Pts',(-0.0263981236224262,0.0133961332988513,
0.00344712028066522));
#51486=CARTESIAN_POINT('Ctrl Pts',(-0.0263538464463589,0.0133961323911641,
0.00347280143798082));
#51487=CARTESIAN_POINT('Ctrl Pts',(-0.0263034087596331,0.0133961350177981,
0.00350204927193081));
#51488=CARTESIAN_POINT('Ctrl Pts',(-0.0262529710729073,0.0133961376444321,
0.00353129710588081));
#51489=CARTESIAN_POINT('Ctrl Pts',(-0.0261963728170893,0.0133961455241088,
0.00356411151466535));
#51490=CARTESIAN_POINT('Ctrl Pts',(-0.0261633185455084,0.0133961521945727,
0.00358328433450696));
#51491=CARTESIAN_POINT('Ctrl Pts',(-0.0261302642739275,0.0133961588650367,
0.00360245715434857));
#51492=CARTESIAN_POINT('Ctrl Pts',(-0.0261207540577249,0.013396162339358,
0.00360798850995018));
#51493=CARTESIAN_POINT('Ctrl Pts',(-0.0261040014070238,0.013396168779049,
0.00361774460599147));
#51494=CARTESIAN_POINT('Ctrl Pts',(-0.0260872487563228,0.0133961752187401,
0.00362750070203276));
#51495=CARTESIAN_POINT('Ctrl Pts',(-0.0260632536437238,0.0133961853949361,
0.003641481490354));
#51496=CARTESIAN_POINT('Ctrl Pts',(-0.0260395330951174,0.0133961977045661,
0.00365532466296406));
#51497=CARTESIAN_POINT('Ctrl Pts',(-0.0260336029579654,0.0133962007819736,
0.00365878545611685));
#51498=CARTESIAN_POINT('Ctrl Pts',(-0.0260276899814467,0.0133962039823826,
0.0036622376489649));
#51499=CARTESIAN_POINT('Ctrl Pts',(-0.0260217836934467,0.0133962073090115,
0.00366568731888552));
#51500=CARTESIAN_POINT('Ctrl Pts',(-0.0260166156914465,0.0133962102198117,
0.00366870578006609));
#51501=CARTESIAN_POINT('Ctrl Pts',(-0.0260114528103434,0.0133962132272588,
0.00367172230963));
#51502=CARTESIAN_POINT('Ctrl Pts',(-0.0260062880346306,0.0133962163339297,
0.00367474097893365));
#51503=CARTESIAN_POINT('Ctrl Pts',(-0.0259701346046417,0.0133962380806259,
0.00369587166405896));
#51504=CARTESIAN_POINT('Ctrl Pts',(-0.0259338883400778,0.0133962646035691,
0.00371710719892812));
#51505=CARTESIAN_POINT('Ctrl Pts',(-0.0258951429137755,0.0133962973664198,
0.00373984404161307));
#51506=CARTESIAN_POINT('Ctrl Pts',(-0.0257939303715984,0.0133963829510096,
0.00379923824291234));
#51507=CARTESIAN_POINT('Ctrl Pts',(-0.0256756638564315,0.0133965123590765,
0.00386887687484338));
#51508=CARTESIAN_POINT('Ctrl Pts',(-0.0255445494680514,0.0133966946948038,
0.00394632154718793));
#51509=CARTESIAN_POINT('Ctrl Pts',(-0.0254134350796713,0.0133968770305312,
0.00402376621953248));
#51510=CARTESIAN_POINT('Ctrl Pts',(-0.0252694728254696,0.0133971115725649,
0.00410901694869879));
#51511=CARTESIAN_POINT('Ctrl Pts',(-0.0251115451843419,0.0133974079443082,
0.00420272793954665));
#51512=CARTESIAN_POINT('Ctrl Pts',(-0.0249536175432143,0.0133977043160516,
0.00429643893039451));
#51513=CARTESIAN_POINT('Ctrl Pts',(-0.0247817245066117,0.0133980627385854,
0.00439861016754807));
#51514=CARTESIAN_POINT('Ctrl Pts',(-0.0245961457050751,0.0133984902066176,
0.00450908869591151));
#51515=CARTESIAN_POINT('',(-0.0217115430864154,0.013403672751003,0.00623566005618913));
#51516=CARTESIAN_POINT('Ctrl Pts',(-0.0245961457050751,0.0133984902066176,
0.00450908869591151));
#51517=CARTESIAN_POINT('Ctrl Pts',(-0.0242249881020029,0.0133993451426819,
0.00473004575263784));
#51518=CARTESIAN_POINT('Ctrl Pts',(-0.0237990859267062,0.0134004767238543,
0.00498422950764963));
#51519=CARTESIAN_POINT('Ctrl Pts',(-0.0233182712556556,0.0134019301764394,
0.00527185391241485));
#51520=CARTESIAN_POINT('Ctrl Pts',(-0.0228374565846051,0.0134033836290245,
0.00555947831718007));
#51521=CARTESIAN_POINT('Ctrl Pts',(-0.0223017296223626,0.0134051576682972,
0.00588054379428986));
#51522=CARTESIAN_POINT('Ctrl Pts',(-0.0217112388916228,0.0134072933313472,
0.00623513020576297));
#51523=CARTESIAN_POINT('',(-0.0196330755873382,0.013399961279499,0.00732918595449924));
#51524=CARTESIAN_POINT('Ctrl Pts',(-0.0217107156962388,0.0134,0.00623430285898128));
#51525=CARTESIAN_POINT('Ctrl Pts',(-0.0210382714245267,0.0134,0.00663741032810192));
#51526=CARTESIAN_POINT('Ctrl Pts',(-0.0203387252089173,0.0134,0.00698909350869522));
#51527=CARTESIAN_POINT('Ctrl Pts',(-0.0196330752480917,0.0134,0.00732918602429228));
#51528=CARTESIAN_POINT('',(-0.0170139362062251,0.0134,0.00887744578929155));
#51529=CARTESIAN_POINT('',(-0.0169180511005122,0.0134,0.00893412666903227));
#51530=CARTESIAN_POINT('',(-0.00395280707079757,0.0134,0.00203751601562436));
#51531=CARTESIAN_POINT('',(0.00979635300466746,0.0134,-0.0051627258920988));
#51532=CARTESIAN_POINT('',(-0.00395280707079757,0.0134,-0.00203751601562436));
#51533=CARTESIAN_POINT('Origin',(-0.00501982557395217,0.0134,-2.16840434497101E-19));
#51534=CARTESIAN_POINT('',(-0.0170139362062251,0.0134,-0.00887744578929154));
#51535=CARTESIAN_POINT('',(0.00979635300466746,0.0134,0.0051627258920988));
#51536=CARTESIAN_POINT('',(-0.0198053127327029,0.0133999927310859,-0.00722737050826749));
#51537=CARTESIAN_POINT('',(-0.021610272031846,0.0134,-0.00616039858740607));
#51538=CARTESIAN_POINT('Ctrl Pts',(-0.0198053128281438,0.0134,-0.0072273706664189));
#51539=CARTESIAN_POINT('Ctrl Pts',(-0.0205037791748502,0.0134,-0.00689234317033915));
#51540=CARTESIAN_POINT('Ctrl Pts',(-0.0211960792182919,0.0134,-0.00654557458054435));
#51541=CARTESIAN_POINT('Ctrl Pts',(-0.0218610959359586,0.0134,-0.00614689907887388));
#51542=CARTESIAN_POINT('',(-0.00501982557395217,0.0134,-0.0012));
#51543=CARTESIAN_POINT('Origin',(-0.00501982557395217,0.0134,-2.16840434497101E-19));
#51544=CARTESIAN_POINT('',(-0.00926982557395217,0.0134,-0.0025));
#51545=CARTESIAN_POINT('Origin',(-0.00926982557395217,0.0134,-0.003));
#51546=CARTESIAN_POINT('',(-0.00926982557395217,0.0134,0.0035));
#51547=CARTESIAN_POINT('Origin',(-0.00926982557395217,0.0134,0.003));
#51548=CARTESIAN_POINT('Origin',(-0.00501982557395217,-0.0233872477181734,
-2.16840434497101E-19));
#51549=CARTESIAN_POINT('',(-0.00386002285313196,0.0136,0.00221469132133082));
#51550=CARTESIAN_POINT('',(-0.00386002285313196,0.0148,0.00221469132133082));
#51551=CARTESIAN_POINT('',(-0.00386002285313196,-0.0233872477181734,0.00221469132133082));
#51552=CARTESIAN_POINT('',(-0.00386002285313196,0.0148,-0.00221469132133082));
#51553=CARTESIAN_POINT('Origin',(-0.00501982557395217,0.0148,-2.16840434497101E-19));
#51554=CARTESIAN_POINT('',(-0.00386002285313196,0.0136,-0.00221469132133082));
#51555=CARTESIAN_POINT('',(-0.00386002285313196,-0.0233872477181734,-0.00221469132133082));
#51556=CARTESIAN_POINT('Origin',(-0.00501982557395217,0.0136,-2.16840434497101E-19));
#51557=CARTESIAN_POINT('Origin',(-0.0170198255739522,-0.0233872477181734,
0.00910629506495907));
#51558=CARTESIAN_POINT('',(-0.016701694953409,0.0136,0.00893969452982874));
#51559=CARTESIAN_POINT('',(-0.016701694953409,0.0148,0.00893969452982874));
#51560=CARTESIAN_POINT('',(-0.016701694953409,-0.0233872477181734,0.00893969452982874));
#51561=CARTESIAN_POINT('',(-0.00386002285313196,0.0148,0.00221469132133081));
#51562=CARTESIAN_POINT('',(-0.0170198255739522,0.0136,0.00910629506495907));
#51563=CARTESIAN_POINT('Origin',(-0.0170198255739522,-0.0233872477181734,
-0.00910629506495906));
#51564=CARTESIAN_POINT('',(-0.016701694953409,0.0148,-0.00893969452982874));
#51565=CARTESIAN_POINT('',(-0.0170198255739522,0.0148,-0.00910629506495906));
#51566=CARTESIAN_POINT('',(-0.016701694953409,0.0136,-0.00893969452982874));
#51567=CARTESIAN_POINT('',(-0.016701694953409,-0.0233872477181734,-0.00893969452982874));
#51568=CARTESIAN_POINT('',(-0.0170198255739522,0.0136,-0.00910629506495906));
#51569=CARTESIAN_POINT('Ctrl Pts',(-0.0364455123647001,0.00340591076454288,
0.00292997690155913));
#51570=CARTESIAN_POINT('Ctrl Pts',(-0.0333747951719863,0.00232389768505854,
0.00146510792779752));
#51571=CARTESIAN_POINT('Ctrl Pts',(-0.030666089939513,3.24199491719774E-5,
0.00106768719154779));
#51572=CARTESIAN_POINT('Ctrl Pts',(-0.0362669964429192,0.00344366530354269,
0.00299137018949283));
#51573=CARTESIAN_POINT('Ctrl Pts',(-0.0331820842563904,0.00233996001538881,
0.00154459652507376));
#51574=CARTESIAN_POINT('Ctrl Pts',(-0.0304662723539453,3.26377421315948E-5,
0.0011853206571064));
#51575=CARTESIAN_POINT('Ctrl Pts',(-0.0359048356083394,0.00352223993193398,
0.00311624801154962));
#51576=CARTESIAN_POINT('Ctrl Pts',(-0.0327954167543044,0.00237267298125369,
0.00170402429165362));
#51577=CARTESIAN_POINT('Ctrl Pts',(-0.0300695591452557,3.30817301717868E-5,
0.00141885729043467));
#51578=CARTESIAN_POINT('Ctrl Pts',(-0.0353368818305699,0.00364968519670089,
0.00331160069857409));
#51579=CARTESIAN_POINT('Ctrl Pts',(-0.0322062130942011,0.00242275749036137,
0.00194751119469747));
#51580=CARTESIAN_POINT('Ctrl Pts',(-0.0294809352339733,3.37643438218347E-5,
0.00176534062295578));
#51581=CARTESIAN_POINT('Ctrl Pts',(-0.0347324273520965,0.00378725469799749,
0.00351789412330234));
#51582=CARTESIAN_POINT('Ctrl Pts',(-0.0316008826462354,0.00247324053409076,
0.0021994531946527));
#51583=CARTESIAN_POINT('Ctrl Pts',(-0.0288961484974036,3.44571825927306E-5,
0.00210954619418795));
#51584=CARTESIAN_POINT('Ctrl Pts',(-0.034185048803803,0.00391106611448223,
0.00370294412137096));
#51585=CARTESIAN_POINT('Ctrl Pts',(-0.0310754271943663,0.00251527669127259,
0.00242122290368142));
#51586=CARTESIAN_POINT('Ctrl Pts',(-0.0284093302761368,3.50404667023504E-5,
0.00239608347560846));
#51587=CARTESIAN_POINT('Ctrl Pts',(-0.0337092817698781,0.00401634422797446,
0.00386315824648985));
#51588=CARTESIAN_POINT('Ctrl Pts',(-0.0306359820359663,0.00254880604501725,
0.00261003824762744));
#51589=CARTESIAN_POINT('Ctrl Pts',(-0.0280183594648203,3.55115239250338E-5,
0.00262621551190547));
#51590=CARTESIAN_POINT('Ctrl Pts',(-0.0333296829265055,0.00409863588959051,
0.00399102434511768));
#51591=CARTESIAN_POINT('Ctrl Pts',(-0.0302949405967055,0.00257390378796406,
0.00275874528091764));
#51592=CARTESIAN_POINT('Ctrl Pts',(-0.0277240786605853,3.58677457098526E-5,
0.00279944354024005));
#51593=CARTESIAN_POINT('Ctrl Pts',(-0.0329218081184897,0.0041847120404232,
0.00412899533261083));
#51594=CARTESIAN_POINT('Ctrl Pts',(-0.0299393669415808,0.00259903849304822,
0.00291659451345235));
#51595=CARTESIAN_POINT('Ctrl Pts',(-0.0274278861496425,3.62288611593448E-5,
0.00297381181250567));
#51596=CARTESIAN_POINT('Ctrl Pts',(-0.0325522084676953,0.00426011777198721,
0.00425525216837874));
#51597=CARTESIAN_POINT('Ctrl Pts',(-0.0296275829358075,0.00262014249564209,
0.0030580312060908));
#51598=CARTESIAN_POINT('Ctrl Pts',(-0.0271786832862726,3.65364297070277E-5,
0.00312053589766483));
#51599=CARTESIAN_POINT('Ctrl Pts',(-0.0322332366460956,0.00432315291499516,
0.00436573860390773));
#51600=CARTESIAN_POINT('Ctrl Pts',(-0.0293659012756563,0.00263726882200995,
0.0031791299793348));
#51601=CARTESIAN_POINT('Ctrl Pts',(-0.0269772499404853,3.67891538465943E-5,
0.00323915086441261));
#51602=CARTESIAN_POINT('Ctrl Pts',(-0.0319804392227183,0.00437197070979676,
0.00445434196535493));
#51603=CARTESIAN_POINT('Ctrl Pts',(-0.0291625050568359,0.00265029366328149,
0.00327461785404188));
#51604=CARTESIAN_POINT('Ctrl Pts',(-0.02682493216657,3.69830684658742E-5,
0.00332885375602016));
#51605=CARTESIAN_POINT('Ctrl Pts',(-0.0317565244407999,0.00441413023968693,
0.00453399430810753));
#51606=CARTESIAN_POINT('Ctrl Pts',(-0.0289859845398002,0.0026613659398422,
0.00335880113672149));
#51607=CARTESIAN_POINT('Ctrl Pts',(-0.0266967639933256,3.71494125987322E-5,
0.00340434438765406));
#51608=CARTESIAN_POINT('Ctrl Pts',(-0.031567895438941,0.00444890207989184,
0.00460205596168863));
#51609=CARTESIAN_POINT('Ctrl Pts',(-0.0288397235658548,0.00267041177898812,
0.00342947624865893));
#51610=CARTESIAN_POINT('Ctrl Pts',(-0.0265933374933781,3.72862647502668E-5,
0.0034652694975214));
#51611=CARTESIAN_POINT('Ctrl Pts',(-0.0314211815457098,0.00447555725281909,
0.00465555130782646));
#51612=CARTESIAN_POINT('Ctrl Pts',(-0.0287272506203122,0.00267731062923309,
0.00348432164762575));
#51613=CARTESIAN_POINT('Ctrl Pts',(-0.0265152767808677,3.73911234432494E-5,
0.00351125648332721));
#51614=CARTESIAN_POINT('Ctrl Pts',(-0.0312686963284664,0.0045028342054351,
0.0047117935449501));
#51615=CARTESIAN_POINT('Ctrl Pts',(-0.0286117065954078,0.00268434106128931,
0.00354120125203931));
#51616=CARTESIAN_POINT('Ctrl Pts',(-0.0264366758557256,3.74984711339515E-5,
0.0035575661347842));
#51617=CARTESIAN_POINT('Ctrl Pts',(-0.0311096964982641,0.00453085160163887,
0.00477123004504529));
#51618=CARTESIAN_POINT('Ctrl Pts',(-0.0284926931804869,0.00269155560975046,
0.00360039129491648));
#51619=CARTESIAN_POINT('Ctrl Pts',(-0.0263574774216831,3.7609087124493E-5,
0.00360423290822119));
#51620=CARTESIAN_POINT('Ctrl Pts',(-0.0309713914373861,0.00455473602616356,
0.00482359862602796));
#51621=CARTESIAN_POINT('Ctrl Pts',(-0.0283904108244781,0.00269767648006451,
0.00365176307124788));
#51622=CARTESIAN_POINT('Ctrl Pts',(-0.0262909288458718,3.77033890942823E-5,
0.00364345014849943));
#51623=CARTESIAN_POINT('Ctrl Pts',(-0.0308561825197073,0.00457455485418223,
0.0048679434459117));
#51624=CARTESIAN_POINT('Ctrl Pts',(-0.0283061545418152,0.00270282781575326,
0.0036945215769936));
#51625=CARTESIAN_POINT('Ctrl Pts',(-0.0262373176226958,3.77828009240422E-5,
0.00367504736385796));
#51626=CARTESIAN_POINT('Ctrl Pts',(-0.030783451543195,0.00458653413502901,
0.00489576854994378));
#51627=CARTESIAN_POINT('Ctrl Pts',(-0.0282530896816562,0.00270580485141099,
0.00372142305380727));
#51628=CARTESIAN_POINT('Ctrl Pts',(-0.0262036563470202,3.78291696305176E-5,
0.00369488599018227));
#51629=CARTESIAN_POINT('Ctrl Pts',(-0.0307293296760956,0.0045962451598897,
0.0049174436794188));
#51630=CARTESIAN_POINT('Ctrl Pts',(-0.0282142654926756,0.00270852223581756,
0.00374156046938465));
#51631=CARTESIAN_POINT('Ctrl Pts',(-0.0261799863912769,3.78706614478648E-5,
0.00370884079396693));
#51632=CARTESIAN_POINT('Ctrl Pts',(-0.0307015264051103,0.00459992790810007,
0.00492738598974962));
#51633=CARTESIAN_POINT('Ctrl Pts',(-0.0281936909151507,0.00270914622671935,
0.00375170204460587));
#51634=CARTESIAN_POINT('Ctrl Pts',(-0.0261664601757535,3.78812763338712E-5,
0.00371680943126161));
#51635=CARTESIAN_POINT('Ctrl Pts',(-0.0306759785647499,0.00460670317667091,
0.00493977799715337));
#51636=CARTESIAN_POINT('Ctrl Pts',(-0.0281766044250891,0.002711744575781,
0.00376154458782346));
#51637=CARTESIAN_POINT('Ctrl Pts',(-0.0261579338285578,3.79191187909183E-5,
0.00372184690489322));
#51638=CARTESIAN_POINT('Ctrl Pts',(-0.0306739081276985,0.00460190391753511,
0.00493571878828618));
#51639=CARTESIAN_POINT('Ctrl Pts',(-0.0281724315802146,0.00270877101912153,
0.0037615151616685));
#51640=CARTESIAN_POINT('Ctrl Pts',(-0.0261512462899574,3.78780240191974E-5,
0.00372576551137767));
#51641=CARTESIAN_POINT('Ctrl Pts',(-0.0305817008950556,0.00464718206751526,
0.00500013630428141));
#51642=CARTESIAN_POINT('Ctrl Pts',(-0.028121665557071,0.00273053660259818,
0.00380025138698242));
#51643=CARTESIAN_POINT('Ctrl Pts',(-0.0261438777031298,3.81864845659119E-5,
0.00373024570056496));
#51644=CARTESIAN_POINT('Ctrl Pts',(-0.0304512352465178,0.00470705887529274,
0.00508932502427095));
#51645=CARTESIAN_POINT('Ctrl Pts',(-0.0280486526672015,0.00275918545777291,
0.00385443627071402));
#51646=CARTESIAN_POINT('Ctrl Pts',(-0.0261310958420302,3.8592713764993E-5,
0.0037379588375763));
#51647=CARTESIAN_POINT('Ctrl Pts',(-0.0302097657705172,0.00481654509266694,
0.00525862778588942));
#51648=CARTESIAN_POINT('Ctrl Pts',(-0.0279154643696936,0.00281236805077608,
0.00395458858415277));
#51649=CARTESIAN_POINT('Ctrl Pts',(-0.0261121862462621,3.93455240931729E-5,
0.0037494416009322));
#51650=CARTESIAN_POINT('Ctrl Pts',(-0.0298456573331352,0.0049707839105292,
0.00552107347107061));
#51651=CARTESIAN_POINT('Ctrl Pts',(-0.0277156005697513,0.00288931259523331,
0.0041046739806172));
#51652=CARTESIAN_POINT('Ctrl Pts',(-0.0260883721232669,4.04305341557616E-5,
0.00376397058687835));
#51653=CARTESIAN_POINT('Ctrl Pts',(-0.029294757673212,0.00518712242800417,
0.00593483822630104));
#51654=CARTESIAN_POINT('Ctrl Pts',(-0.0274151742246471,0.00300185665309095,
0.00433081235633842));
#51655=CARTESIAN_POINT('Ctrl Pts',(-0.0260624466832064,4.20073033700595E-5,
0.00377997647220182));
#51656=CARTESIAN_POINT('Ctrl Pts',(-0.0285524571140508,0.0054366086587878,
0.00654380090261184));
#51657=CARTESIAN_POINT('Ctrl Pts',(-0.027001949242104,0.00314768404954061,
0.00463992614113889));
#51658=CARTESIAN_POINT('Ctrl Pts',(-0.0260335236074697,4.401142030668E-5,
0.00379796151968866));
#51659=CARTESIAN_POINT('Ctrl Pts',(-0.0280809156183133,0.00556967658510273,
0.00696339051093119));
#51660=CARTESIAN_POINT('Ctrl Pts',(-0.0267268473930116,0.00323774605000878,
0.00484327138018103));
#51661=CARTESIAN_POINT('Ctrl Pts',(-0.0260064442295,4.52205599225896E-5,
0.00381451140871031));
#51662=CARTESIAN_POINT('Ctrl Pts',(-0.0277524351262434,0.00565354262612152,
0.00726569554266335));
#51663=CARTESIAN_POINT('Ctrl Pts',(-0.0265287908709839,0.0032993317982997,
0.00498871081272797));
#51664=CARTESIAN_POINT('Ctrl Pts',(-0.0259804809093425,4.60369483617543E-5,
0.00383023176033879));
#51665=CARTESIAN_POINT('Ctrl Pts',(-0.0274161511476627,0.00573049620110287,
0.00758476525177793));
#51666=CARTESIAN_POINT('Ctrl Pts',(-0.0263196182699441,0.00336105701133233,
0.00514148687082381));
#51667=CARTESIAN_POINT('Ctrl Pts',(-0.025946633572234,4.68447015644706E-5,
0.00385061772352051));
#51668=CARTESIAN_POINT('Ctrl Pts',(-0.027107213168873,0.00579088786390267,
0.00788764517379605));
#51669=CARTESIAN_POINT('Ctrl Pts',(-0.0261194595041263,0.00341582373363926,
0.00528685403998759));
#51670=CARTESIAN_POINT('Ctrl Pts',(-0.0259051879585585,4.75500473328697E-5,
0.00387546346390592));
#51671=CARTESIAN_POINT('Ctrl Pts',(-0.0268222191277561,0.00583771371380135,
0.00817407869531208));
#51672=CARTESIAN_POINT('Ctrl Pts',(-0.0259277666571967,0.00346424929736276,
0.00542562025819949));
#51673=CARTESIAN_POINT('Ctrl Pts',(-0.0258569234762942,4.8164363075934E-5,
0.00390431639822479));
#51674=CARTESIAN_POINT('Ctrl Pts',(-0.0265096649800296,0.00588051745048727,
0.00849409109638237));
#51675=CARTESIAN_POINT('Ctrl Pts',(-0.0257106286229303,0.00351508733799058,
0.00558256061587452));
#51676=CARTESIAN_POINT('Ctrl Pts',(-0.0257937198450575,4.88001461067806E-5,
0.00394203740391715));
#51677=CARTESIAN_POINT('Ctrl Pts',(-0.0261995682192878,0.00591132484202696,
0.00881840166566976));
#51678=CARTESIAN_POINT('Ctrl Pts',(-0.0254860437689506,0.00356200174806162,
0.00574482934744544));
#51679=CARTESIAN_POINT('Ctrl Pts',(-0.0257163416563158,4.93751853691084E-5,
0.00398814680952696));
#51680=CARTESIAN_POINT('Ctrl Pts',(-0.0257938698545106,0.00593627093979265,
0.00924940881465935));
#51681=CARTESIAN_POINT('Ctrl Pts',(-0.0251803962446941,0.0036180473812791,
0.00596617519969835));
#51682=CARTESIAN_POINT('Ctrl Pts',(-0.0255947569082474,5.00467832057705E-5,
0.00406052623970451));
#51683=CARTESIAN_POINT('Ctrl Pts',(-0.0253923226440449,0.00593971548210584,
0.00968302452453125));
#51684=CARTESIAN_POINT('Ctrl Pts',(-0.0248623974297738,0.00366536133344948,
0.00619779346020047));
#51685=CARTESIAN_POINT('Ctrl Pts',(-0.0254454981240691,5.05928833255763E-5,
0.00414930233341545));
#51686=CARTESIAN_POINT('Ctrl Pts',(-0.0249986734962245,0.00592312729945216,
0.0101112731277479));
#51687=CARTESIAN_POINT('Ctrl Pts',(-0.0245372400514592,0.00370302273718345,
0.00643685192505727));
#51688=CARTESIAN_POINT('Ctrl Pts',(-0.0252710108219186,5.10068228760653E-5,
0.00425303531907116));
#51689=CARTESIAN_POINT('Ctrl Pts',(-0.0246605209153862,0.00589409094509935,
0.0104799528591913));
#51690=CARTESIAN_POINT('Ctrl Pts',(-0.0242485447068516,0.00372845658143586,
0.00665116676847146));
#51691=CARTESIAN_POINT('Ctrl Pts',(-0.0250999117617437,5.1268439305896E-5,
0.00435472885127864));
#51692=CARTESIAN_POINT('Ctrl Pts',(-0.0243597776620712,0.00585707152211605,
0.0108072836977489));
#51693=CARTESIAN_POINT('Ctrl Pts',(-0.0239851571629279,0.00374548999173081,
0.0068485555891743));
#51694=CARTESIAN_POINT('Ctrl Pts',(-0.0249313947513967,5.14269322207653E-5,
0.00445487455205838));
#51695=CARTESIAN_POINT('Ctrl Pts',(-0.0239953492978759,0.0058002555009245,
0.0112023189097569));
#51696=CARTESIAN_POINT('Ctrl Pts',(-0.023659184141879,0.00375987256159987,
0.00709506282792327));
#51697=CARTESIAN_POINT('Ctrl Pts',(-0.0247094746225135,5.15372030271051E-5,
0.00458674636673381));
#51698=CARTESIAN_POINT('Ctrl Pts',(-0.0235913514326662,0.00571925070838247,
0.0116362329642894));
#51699=CARTESIAN_POINT('Ctrl Pts',(-0.0232884818635941,0.00376590220862389,
0.00737905762402919));
#51700=CARTESIAN_POINT('Ctrl Pts',(-0.0244363149918091,5.15321333879219E-5,
0.00474905568053847));
#51701=CARTESIAN_POINT('Ctrl Pts',(-0.023158991970489,0.0056129492390785,
0.0120931021922947));
#51702=CARTESIAN_POINT('Ctrl Pts',(-0.0228826498218856,0.00376066312518332,
0.0076944351282338));
#51703=CARTESIAN_POINT('Ctrl Pts',(-0.0241133983629133,5.13796891134259E-5,
0.00494092386423699));
#51704=CARTESIAN_POINT('Ctrl Pts',(-0.0226319129215638,0.00546354818217184,
0.012639550107198));
#51705=CARTESIAN_POINT('Ctrl Pts',(-0.0223791154247985,0.00374157039263029,
0.00809045414576035));
#51706=CARTESIAN_POINT('Ctrl Pts',(-0.0236876437050478,5.10365477415924E-5,
0.00519388996668408));
#51707=CARTESIAN_POINT('Ctrl Pts',(-0.0220427484603341,0.00526875827317497,
0.0132307259340806));
#51708=CARTESIAN_POINT('Ctrl Pts',(-0.0218054301955835,0.00370089266382102,
0.00854835534568239));
#51709=CARTESIAN_POINT('Ctrl Pts',(-0.0231644666249741,5.04164249423466E-5,
0.00550472954656049));
#51710=CARTESIAN_POINT('Ctrl Pts',(-0.0214022105896984,0.00503087002550459,
0.0138443682153251));
#51711=CARTESIAN_POINT('Ctrl Pts',(-0.0211724262978549,0.00363502645902371,
0.00905918822391987));
#51712=CARTESIAN_POINT('Ctrl Pts',(-0.0225455170232091,4.94807903072516E-5,
0.00587244025833354));
#51713=CARTESIAN_POINT('Ctrl Pts',(-0.0206076112485532,0.0047135341608338,
0.014569016759525));
#51714=CARTESIAN_POINT('Ctrl Pts',(-0.0203790291879768,0.00353078858065994,
0.00970228983916538));
#51715=CARTESIAN_POINT('Ctrl Pts',(-0.0217277835251736,4.80490545205933E-5,
0.00635818294222504));
#51716=CARTESIAN_POINT('Ctrl Pts',(-0.0200569456108525,0.00447901500725725,
0.01503294755748));
#51717=CARTESIAN_POINT('Ctrl Pts',(-0.01982337570409,0.00343879995533105,
0.0101515640080081));
#51718=CARTESIAN_POINT('Ctrl Pts',(-0.0211192082891102,4.68180167576593E-5,
0.00671958904311641));
#51719=CARTESIAN_POINT('Ctrl Pts',(-0.0196993664659313,0.00432573469918011,
0.0153197074216856));
#51720=CARTESIAN_POINT('Ctrl Pts',(-0.0194607362281236,0.00337353450158482,
0.0104416089908505));
#51721=CARTESIAN_POINT('Ctrl Pts',(-0.0207133290522096,4.59510186099511E-5,
0.00696056413499288));
#51722=CARTESIAN_POINT('',(-0.0307219745744663,7.95258423531978E-5,0.00107599969506516));
#51723=CARTESIAN_POINT('Origin',(-0.0367510524517764,-0.00895601651477296,
0.0114205245397328));
#51724=CARTESIAN_POINT('',(-0.0262191092076098,0.00012427284417193,0.0037259611256264));
#51725=CARTESIAN_POINT('Ctrl Pts',(-0.0307219740115217,7.95260984898368E-5,
0.00107600024689227));
#51726=CARTESIAN_POINT('Ctrl Pts',(-0.0305252572528752,8.13345891118369E-5,
0.00119223192931586));
#51727=CARTESIAN_POINT('Ctrl Pts',(-0.0303284251623317,8.32609267468997E-5,
0.00130852983035956));
#51728=CARTESIAN_POINT('Ctrl Pts',(-0.0301316153384272,8.52758354696813E-5,
0.00142477868099659));
#51729=CARTESIAN_POINT('Ctrl Pts',(-0.0299369158857927,8.72691385358141E-5,
0.00153978100730014));
#51730=CARTESIAN_POINT('Ctrl Pts',(-0.0297422370116984,8.93491181379123E-5,
0.00165473599950342));
#51731=CARTESIAN_POINT('Ctrl Pts',(-0.0295476067310188,9.14849303570787E-5,
0.00176960141917011));
#51732=CARTESIAN_POINT('Ctrl Pts',(-0.0293540301943859,9.36091791165256E-5,
0.00188384494818485));
#51733=CARTESIAN_POINT('Ctrl Pts',(-0.0291605002719552,9.57886356598487E-5,
0.00199800069131126));
#51734=CARTESIAN_POINT('Ctrl Pts',(-0.028966900823677,9.79911655836168E-5,
0.00211212007243703));
#51735=CARTESIAN_POINT('Ctrl Pts',(-0.0288820222035214,9.895680728582E-5,
0.00216215273363064));
#51736=CARTESIAN_POINT('Ctrl Pts',(-0.028797129948477,9.99268420874477E-5,
0.00221217864547998));
#51737=CARTESIAN_POINT('Ctrl Pts',(-0.0287122065938775,0.00010089857280184,
0.0022622074254998));
#51738=CARTESIAN_POINT('Ctrl Pts',(-0.0286036039689568,0.000102141252236687,
0.00232618578407208));
#51739=CARTESIAN_POINT('Ctrl Pts',(-0.0284947741845346,0.000103390112473951,
0.0023902735069483));
#51740=CARTESIAN_POINT('Ctrl Pts',(-0.0283858420771839,0.000104631353219126,
0.00245439234151685));
#51741=CARTESIAN_POINT('Ctrl Pts',(-0.028288569628719,0.000105739736498895,
0.00251164815142346));
#51742=CARTESIAN_POINT('Ctrl Pts',(-0.0281912154713187,0.000106842034320342,
0.00256892885933081));
#51743=CARTESIAN_POINT('Ctrl Pts',(-0.0280938961439213,0.000107928199043347,
0.00262616431261735));
#51744=CARTESIAN_POINT('Ctrl Pts',(-0.0279959851842882,0.000109020966874701,
0.00268374771671787));
#51745=CARTESIAN_POINT('Ctrl Pts',(-0.0278981088942278,0.000110097405311395,
0.00274128566927246));
#51746=CARTESIAN_POINT('Ctrl Pts',(-0.027800296460405,0.000111147477837171,
0.00279876033041972));
#51747=CARTESIAN_POINT('Ctrl Pts',(-0.0277014984804252,0.000112208130765682,
0.00285681409924481));
#51748=CARTESIAN_POINT('Ctrl Pts',(-0.0276027651039974,0.000113241889062903,
0.00291480362867732));
#51749=CARTESIAN_POINT('Ctrl Pts',(-0.0275041250658499,0.000114238488510968,
0.0029727129547738));
#51750=CARTESIAN_POINT('Ctrl Pts',(-0.0274040669501753,0.000115249415359015,
0.00303145480197922));
#51751=CARTESIAN_POINT('Ctrl Pts',(-0.0273041037905599,0.000116222120639044,
0.00309011478667495));
#51752=CARTESIAN_POINT('Ctrl Pts',(-0.0272042255891732,0.000117146481370503,
0.00314870161633757));
#51753=CARTESIAN_POINT('Ctrl Pts',(-0.0271536039826784,0.000117614978245272,
0.00317839537729622));
#51754=CARTESIAN_POINT('Ctrl Pts',(-0.0271030047169357,0.000118071045377641,
0.0032080700472859));
#51755=CARTESIAN_POINT('Ctrl Pts',(-0.0270524214565589,0.00011851347969458,
0.00323772994986223));
#51756=CARTESIAN_POINT('Ctrl Pts',(-0.0270012925077992,0.000118960686959428,
0.00326770982122177));
#51757=CARTESIAN_POINT('Ctrl Pts',(-0.0269501798413928,0.000119393967140987,
0.00329767464809863));
#51758=CARTESIAN_POINT('Ctrl Pts',(-0.0268990741911264,0.000119812157868954,
0.00332763063128599));
#51759=CARTESIAN_POINT('Ctrl Pts',(-0.0268473465297388,0.000120235438431063,
0.00335795121123693));
#51760=CARTESIAN_POINT('Ctrl Pts',(-0.0267956259413342,0.000120643262574798,
0.00338826280173099));
#51761=CARTESIAN_POINT('Ctrl Pts',(-0.0267438961144647,0.000121034609501203,
0.00341857601094203));
#51762=CARTESIAN_POINT('Ctrl Pts',(-0.0267177717553492,0.000121232245725077,
0.00343388464836257));
#51763=CARTESIAN_POINT('Ctrl Pts',(-0.0266916451290816,0.000121425677806561,
0.00344919364504706));
#51764=CARTESIAN_POINT('Ctrl Pts',(-0.026665513235662,0.000121614815219698,
0.0034645049316798));
#51765=CARTESIAN_POINT('Ctrl Pts',(-0.0266391931547748,0.000121805314696052,
0.00347992648174471));
#51766=CARTESIAN_POINT('Ctrl Pts',(-0.0266128677255237,0.000121991457392134,
0.00349535035792513));
#51767=CARTESIAN_POINT('Ctrl Pts',(-0.0265865335877925,0.000122173105607934,
0.00351077869403059));
#51768=CARTESIAN_POINT('Ctrl Pts',(-0.0265599989071751,0.000122356137133028,
0.00352632452185281));
#51769=CARTESIAN_POINT('Ctrl Pts',(-0.0265334553754045,0.000122534606498225,
0.00354187488399971));
#51770=CARTESIAN_POINT('Ctrl Pts',(-0.0265068982539826,0.000122708637195116,
0.00355743286379766));
#51771=CARTESIAN_POINT('Ctrl Pts',(-0.0264801273676615,0.000122884068708525,
0.00357311607365837));
#51772=CARTESIAN_POINT('Ctrl Pts',(-0.0264533426686387,0.000123054986866343,
0.00358880702510529));
#51773=CARTESIAN_POINT('Ctrl Pts',(-0.0264265400040283,0.000123220680241195,
0.00360450809544571));
#51774=CARTESIAN_POINT('Ctrl Pts',(-0.0264151459496129,0.000123291117988962,
0.00361118276202975));
#51775=CARTESIAN_POINT('Ctrl Pts',(-0.0264037486565156,0.000123360612090243,
0.00361785925271107));
#51776=CARTESIAN_POINT('Ctrl Pts',(-0.0263923472133218,0.000123429359989684,
0.00362453821571575));
#51777=CARTESIAN_POINT('Ctrl Pts',(-0.0263767145458341,0.000123523621131379,
0.00363369582901427));
#51778=CARTESIAN_POINT('Ctrl Pts',(-0.0263610595312741,0.000123628241621857,
0.00364287217015774));
#51779=CARTESIAN_POINT('Ctrl Pts',(-0.0263454005924302,0.000123732914342874,
0.0036520516001013));
#51780=CARTESIAN_POINT('Ctrl Pts',(-0.0263317686235584,0.000123824037712654,
0.00366004279953693));
#51781=CARTESIAN_POINT('Ctrl Pts',(-0.0263181337153121,0.000123915187696385,
0.00366803631562752));
#51782=CARTESIAN_POINT('Ctrl Pts',(-0.0263045153126929,0.000123995921902339,
0.00367601595328584));
#51783=CARTESIAN_POINT('Ctrl Pts',(-0.0262907854281113,0.000124077317008691,
0.00368406091326504));
#51784=CARTESIAN_POINT('Ctrl Pts',(-0.0262770721649393,0.000124148203574728,
0.0036920918942593));
#51785=CARTESIAN_POINT('Ctrl Pts',(-0.0262633646773175,0.000124214468613312,
0.00370011806415441));
#51786=CARTESIAN_POINT('Ctrl Pts',(-0.0262564551243315,0.000124247870926547,
0.00370416382714869));
#51787=CARTESIAN_POINT('Ctrl Pts',(-0.026249547190954,0.000124280025057016,
0.00370820824545637));
#51788=CARTESIAN_POINT('Ctrl Pts',(-0.0262426750462274,0.0001242928932531,
0.00371222298187236));
#51789=CARTESIAN_POINT('Ctrl Pts',(-0.0262376653489532,0.00012430227398785,
0.00371514966850082));
#51790=CARTESIAN_POINT('Ctrl Pts',(-0.0262326274393708,0.000124326403532759,
0.00371809980664705));
#51791=CARTESIAN_POINT('Ctrl Pts',(-0.0262275856449859,0.000124352433508816,
0.00372105321361447));
#51792=CARTESIAN_POINT('Ctrl Pts',(-0.026224665565161,0.000124367509412776,
0.00372276375225252));
#51793=CARTESIAN_POINT('Ctrl Pts',(-0.0262220357872776,0.000124236843468986,
0.00372423694144539));
#51794=CARTESIAN_POINT('Ctrl Pts',(-0.0262191092076098,0.00012427284417193,
0.0037259611256264));
#51795=CARTESIAN_POINT('',(-0.0207569920523634,8.45301690043879E-5,0.0069665043144839));
#51796=CARTESIAN_POINT('Ctrl Pts',(-0.0262191092076098,0.00012427284417193,
0.0037259611256264));
#51797=CARTESIAN_POINT('Ctrl Pts',(-0.026218313252602,0.000124257642349168,
0.00372641839465707));
#51798=CARTESIAN_POINT('Ctrl Pts',(-0.0262174583909347,0.000124274509407832,
0.00372692500192157));
#51799=CARTESIAN_POINT('Ctrl Pts',(-0.0262165687577017,0.000124310605772055,
0.00372746087457822));
#51800=CARTESIAN_POINT('Ctrl Pts',(-0.0262104887075549,0.000124557300360844,
0.00373112320699108));
#51801=CARTESIAN_POINT('Ctrl Pts',(-0.026203466830604,0.000125314347699211,
0.00373557411719657));
#51802=CARTESIAN_POINT('Ctrl Pts',(-0.0261971149797945,0.000125703392451664,
0.00373946416591847));
#51803=CARTESIAN_POINT('Ctrl Pts',(-0.0261877584649919,0.000126276469983611,
0.00374519435378668));
#51804=CARTESIAN_POINT('Ctrl Pts',(-0.0261784184200931,0.000126837975953154,
0.00375091282474766));
#51805=CARTESIAN_POINT('Ctrl Pts',(-0.0261691966518907,0.00012731559893701,
0.00375652714292099));
#51806=CARTESIAN_POINT('Ctrl Pts',(-0.0261588155943136,0.000127853264988325,
0.00376284724975233));
#51807=CARTESIAN_POINT('Ctrl Pts',(-0.0261485536193207,0.00012829898441606,
0.00376906010303047));
#51808=CARTESIAN_POINT('Ctrl Pts',(-0.0261380673911856,0.000128789974380921,
0.00377543129488929));
#51809=CARTESIAN_POINT('Ctrl Pts',(-0.0261262956103143,0.000129341156960766,
0.00378258355912431));
#51810=CARTESIAN_POINT('Ctrl Pts',(-0.0261142716574951,0.000129932778179259,
0.00378991014955548));
#51811=CARTESIAN_POINT('Ctrl Pts',(-0.0261019504193946,0.000130510114165908,
0.00379741689306796));
#51812=CARTESIAN_POINT('Ctrl Pts',(-0.0260883874996105,0.000131145631604298,
0.00380568013408884));
#51813=CARTESIAN_POINT('Ctrl Pts',(-0.0260745686731552,0.0001317384880603,
0.00381408777172032));
#51814=CARTESIAN_POINT('Ctrl Pts',(-0.0260621770610233,0.000131810391501782,
0.0038214233342845));
#51815=CARTESIAN_POINT('Ctrl Pts',(-0.026049122476854,0.00013188614189801,
0.00382915136175217));
#51816=CARTESIAN_POINT('Ctrl Pts',(-0.0260375247560911,0.000131425149614633,
0.00383578351186937));
#51817=CARTESIAN_POINT('Ctrl Pts',(-0.0260264852753561,0.000130800874521038,
0.00384201505075769));
#51818=CARTESIAN_POINT('Ctrl Pts',(-0.0260155572388606,0.000130182901523054,
0.00384818368187621));
#51819=CARTESIAN_POINT('Ctrl Pts',(-0.0260051922966206,0.000129397723389961,
0.00385394717785739));
#51820=CARTESIAN_POINT('Ctrl Pts',(-0.0259948301686768,0.000128635554659348,
0.00385972339426267));
#51821=CARTESIAN_POINT('Ctrl Pts',(-0.0259851541880192,0.000127923854327597,
0.00386511712791609));
#51822=CARTESIAN_POINT('Ctrl Pts',(-0.0259754844107568,0.00012723076004095,
0.00387051909059551));
#51823=CARTESIAN_POINT('Ctrl Pts',(-0.0259655001182173,0.000126665520066985,
0.00387616921576119));
#51824=CARTESIAN_POINT('Ctrl Pts',(-0.0259504486967768,0.00012581341512019,
0.00388468683628603));
#51825=CARTESIAN_POINT('Ctrl Pts',(-0.0259346753191958,0.000125251151555231,
0.00389377221539224));
#51826=CARTESIAN_POINT('Ctrl Pts',(-0.0259174185138597,0.000125266953211752,
0.00390401171199071));
#51827=CARTESIAN_POINT('Ctrl Pts',(-0.0258978752943211,0.000125284848484745,
0.0039156078751328));
#51828=CARTESIAN_POINT('Ctrl Pts',(-0.025878398121216,0.000125281820980013,
0.00392716302802724));
#51829=CARTESIAN_POINT('Ctrl Pts',(-0.0258588900120178,0.000125282028506469,
0.00393874416856717));
#51830=CARTESIAN_POINT('Ctrl Pts',(-0.0258422233954665,0.000125282205805246,
0.00394863843492812));
#51831=CARTESIAN_POINT('Ctrl Pts',(-0.0258255312581991,0.000125284518560359,
0.00395855330740935));
#51832=CARTESIAN_POINT('Ctrl Pts',(-0.0258088207793041,0.000125289424603215,
0.00396848398787762));
#51833=CARTESIAN_POINT('Ctrl Pts',(-0.0257840514799041,0.000125296696641624,
0.00398320385313759));
#51834=CARTESIAN_POINT('Ctrl Pts',(-0.0257592419786764,0.000125309797834037,
0.00399795849075353));
#51835=CARTESIAN_POINT('Ctrl Pts',(-0.0257345055512984,0.000125296226632468,
0.00401266387494284));
#51836=CARTESIAN_POINT('Ctrl Pts',(-0.0257269516828363,0.000125292082336691,
0.00401715452091017));
#51837=CARTESIAN_POINT('Ctrl Pts',(-0.025719414317235,0.000125283071607205,
0.00402163368790882));
#51838=CARTESIAN_POINT('Ctrl Pts',(-0.0257118899152836,0.000125270118788965,
0.00402610384659461));
#51839=CARTESIAN_POINT('Ctrl Pts',(-0.0256803268705193,0.000125215784851918,
0.00404485508019595));
#51840=CARTESIAN_POINT('Ctrl Pts',(-0.0256489924869321,0.000125092034389544,
0.00406344745792039));
#51841=CARTESIAN_POINT('Ctrl Pts',(-0.0256177491731015,0.000124927750833351,
0.00408197378525708));
#51842=CARTESIAN_POINT('Ctrl Pts',(-0.0255564195001067,0.000124605267218635,
0.00411834040127974));
#51843=CARTESIAN_POINT('Ctrl Pts',(-0.0254954377548005,0.000124126490117409,
0.0041544542529373));
#51844=CARTESIAN_POINT('Ctrl Pts',(-0.0254347581974083,0.000123584215385121,
0.00419037491538026));
#51845=CARTESIAN_POINT('Ctrl Pts',(-0.0253754594351541,0.000123054280398638,
0.00422547818431893));
#51846=CARTESIAN_POINT('Ctrl Pts',(-0.0253164521623267,0.000122463921329405,
0.00426039531471784));
#51847=CARTESIAN_POINT('Ctrl Pts',(-0.0252575344012696,0.000121847452620448,
0.00429525749972636));
#51848=CARTESIAN_POINT('Ctrl Pts',(-0.0251998379772801,0.000121243763013611,
0.00432939700827802));
#51849=CARTESIAN_POINT('Ctrl Pts',(-0.0251422265861802,0.000120615089204082,
0.00436348431978858));
#51850=CARTESIAN_POINT('Ctrl Pts',(-0.0250845856810912,0.00011997913229085,
0.00439759301155981));
#51851=CARTESIAN_POINT('Ctrl Pts',(-0.0250280357281178,0.000119355211943296,
0.00443105613835619));
#51852=CARTESIAN_POINT('Ctrl Pts',(-0.0249714568511407,0.000118724306895247,
0.00446454015753084));
#51853=CARTESIAN_POINT('Ctrl Pts',(-0.0249147917049414,0.000118095225489086,
0.0044980816054591));
#51854=CARTESIAN_POINT('Ctrl Pts',(-0.0248591073634841,0.000117477032716725,
0.00453104249173021));
#51855=CARTESIAN_POINT('Ctrl Pts',(-0.0248033395066288,0.000116860609546021,
0.0045640589607905));
#51856=CARTESIAN_POINT('Ctrl Pts',(-0.0247474512262175,0.000116251253002794,
0.00459715428310829));
#51857=CARTESIAN_POINT('Ctrl Pts',(-0.0246382440577773,0.000115060554305916,
0.00466182341252776));
#51858=CARTESIAN_POINT('Ctrl Pts',(-0.0245285801009226,0.000113896810116591,
0.0047267918768944));
#51859=CARTESIAN_POINT('Ctrl Pts',(-0.0244183518607806,0.000112776485805999,
0.00479212631922648));
#51860=CARTESIAN_POINT('Ctrl Pts',(-0.0243110402029364,0.000111685804697981,
0.00485573204596173));
#51861=CARTESIAN_POINT('Ctrl Pts',(-0.0242031919125816,0.000110636321447355,
0.00491968572852661));
#51862=CARTESIAN_POINT('Ctrl Pts',(-0.0240947885822766,0.000109629476930135,
0.00498399669551821));
#51863=CARTESIAN_POINT('Ctrl Pts',(-0.0239887863865853,0.000108644934026843,
0.00504688317408824));
#51864=CARTESIAN_POINT('Ctrl Pts',(-0.0238822510031491,0.000107701166320274,
0.00511011274960858));
#51865=CARTESIAN_POINT('Ctrl Pts',(-0.0237753609545318,0.000106795374651794,
0.00517357556253613));
#51866=CARTESIAN_POINT('Ctrl Pts',(-0.0235670917864745,0.00010503049120691,
0.00529722923677397));
#51867=CARTESIAN_POINT('Ctrl Pts',(-0.0233574948382918,0.000103409482345986,
0.00542175804479225));
#51868=CARTESIAN_POINT('Ctrl Pts',(-0.0231469207294679,0.00010187771712088,
0.00554691553928123));
#51869=CARTESIAN_POINT('Ctrl Pts',(-0.0229414037745486,0.000100382738813845,
0.00566906724775274));
#51870=CARTESIAN_POINT('Ctrl Pts',(-0.0227349470379256,9.89726889956665E-5,
0.0057918231121365));
#51871=CARTESIAN_POINT('Ctrl Pts',(-0.0225281333326472,9.75825445919448E-5,
0.00591478789175411));
#51872=CARTESIAN_POINT('Ctrl Pts',(-0.02232403982328,9.6210684591173E-5,
0.00603613533034356));
#51873=CARTESIAN_POINT('Ctrl Pts',(-0.0221195951197529,9.48581312153604E-5,
0.00615768826359034));
#51874=CARTESIAN_POINT('Ctrl Pts',(-0.0219154123534245,9.34628299006657E-5,
0.00627902490392014));
#51875=CARTESIAN_POINT('Ctrl Pts',(-0.0215266328754144,9.08060703388838E-5,
0.00651005907266608));
#51876=CARTESIAN_POINT('Ctrl Pts',(-0.021138800462131,8.79873584830102E-5,
0.00674031620404643));
#51877=CARTESIAN_POINT('Ctrl Pts',(-0.0207569064093787,8.46249031451449E-5,
0.00696634980021813));
#51878=CARTESIAN_POINT('Ctrl Pts',(-0.0207569920523634,8.45301690043879E-5,
0.0069665043144839));
#51879=CARTESIAN_POINT('Ctrl Pts',(-0.0210089319175918,0.000156447471720346,
0.00687493731751199));
#51880=CARTESIAN_POINT('Ctrl Pts',(-0.0212588640564334,0.000233847770492934,
0.00678509563754937));
#51881=CARTESIAN_POINT('Ctrl Pts',(-0.0215066257862298,0.000317179867387291,
0.00669685818551664));
#51882=CARTESIAN_POINT('Ctrl Pts',(-0.0217186243241269,0.000388483384342961,
0.00662135737740526));
#51883=CARTESIAN_POINT('Ctrl Pts',(-0.0219289662434665,0.000464028822881538,
0.00654699979756583));
#51884=CARTESIAN_POINT('Ctrl Pts',(-0.0221376399317455,0.000544631803685119,
0.00647399888350404));
#51885=CARTESIAN_POINT('Ctrl Pts',(-0.0222947802331561,0.000605329330060039,
0.00641902604177432));
#51886=CARTESIAN_POINT('Ctrl Pts',(-0.0224509733069686,0.000668898321367291,
0.0063648219031823));
#51887=CARTESIAN_POINT('Ctrl Pts',(-0.0226062016136997,0.00073503623390973,
0.00631153256380226));
#51888=CARTESIAN_POINT('Ctrl Pts',(-0.0229675645848045,0.000889001661236195,
0.00618747790900306));
#51889=CARTESIAN_POINT('Ctrl Pts',(-0.0233240023418203,0.0010564663025375,
0.00606787748581256));
#51890=CARTESIAN_POINT('Ctrl Pts',(-0.023677835969773,0.0012347319140267,
0.00595343570009491));
#51891=CARTESIAN_POINT('Ctrl Pts',(-0.023951102370562,0.00137240679337031,
0.00586505208584131));
#51892=CARTESIAN_POINT('Ctrl Pts',(-0.0242233983168268,0.0015188332599898,
0.00578093151035615));
#51893=CARTESIAN_POINT('Ctrl Pts',(-0.0244935184573884,0.00166964263063737,
0.00570110719725304));
#51894=CARTESIAN_POINT('Ctrl Pts',(-0.024689744656477,0.00177919665918037,
0.00564311958654575));
#51895=CARTESIAN_POINT('Ctrl Pts',(-0.0248847564386643,0.00189105397096317,
0.00558743987649347));
#51896=CARTESIAN_POINT('Ctrl Pts',(-0.0250806101958126,0.00200380994308026,
0.00553329955785079));
#51897=CARTESIAN_POINT('Ctrl Pts',(-0.0251969754966454,0.00207080320788732,
0.0055011324217296));
#51898=CARTESIAN_POINT('Ctrl Pts',(-0.0253133795787861,0.00213803928365046,
0.00546964294750879));
#51899=CARTESIAN_POINT('Ctrl Pts',(-0.0254299810437924,0.00220515851977943,
0.00543888238066341));
#51900=CARTESIAN_POINT('Ctrl Pts',(-0.0257797854388112,0.00240651622816635,
0.00534660068012726));
#51901=CARTESIAN_POINT('Ctrl Pts',(-0.026131284877388,0.00260689990446499,
0.00526077943816682));
#51902=CARTESIAN_POINT('Ctrl Pts',(-0.0264893372228397,0.00279674832677038,
0.00518482321349141));
#51903=CARTESIAN_POINT('Ctrl Pts',(-0.0264943584335114,0.00279941069984568,
0.00518375802788164));
#51904=CARTESIAN_POINT('Ctrl Pts',(-0.0264993810855449,0.00280207069650618,
0.0051826944884762));
#51905=CARTESIAN_POINT('Ctrl Pts',(-0.0265044052058202,0.00280472828016308,
0.00518163259052267));
#51906=CARTESIAN_POINT('Ctrl Pts',(-0.0269770608500551,0.00305474656130141,
0.00508173210370392));
#51907=CARTESIAN_POINT('Ctrl Pts',(-0.0274625835314519,0.00328308994308195,
0.00499672802735591));
#51908=CARTESIAN_POINT('Ctrl Pts',(-0.0279619732697084,0.00347647507401588,
0.00491780008001345));
#51909=CARTESIAN_POINT('Ctrl Pts',(-0.028128375408712,0.00354091312104355,
0.00489150042213339));
#51910=CARTESIAN_POINT('Ctrl Pts',(-0.0282960786034483,0.00360180694979735,
0.00486620699844024));
#51911=CARTESIAN_POINT('Ctrl Pts',(-0.0284653497047326,0.00365860512073623,
0.00484126609095895));
#51912=CARTESIAN_POINT('Ctrl Pts',(-0.0288094782020681,0.00377407591916729,
0.00479056117471157));
#51913=CARTESIAN_POINT('Ctrl Pts',(-0.0291601534207853,0.00387258032277834,
0.00474130097945834));
#51914=CARTESIAN_POINT('Ctrl Pts',(-0.0295166264965012,0.00395137882575817,
0.00468944087823975));
#51915=CARTESIAN_POINT('Ctrl Pts',(-0.0296495805641012,0.00398076837073549,
0.00467009857198194));
#51916=CARTESIAN_POINT('Ctrl Pts',(-0.0297833918223292,0.00400739927173845,
0.00465035590312184));
#51917=CARTESIAN_POINT('Ctrl Pts',(-0.0299179316600492,0.00403142587061642,
0.00463026109732501));
#51918=CARTESIAN_POINT('Ctrl Pts',(-0.0301290446636343,0.00406912717560552,
0.00459872936010782));
#51919=CARTESIAN_POINT('Ctrl Pts',(-0.0303415965120746,0.00410071552300745,
0.00456669090118318));
#51920=CARTESIAN_POINT('Ctrl Pts',(-0.0305556012738504,0.00412637462228191,
0.00453376913295831));
#51921=CARTESIAN_POINT('Ctrl Pts',(-0.0312962755608384,0.00421518122126669,
0.00441982630755575));
#51922=CARTESIAN_POINT('Ctrl Pts',(-0.0320539645187785,0.00423329656380979,
0.00429539350663322));
#51923=CARTESIAN_POINT('Ctrl Pts',(-0.0328029016201836,0.0042087665877202,
0.00416971706663987));
#51924=CARTESIAN_POINT('Ctrl Pts',(-0.0364391610694963,0.00340557668880201,
-0.00293086975220482));
#51925=CARTESIAN_POINT('Ctrl Pts',(-0.0333515059907657,0.00231570437435815,
-0.00145682442346898));
#51926=CARTESIAN_POINT('Ctrl Pts',(-0.0306323136900912,3.78646002930885E-6,
-0.00106277624427272));
#51927=CARTESIAN_POINT('Ctrl Pts',(-0.0370882476239518,0.00326876767257525,
-0.00270781351667378));
#51928=CARTESIAN_POINT('Ctrl Pts',(-0.0336803404828681,0.00234022559976933,
-0.00130013403482534));
#51929=CARTESIAN_POINT('Ctrl Pts',(-0.0307001750317395,3.81513661006243E-6,
-0.0010227126334477));
#51930=CARTESIAN_POINT('Ctrl Pts',(-0.0380711951877001,0.00301807121471456,
-0.00226920015226592));
#51931=CARTESIAN_POINT('Ctrl Pts',(-0.034177376109665,0.00240378747134278,
-0.00103180215401773));
#51932=CARTESIAN_POINT('Ctrl Pts',(-0.030832739744055,3.89817058239106E-6,
-0.000927476398380698));
#51933=CARTESIAN_POINT('Ctrl Pts',(-0.0389548787833504,0.00272631412492715,
-0.0015547766452028));
#51934=CARTESIAN_POINT('Ctrl Pts',(-0.0346510542984124,0.00247046977074249,
-0.000698423070453612));
#51935=CARTESIAN_POINT('Ctrl Pts',(-0.0310253932093769,3.98754807420298E-6,
-0.000718402588876897));
#51936=CARTESIAN_POINT('Ctrl Pts',(-0.0394299081639852,0.00253997682056228,
-0.000776937711593115));
#51937=CARTESIAN_POINT('Ctrl Pts',(-0.0349404581571179,0.00249716840139465,
-0.000359675024101642));
#51938=CARTESIAN_POINT('Ctrl Pts',(-0.0311927692352808,4.02218976237312E-6,
-0.000404760023136305));
#51939=CARTESIAN_POINT('Ctrl Pts',(-0.0395722564060474,0.0024790222613675,
-1.15969768619817E-6));
#51940=CARTESIAN_POINT('Ctrl Pts',(-0.035039641525199,0.00250059432609173,
-5.23131714616352E-7));
#51941=CARTESIAN_POINT('Ctrl Pts',(-0.0312636285943568,4.02588199220811E-6,
-5.43240818511782E-7));
#51942=CARTESIAN_POINT('Ctrl Pts',(-0.0394285060247083,0.00254062091626967,
0.000782073488798124));
#51943=CARTESIAN_POINT('Ctrl Pts',(-0.0349395146745486,0.00249717010318348,
0.000361994712682985));
#51944=CARTESIAN_POINT('Ctrl Pts',(-0.0311921191911461,4.02220893042648E-6,
0.000407199219089637));
#51945=CARTESIAN_POINT('Ctrl Pts',(-0.0389546331855897,0.00272679970989166,
0.00155567037639612));
#51946=CARTESIAN_POINT('Ctrl Pts',(-0.0346508084577749,0.00247061634579135,
0.000698666670416455));
#51947=CARTESIAN_POINT('Ctrl Pts',(-0.0310250230018649,3.98777465588809E-6,
0.000718630607728727));
#51948=CARTESIAN_POINT('Ctrl Pts',(-0.0380701459630995,0.00301899823186677,
0.00227065266162116));
#51949=CARTESIAN_POINT('Ctrl Pts',(-0.0341767045856397,0.00240421141794788,
0.0010323670224691));
#51950=CARTESIAN_POINT('Ctrl Pts',(-0.0308322812675443,3.8988403441998E-6,
0.000927873377138205));
#51951=CARTESIAN_POINT('Ctrl Pts',(-0.03709649940938,0.00326823276024269,
0.0027060963939119));
#51952=CARTESIAN_POINT('Ctrl Pts',(-0.0336843534503945,0.00234128603914245,
0.00129828781356605));
#51953=CARTESIAN_POINT('Ctrl Pts',(-0.0307005310944394,3.81666377594922E-6,
0.00102250283151694));
#51954=CARTESIAN_POINT('Ctrl Pts',(-0.0364455123647001,0.00340591076454287,
0.00292997690155913));
#51955=CARTESIAN_POINT('Ctrl Pts',(-0.0333545450336161,0.002316762246266,
0.00145544770917396));
#51956=CARTESIAN_POINT('Ctrl Pts',(-0.0306323184676507,3.78802893956849E-6,
0.00106277396492297));
#51957=CARTESIAN_POINT('',(-0.0307218899246848,7.95071454126342E-5,-0.00107604988198002));
#51958=CARTESIAN_POINT('Origin',(-0.0367505097033021,-0.0089574493287422,
-0.0114196063907013));
#51959=CARTESIAN_POINT('Ctrl Pts',(-0.0307219761960901,7.95254459509771E-5,
0.00107599840369229));
#51960=CARTESIAN_POINT('Ctrl Pts',(-0.0307952892239638,7.23751598598542E-5,
0.00102702375505616));
#51961=CARTESIAN_POINT('Ctrl Pts',(-0.0308575640997885,6.60272950011091E-5,
0.000973667173881751));
#51962=CARTESIAN_POINT('Ctrl Pts',(-0.0309105260823048,6.0949682466073E-5,
0.000919868255617537));
#51963=CARTESIAN_POINT('Ctrl Pts',(-0.030939927140558,5.81309212559178E-5,
0.000890002584910073));
#51964=CARTESIAN_POINT('Ctrl Pts',(-0.0309663339185817,5.5725626318494E-5,
0.000860199941229648));
#51965=CARTESIAN_POINT('Ctrl Pts',(-0.0309891703178521,5.39114965788957E-5,
0.000832533674153722));
#51966=CARTESIAN_POINT('Ctrl Pts',(-0.0310271481280753,5.08945290545872E-5,
0.000786523608023947));
#51967=CARTESIAN_POINT('Ctrl Pts',(-0.0310563547759014,4.85596066354287E-5,
0.000744646729173092));
#51968=CARTESIAN_POINT('Ctrl Pts',(-0.0310830526124284,4.63540473445381E-5,
0.000701615877086658));
#51969=CARTESIAN_POINT('Ctrl Pts',(-0.0311013268778553,4.4844375358352E-5,
0.000672161909467244));
#51970=CARTESIAN_POINT('Ctrl Pts',(-0.0311184086269113,4.33922934027984E-5,
0.000642052125309306));
#51971=CARTESIAN_POINT('Ctrl Pts',(-0.0311354485141428,4.17989301285626E-5,
0.000608142095971056));
#51972=CARTESIAN_POINT('Ctrl Pts',(-0.0311673311584297,3.88176525061228E-5,
0.000544694410639605));
#51973=CARTESIAN_POINT('Ctrl Pts',(-0.0311994341201196,3.69670941630756E-5,
0.000469716090898414));
#51974=CARTESIAN_POINT('Ctrl Pts',(-0.0312241401658602,3.58729802009628E-5,
0.00039074032007412));
#51975=CARTESIAN_POINT('Ctrl Pts',(-0.0312319292952294,3.55280364861704E-5,
0.000365841455138563));
#51976=CARTESIAN_POINT('Ctrl Pts',(-0.0312390169873475,3.52581840626902E-5,
0.000340594862418149));
#51977=CARTESIAN_POINT('Ctrl Pts',(-0.0312453204200204,3.5051385148846E-5,
0.000315483955331365));
#51978=CARTESIAN_POINT('Ctrl Pts',(-0.0312716174731044,3.41886485579732E-5,
0.00021072470891631));
#51979=CARTESIAN_POINT('Ctrl Pts',(-0.0312835549901547,3.291925126843E-5,
0.000105666092760674));
#51980=CARTESIAN_POINT('Ctrl Pts',(-0.0312836230622852,3.28827347166887E-5,
4.69038162585774E-7));
#51981=CARTESIAN_POINT('Ctrl Pts',(-0.0312836911344156,3.28462181649474E-5,
-0.000104728016435503));
#51982=CARTESIAN_POINT('Ctrl Pts',(-0.0312718650099121,3.40805814071716E-5,
-0.000209842528665909));
#51983=CARTESIAN_POINT('Ctrl Pts',(-0.0312455288419261,3.49919317592131E-5,
-0.000314780646790837));
#51984=CARTESIAN_POINT('Ctrl Pts',(-0.0312392913232001,3.52077780770892E-5,
-0.000339634432551035));
#51985=CARTESIAN_POINT('Ctrl Pts',(-0.03123228377827,3.54866957373038E-5,
-0.000364608910458436));
#51986=CARTESIAN_POINT('Ctrl Pts',(-0.0312245862128562,3.58386645348763E-5,
-0.000389258505156901));
#51987=CARTESIAN_POINT('Ctrl Pts',(-0.0311997829739071,3.69727849638032E-5,
-0.000468684889271354));
#51988=CARTESIAN_POINT('Ctrl Pts',(-0.0311674726314981,3.88661463710896E-5,
-0.000544246841131906));
#51989=CARTESIAN_POINT('Ctrl Pts',(-0.0311354856583077,4.18439708565057E-5,
-0.000607984583139167));
#51990=CARTESIAN_POINT('Ctrl Pts',(-0.0311185461912651,4.34209490666401E-5,
-0.000641738429546463));
#51991=CARTESIAN_POINT('Ctrl Pts',(-0.0311015799906545,4.48476797169792E-5,
-0.000671707621614676));
#51992=CARTESIAN_POINT('Ctrl Pts',(-0.0310834529036156,4.63296669299169E-5,
-0.000700990744872741));
#51993=CARTESIAN_POINT('Ctrl Pts',(-0.0310567274409192,4.85146177657057E-5,
-0.000744163981509777));
#51994=CARTESIAN_POINT('Ctrl Pts',(-0.0310275253588562,5.08264957832321E-5,
-0.000786099484748195));
#51995=CARTESIAN_POINT('Ctrl Pts',(-0.0309894158192428,5.38536203572919E-5,
-0.000832278091066834));
#51996=CARTESIAN_POINT('Ctrl Pts',(-0.0309665454929332,5.56702606917277E-5,
-0.000859990831911842));
#51997=CARTESIAN_POINT('Ctrl Pts',(-0.0309401709900778,5.8085624176027E-5,
-0.000889753759681022));
#51998=CARTESIAN_POINT('Ctrl Pts',(-0.0309107199611745,6.09170276475944E-5,
-0.000919657366608743));
#51999=CARTESIAN_POINT('Ctrl Pts',(-0.0308578095907544,6.60037975184087E-5,
-0.00097338081799111));
#52000=CARTESIAN_POINT('Ctrl Pts',(-0.0307952836375779,7.23588730805084E-5,
-0.00102702773176624));
#52001=CARTESIAN_POINT('Ctrl Pts',(-0.0307218911474655,7.95069316882072E-5,
-0.00107604898256824));
#52002=CARTESIAN_POINT('Ctrl Pts',(-0.0306659720248312,3.23414461730682E-5,
-0.00106769530807909));
#52003=CARTESIAN_POINT('Ctrl Pts',(-0.0333716875076,0.0023228279927353,
-0.00146645907172397));
#52004=CARTESIAN_POINT('Ctrl Pts',(-0.0364391610694963,0.00340557668880201,
-0.0029308697522048));
#52005=CARTESIAN_POINT('Ctrl Pts',(-0.0304648451406503,3.25593610126452E-5,
-0.00118610079900385));
#52006=CARTESIAN_POINT('Ctrl Pts',(-0.033177519503754,0.00233892557013915,
-0.00154659656588374));
#52007=CARTESIAN_POINT('Ctrl Pts',(-0.036259057400032,0.00344353742848523,
-0.0029927617234314));
#52008=CARTESIAN_POINT('Ctrl Pts',(-0.0300655212000987,3.30036942474922E-5,
-0.00142117692855237));
#52009=CARTESIAN_POINT('Ctrl Pts',(-0.032787882853436,0.00237171648936093,
-0.00170736037005578));
#52010=CARTESIAN_POINT('Ctrl Pts',(-0.0358936020458381,0.00352256019043282,
-0.00311869399351504));
#52011=CARTESIAN_POINT('Ctrl Pts',(-0.0294730439529765,3.36869730645144E-5,
-0.00176993295614264));
#52012=CARTESIAN_POINT('Ctrl Pts',(-0.0321940369640194,0.00242192567971165,
-0.00195299737112982));
#52013=CARTESIAN_POINT('Ctrl Pts',(-0.0353202505619921,0.00365077259747625,
-0.00331582646852773));
#52014=CARTESIAN_POINT('Ctrl Pts',(-0.0288844566138175,3.43805751075243E-5,
-0.00211638087976133));
#52015=CARTESIAN_POINT('Ctrl Pts',(-0.0315837846962915,0.00247253394371439,
-0.00220730892162865));
#52016=CARTESIAN_POINT('Ctrl Pts',(-0.0347097518201094,0.0037892002750051,
-0.00352417393855777));
#52017=CARTESIAN_POINT('Ctrl Pts',(-0.0283946132121652,3.49644787594377E-5,
-0.00240470419248045));
#52018=CARTESIAN_POINT('Ctrl Pts',(-0.0310540109273581,0.00251466505539929,
-0.00243127336975895));
#52019=CARTESIAN_POINT('Ctrl Pts',(-0.034156713001383,0.0039137701019183,
-0.00371122941019911));
#52020=CARTESIAN_POINT('Ctrl Pts',(-0.0280011050394867,3.54363580167864E-5,
-0.00263633501468253));
#52021=CARTESIAN_POINT('Ctrl Pts',(-0.0306106703026876,0.00254828741318223,
-0.00262215176228272));
#52022=CARTESIAN_POINT('Ctrl Pts',(-0.0336756196744561,0.00401973235510397,
-0.00387342560833778));
#52023=CARTESIAN_POINT('Ctrl Pts',(-0.0277045049304437,3.57938454752424E-5,
-0.00281093281213578));
#52024=CARTESIAN_POINT('Ctrl Pts',(-0.0302660225247906,0.0025734969554845,
-0.00277278147548018));
#52025=CARTESIAN_POINT('Ctrl Pts',(-0.0332910571209545,0.00410268222584421,
-0.00400318713095339));
#52026=CARTESIAN_POINT('Ctrl Pts',(-0.0274056655920821,3.61568571396258E-5,
-0.00298686453896102));
#52027=CARTESIAN_POINT('Ctrl Pts',(-0.0299061539411528,0.00259878283369678,
-0.0029329650039485));
#52028=CARTESIAN_POINT('Ctrl Pts',(-0.0328771438690326,0.00418955458028497,
-0.0041435432325896));
#52029=CARTESIAN_POINT('Ctrl Pts',(-0.0271539582111298,3.64666901547067E-5,
-0.00313506846284764));
#52030=CARTESIAN_POINT('Ctrl Pts',(-0.029590063973267,0.00262005567911308,
-0.00307679824266307));
#52031=CARTESIAN_POINT('Ctrl Pts',(-0.0325013306245234,0.00426576503991228,
-0.00427235715587504));
#52032=CARTESIAN_POINT('Ctrl Pts',(-0.0269503393755227,3.6721787310625E-5,
-0.00325497529873103));
#52033=CARTESIAN_POINT('Ctrl Pts',(-0.0293243762770283,0.00263735268991712,
-0.00320018057455909));
#52034=CARTESIAN_POINT('Ctrl Pts',(-0.0321764258442447,0.00432954907901014,
-0.00438539085653449));
#52035=CARTESIAN_POINT('Ctrl Pts',(-0.0267962883207492,3.69178344365261E-5,
-0.00334570310540647));
#52036=CARTESIAN_POINT('Ctrl Pts',(-0.0291176448799536,0.00265052820534663,
-0.00329760173839145));
#52037=CARTESIAN_POINT('Ctrl Pts',(-0.0319185969267873,0.00437899055578669,
-0.0044762214375067));
#52038=CARTESIAN_POINT('Ctrl Pts',(-0.0266665944406192,3.70863136558612E-5,
-0.0034220962932131));
#52039=CARTESIAN_POINT('Ctrl Pts',(-0.0289380157869116,0.00266174944143041,
-0.00338361927320225));
#52040=CARTESIAN_POINT('Ctrl Pts',(-0.03168990188217,0.00442172936806749,
-0.00455806239367165));
#52041=CARTESIAN_POINT('Ctrl Pts',(-0.0265618958214666,3.72251893031226E-5,
-0.00348377426723578));
#52042=CARTESIAN_POINT('Ctrl Pts',(-0.0287890193227952,0.00267093562259292,
-0.0034559335693082));
#52043=CARTESIAN_POINT('Ctrl Pts',(-0.0314969971377745,0.00445701329688577,
-0.00462814357193572));
#52044=CARTESIAN_POINT('Ctrl Pts',(-0.0264828543740696,3.73316761200374E-5,
-0.00353034182108191));
#52045=CARTESIAN_POINT('Ctrl Pts',(-0.028674364485197,0.00267794695681193,
-0.00351209763611023));
#52046=CARTESIAN_POINT('Ctrl Pts',(-0.0313468383591297,0.00448406951464358,
-0.00468329547025618));
#52047=CARTESIAN_POINT('Ctrl Pts',(-0.0264032446328258,3.74410903480025E-5,
-0.00357724898004166));
#52048=CARTESIAN_POINT('Ctrl Pts',(-0.0285564496828184,0.00268512044202649,
-0.00357043197867147));
#52049=CARTESIAN_POINT('Ctrl Pts',(-0.0311905579210017,0.00451181067552851,
-0.00474142017246755));
#52050=CARTESIAN_POINT('Ctrl Pts',(-0.026336381527319,3.75344633438766E-5,
-0.00361664980215379));
#52051=CARTESIAN_POINT('Ctrl Pts',(-0.0284552362796348,0.00269121413078742,
-0.00362099712426088));
#52052=CARTESIAN_POINT('Ctrl Pts',(-0.0310548025406171,0.00453546900121625,
-0.00479255366026566));
#52053=CARTESIAN_POINT('Ctrl Pts',(-0.0262825439416979,3.76122232159902E-5,
-0.00364837848343752));
#52054=CARTESIAN_POINT('Ctrl Pts',(-0.0283720828908489,0.00269628089830896,
-0.00366293169460257));
#52055=CARTESIAN_POINT('Ctrl Pts',(-0.0309420996512683,0.00455497260274855,
-0.00483561125614202));
#52056=CARTESIAN_POINT('Ctrl Pts',(-0.0262419843009898,3.76684800715227E-5,
-0.00367228206963774));
#52057=CARTESIAN_POINT('Ctrl Pts',(-0.0283090423271439,0.00269992121442134,
-0.00369476448950497));
#52058=CARTESIAN_POINT('Ctrl Pts',(-0.0308563295614869,0.00456937467996215,
-0.00486834081427539));
#52059=CARTESIAN_POINT('Ctrl Pts',(-0.026208019901491,3.77262236784257E-5,
-0.00369230473668905));
#52060=CARTESIAN_POINT('Ctrl Pts',(-0.0282542595847076,0.00270371457179228,
-0.00372301745429584));
#52061=CARTESIAN_POINT('Ctrl Pts',(-0.0307805550690652,0.00458299051760416,
-0.00489846967193485));
#52062=CARTESIAN_POINT('Ctrl Pts',(-0.0261808045216819,3.77507625204141E-5,
-0.0037083394051121));
#52063=CARTESIAN_POINT('Ctrl Pts',(-0.0282127768541347,0.00270520608416526,
-0.0037435677573533));
#52064=CARTESIAN_POINT('Ctrl Pts',(-0.0307244920527542,0.00459080952707601,
-0.0049188319945771));
#52065=CARTESIAN_POINT('Ctrl Pts',(-0.0261636656099131,3.781705370848E-5,
-0.00371846090632498));
#52066=CARTESIAN_POINT('Ctrl Pts',(-0.0281799200617113,0.00270975005130535,
-0.00376216305046526));
#52067=CARTESIAN_POINT('Ctrl Pts',(-0.0306760558540184,0.00460301804700601,
-0.00494167931077386));
#52068=CARTESIAN_POINT('Ctrl Pts',(-0.0261518327430556,3.77620276636738E-5,
-0.00372540271260059));
#52069=CARTESIAN_POINT('Ctrl Pts',(-0.0281701564974934,0.0027057343796972,
-0.00376409478037424));
#52070=CARTESIAN_POINT('Ctrl Pts',(-0.0306677672477296,0.0045970237335782,
-0.00493804696372403));
#52071=CARTESIAN_POINT('Ctrl Pts',(-0.026144776878792,3.78895509816586E-5,
-0.00372961580310048));
#52072=CARTESIAN_POINT('Ctrl Pts',(-0.0281436128678637,0.00271471501069469,
-0.00378271465869179));
#52073=CARTESIAN_POINT('Ctrl Pts',(-0.0306224655607035,0.00461639993926548,
-0.00496693774563895));
#52074=CARTESIAN_POINT('Ctrl Pts',(-0.0261374135605129,3.81565997376382E-5,
-0.00373407433410709));
#52075=CARTESIAN_POINT('Ctrl Pts',(-0.0280980043109231,0.00273359669628745,
-0.00381711382495484));
#52076=CARTESIAN_POINT('Ctrl Pts',(-0.0305403726405734,0.00465570696437846,
-0.0050239034882587));
#52077=CARTESIAN_POINT('Ctrl Pts',(-0.0261281640494186,3.84630626987939E-5,
-0.0037396621267139));
#52078=CARTESIAN_POINT('Ctrl Pts',(-0.0280434152443195,0.00275526528829198,
-0.00385782364150545));
#52079=CARTESIAN_POINT('Ctrl Pts',(-0.0304426025519808,0.00470080251139039,
-0.00509131932699353));
#52080=CARTESIAN_POINT('Ctrl Pts',(-0.0261054356644294,3.93073156687108E-5,
-0.00375343659204118));
#52081=CARTESIAN_POINT('Ctrl Pts',(-0.0278926602692761,0.00281505248511113,
-0.00397082959078529));
#52082=CARTESIAN_POINT('Ctrl Pts',(-0.0301707424124219,0.00482364365284629,
-0.00528219616543048));
#52083=CARTESIAN_POINT('Ctrl Pts',(-0.0260771330242492,4.05187705868077E-5,
-0.00377066835420024));
#52084=CARTESIAN_POINT('Ctrl Pts',(-0.0276722875172353,0.00290083210877017,
-0.00413643781579527));
#52085=CARTESIAN_POINT('Ctrl Pts',(-0.0297686688678292,0.00499915145989499,
-0.00556598995984482));
#52086=CARTESIAN_POINT('Ctrl Pts',(-0.0260409078612633,4.28160435087016E-5,
-0.00379308713029676));
#52087=CARTESIAN_POINT('Ctrl Pts',(-0.0272167184552454,0.00306650436760558,
-0.00447832811660013));
#52088=CARTESIAN_POINT('Ctrl Pts',(-0.02894101596812,0.00530184713024665,
-0.00621428296024427));
#52089=CARTESIAN_POINT('Ctrl Pts',(-0.0260043538115754,4.48407708557987E-5,
-0.0038155958698829));
#52090=CARTESIAN_POINT('Ctrl Pts',(-0.0267800050596834,0.00321559967836929,
-0.00480317582103633));
#52091=CARTESIAN_POINT('Ctrl Pts',(-0.0281727309093209,0.00554213262362041,
-0.0068677022049604));
#52092=CARTESIAN_POINT('Ctrl Pts',(-0.0259607701533692,4.61221805003758E-5,
-0.00384194401496335));
#52093=CARTESIAN_POINT('Ctrl Pts',(-0.0264635524308429,0.00331280008633878,
-0.00503500639952359));
#52094=CARTESIAN_POINT('Ctrl Pts',(-0.0276519466871055,0.0056709408313574,
-0.00735233283735931));
#52095=CARTESIAN_POINT('Ctrl Pts',(-0.0259109208809971,4.70910894813173E-5,
-0.00387187549175774));
#52096=CARTESIAN_POINT('Ctrl Pts',(-0.026200151872293,0.00338747640947883,
-0.00522676295442198));
#52097=CARTESIAN_POINT('Ctrl Pts',(-0.027237389066601,0.00575939777742583,
-0.00775104175037189));
#52098=CARTESIAN_POINT('Ctrl Pts',(-0.0258623967014985,4.77672103359955E-5,
-0.00390090483387817));
#52099=CARTESIAN_POINT('Ctrl Pts',(-0.025995917206177,0.00344054815113673,
-0.0053746982282801));
#52100=CARTESIAN_POINT('Ctrl Pts',(-0.026929683601278,0.00581356526299246,
-0.00805724361079941));
#52101=CARTESIAN_POINT('Ctrl Pts',(-0.0258146910606012,4.82892558635125E-5,
-0.0039293909184561));
#52102=CARTESIAN_POINT('Ctrl Pts',(-0.0258238363018331,0.00348207689599807,
-0.00549910882314107));
#52103=CARTESIAN_POINT('Ctrl Pts',(-0.0266786334686938,0.00585101008285789,
-0.00831178973482216));
#52104=CARTESIAN_POINT('Ctrl Pts',(-0.0257518916199959,4.88478750726719E-5,
-0.00396684362353593));
#52105=CARTESIAN_POINT('Ctrl Pts',(-0.0256230629559801,0.00352712041636869,
-0.00564414155165935));
#52106=CARTESIAN_POINT('Ctrl Pts',(-0.0263940947126037,0.00588622677513632,
-0.00860493329766318));
#52107=CARTESIAN_POINT('Ctrl Pts',(-0.0256743693417282,4.9371818595519E-5,
-0.00401302077025589));
#52108=CARTESIAN_POINT('Ctrl Pts',(-0.0254088152555184,0.00357018457708517,
-0.00579897033516915));
#52109=CARTESIAN_POINT('Ctrl Pts',(-0.0261016797480758,0.00591221324371429,
-0.00891170623644723));
#52110=CARTESIAN_POINT('Ctrl Pts',(-0.0255832224951489,4.98366328551321E-5,
-0.00406726790446615));
#52111=CARTESIAN_POINT('Ctrl Pts',(-0.0251877774792792,0.00360923613531693,
-0.00595913824631443));
#52112=CARTESIAN_POINT('Ctrl Pts',(-0.0258107866044053,0.00592748036538003,
-0.0092212190412313));
#52113=CARTESIAN_POINT('Ctrl Pts',(-0.0254936679857824,5.01927210102786E-5,
-0.0041205400118894));
#52114=CARTESIAN_POINT('Ctrl Pts',(-0.0249911997814267,0.00363983237155333,
-0.00610211634548159));
#52115=CARTESIAN_POINT('Ctrl Pts',(-0.0255597507675584,0.00593263301939726,
-0.00949085425259816));
#52116=CARTESIAN_POINT('Ctrl Pts',(-0.0253758720415834,5.05651453544886E-5,
-0.0041905884775542));
#52117=CARTESIAN_POINT('Ctrl Pts',(-0.0247522793478318,0.00367260676775817,
-0.00627664770945765));
#52118=CARTESIAN_POINT('Ctrl Pts',(-0.0252623164499094,0.00593028312395291,
-0.00981230212490256));
#52119=CARTESIAN_POINT('Ctrl Pts',(-0.0252311192315282,5.0888763299654E-5,
-0.00427663842767887));
#52120=CARTESIAN_POINT('Ctrl Pts',(-0.0244864841034371,0.00370231723272169,
-0.00647221927186298));
#52121=CARTESIAN_POINT('Ctrl Pts',(-0.0249420453960832,0.00591497917482241,
-0.010160472132548));
#52122=CARTESIAN_POINT('Ctrl Pts',(-0.0250602889666802,5.11360242616874E-5,
-0.00437816818346445));
#52123=CARTESIAN_POINT('Ctrl Pts',(-0.0242010563876091,0.00372660364023652,
-0.00668426186641994));
#52124=CARTESIAN_POINT('Ctrl Pts',(-0.0246086007077068,0.00588499648903705,
-0.0105235090876737));
#52125=CARTESIAN_POINT('Ctrl Pts',(-0.0248917111638188,5.12844272019451E-5,
-0.00447834690785075));
#52126=CARTESIAN_POINT('Ctrl Pts',(-0.0239395957750621,0.00374282506840123,
-0.00688033142308394));
#52127=CARTESIAN_POINT('Ctrl Pts',(-0.0243106749899636,0.00584724957039815,
-0.0108472856043692));
#52128=CARTESIAN_POINT('Ctrl Pts',(-0.0246693003821806,5.13849543682559E-5,
-0.00461050700441935));
#52129=CARTESIAN_POINT('Ctrl Pts',(-0.0236148624308845,0.00375641825322508,
-0.00712603678614978));
#52130=CARTESIAN_POINT('Ctrl Pts',(-0.0239481818224663,0.00578962008503306,
-0.0112395797881903));
#52131=CARTESIAN_POINT('Ctrl Pts',(-0.0243953711908193,5.13711945846472E-5,
-0.00477327030270521));
#52132=CARTESIAN_POINT('Ctrl Pts',(-0.0232447751136219,0.00376172831682206,
-0.0074096868729248));
#52133=CARTESIAN_POINT('Ctrl Pts',(-0.0235452646130942,0.00570778643045448,
-0.0116715846411793));
#52134=CARTESIAN_POINT('Ctrl Pts',(-0.0240726649027794,5.12118187243539E-5,
-0.00496501010794583));
#52135=CARTESIAN_POINT('Ctrl Pts',(-0.0228405020174707,0.00375586822790691,
-0.00772394722759367));
#52136=CARTESIAN_POINT('Ctrl Pts',(-0.0231148301912106,0.00560105104734249,
-0.0121256226619798));
#52137=CARTESIAN_POINT('Ctrl Pts',(-0.0236480460595398,5.08634391604083E-5,
-0.00521729715840131));
#52138=CARTESIAN_POINT('Ctrl Pts',(-0.0223393718662674,0.00373624599895701,
-0.00811812347554683));
#52139=CARTESIAN_POINT('Ctrl Pts',(-0.022590417361574,0.00545157456564356,
-0.0126684112001716));
#52140=CARTESIAN_POINT('Ctrl Pts',(-0.0231256191168733,5.02401014976624E-5,
-0.0055276861175585));
#52141=CARTESIAN_POINT('Ctrl Pts',(-0.0217671013382464,0.00369518212874887,
-0.0085748562026785));
#52142=CARTESIAN_POINT('Ctrl Pts',(-0.0220027039981841,0.00525666829407956,
-0.0132572883380559));
#52143=CARTESIAN_POINT('Ctrl Pts',(-0.022506802832622,4.93019261157021E-5,
-0.00589531188146266));
#52144=CARTESIAN_POINT('Ctrl Pts',(-0.021134550013562,0.00362896008264994,
-0.00908521441965309));
#52145=CARTESIAN_POINT('Ctrl Pts',(-0.0213625517960801,0.00501846018383101,
-0.0138697797012409));
#52146=CARTESIAN_POINT('Ctrl Pts',(-0.0216884633928667,4.78671456038939E-5,
-0.00638140703944321));
#52147=CARTESIAN_POINT('Ctrl Pts',(-0.0203407251070505,0.00352427154951466,
-0.00972847192511815));
#52148=CARTESIAN_POINT('Ctrl Pts',(-0.0205673942342202,0.0047004754260775,
-0.0145940979045826));
#52149=CARTESIAN_POINT('Ctrl Pts',(-0.0210778116756395,4.66312446128068E-5,
-0.00674404056932037));
#52150=CARTESIAN_POINT('Ctrl Pts',(-0.019783209720137,0.0034317380242369,
-0.0101790687897771));
#52151=CARTESIAN_POINT('Ctrl Pts',(-0.0200147944465283,0.0044649192266308,
-0.0150590894458486));
#52152=CARTESIAN_POINT('Ctrl Pts',(-0.0206712477487095,4.5762457771723E-5,
-0.00698541821209234));
#52153=CARTESIAN_POINT('Ctrl Pts',(-0.0194199829425201,0.00336621201589046,
-0.0104694405421481));
#52154=CARTESIAN_POINT('Ctrl Pts',(-0.0196565859278358,0.00431125424739362,
-0.0153459530959679));
#52155=CARTESIAN_POINT('',(-0.0207149455870811,8.43554850505981E-5,-0.00699117714093166));
#52156=CARTESIAN_POINT('Ctrl Pts',(-0.0327968762032639,0.00420554807594454,
-0.00417120478069329));
#52157=CARTESIAN_POINT('Ctrl Pts',(-0.0317030654778017,0.00424097888210346,
-0.00435540229680534));
#52158=CARTESIAN_POINT('Ctrl Pts',(-0.0295266041626024,0.00414882581713682,
-0.00470177324033703));
#52159=CARTESIAN_POINT('Ctrl Pts',(-0.0264213259365022,0.00288385212068659,
-0.00513303967806249));
#52160=CARTESIAN_POINT('Ctrl Pts',(-0.0236967389144328,0.00113672339326093,
-0.00593058660740073));
#52161=CARTESIAN_POINT('Ctrl Pts',(-0.0217311533549796,0.000374146536090822,
-0.00662175902642767));
#52162=CARTESIAN_POINT('Ctrl Pts',(-0.0207149455884397,8.4355483057549E-5,
-0.00699117714319741));
#52163=CARTESIAN_POINT('',(-0.0263907115489401,0.00012245196838643,-0.00362513812701022));
#52164=CARTESIAN_POINT('Ctrl Pts',(-0.0207149455828892,8.4355490703393E-5,
-0.006991177133933));
#52165=CARTESIAN_POINT('Ctrl Pts',(-0.0210971425310402,8.77204073903474E-5,
-0.00676497304784093));
#52166=CARTESIAN_POINT('Ctrl Pts',(-0.0214863236218676,9.05689834324322E-5,
-0.00653393795875628));
#52167=CARTESIAN_POINT('Ctrl Pts',(-0.0218760532400046,9.32600036074344E-5,
-0.00630236302065223));
#52168=CARTESIAN_POINT('Ctrl Pts',(-0.022080500283299,9.46716774772691E-5,
-0.00618088184705613));
#52169=CARTESIAN_POINT('Ctrl Pts',(-0.0222850980092275,9.60418134407925E-5,
-0.00605925085010957));
#52170=CARTESIAN_POINT('Ctrl Pts',(-0.022489291818599,9.74297572472183E-5,
-0.00593785507351048));
#52171=CARTESIAN_POINT('Ctrl Pts',(-0.0226961163953625,9.8835582875424E-5,
-0.00581489527275426));
#52172=CARTESIAN_POINT('Ctrl Pts',(-0.0229025297706422,0.000100259754044708,
-0.00569217496529666));
#52173=CARTESIAN_POINT('Ctrl Pts',(-0.0231078996179027,0.000101763864891936,
-0.00557011741350745));
#52174=CARTESIAN_POINT('Ctrl Pts',(-0.0233182839071471,0.000103304701074851,
-0.00544507962620509));
#52175=CARTESIAN_POINT('Ctrl Pts',(-0.0235275821357207,0.000104929497605713,
-0.00532073201507991));
#52176=CARTESIAN_POINT('Ctrl Pts',(-0.0237353773562675,0.000106690091906569,
-0.00519735968999793));
#52177=CARTESIAN_POINT('Ctrl Pts',(-0.0238420277422174,0.000107593712601952,
-0.00513403914753832));
#52178=CARTESIAN_POINT('Ctrl Pts',(-0.023948279138249,0.000108533185086646,
-0.00507097714903515));
#52179=CARTESIAN_POINT('Ctrl Pts',(-0.0240540984753581,0.000109511365780083,
-0.00500819657265365));
#52180=CARTESIAN_POINT('Ctrl Pts',(-0.0241623291302322,0.00011051183639281,
-0.00494398540784414));
#52181=CARTESIAN_POINT('Ctrl Pts',(-0.0242701098690006,0.00011155278958794,
-0.00488006741271473));
#52182=CARTESIAN_POINT('Ctrl Pts',(-0.0243775251874332,0.000112632461217019,
-0.00481639370375624));
#52183=CARTESIAN_POINT('Ctrl Pts',(-0.0244878858778078,0.000113741737883529,
-0.00475097403566873));
#52184=CARTESIAN_POINT('Ctrl Pts',(-0.0245978582774167,0.000114891830942718,
-0.00468581373652554));
#52185=CARTESIAN_POINT('Ctrl Pts',(-0.0247073028057999,0.000116066635648145,
-0.00462099409244789));
#52186=CARTESIAN_POINT('Ctrl Pts',(-0.0247633267969307,0.000116668011060599,
-0.00458781330928266));
#52187=CARTESIAN_POINT('Ctrl Pts',(-0.0248192121921035,0.000117275872470403,
-0.00455472194213076));
#52188=CARTESIAN_POINT('Ctrl Pts',(-0.0248749543343892,0.00011788541951887,
-0.00452172172282054));
#52189=CARTESIAN_POINT('Ctrl Pts',(-0.024931690820346,0.0001185058398353,
-0.00448813283651845));
#52190=CARTESIAN_POINT('Ctrl Pts',(-0.0249882794376936,0.00011912799642088,
-0.00445463805534672));
#52191=CARTESIAN_POINT('Ctrl Pts',(-0.0250447742563322,0.000119743657011892,
-0.00442120295626946));
#52192=CARTESIAN_POINT('Ctrl Pts',(-0.0251023743207899,0.000120371362181692,
-0.0043871137440477));
#52193=CARTESIAN_POINT('Ctrl Pts',(-0.0251598771560652,0.000120992292342631,
-0.00435308640225312));
#52194=CARTESIAN_POINT('Ctrl Pts',(-0.0252173636492093,0.000121591559253424,
-0.0043190684232904));
#52195=CARTESIAN_POINT('Ctrl Pts',(-0.0252760858756926,0.00012220370804412,
-0.00428431919167278));
#52196=CARTESIAN_POINT('Ctrl Pts',(-0.0253347920219821,0.000122793183487558,
-0.00424957913155028));
#52197=CARTESIAN_POINT('Ctrl Pts',(-0.0253936652971408,0.000123327091914099,
-0.00421472854072798));
#52198=CARTESIAN_POINT('Ctrl Pts',(-0.0254236140176411,0.000123598690091644,
-0.00419700011299922));
#52199=CARTESIAN_POINT('Ctrl Pts',(-0.0254536056518887,0.000123855923585816,
-0.00417924328455579));
#52200=CARTESIAN_POINT('Ctrl Pts',(-0.025483680306593,0.000124090809101317,
-0.00416143145143432));
#52201=CARTESIAN_POINT('Ctrl Pts',(-0.0255141264866617,0.000124328596260332,
-0.00414339958094724));
#52202=CARTESIAN_POINT('Ctrl Pts',(-0.0255446579384126,0.000124543468298433,
-0.00412531122314441));
#52203=CARTESIAN_POINT('Ctrl Pts',(-0.0255753507891367,0.000124722389861798,
-0.00410711639013784));
#52204=CARTESIAN_POINT('Ctrl Pts',(-0.0256064423089494,0.000124903635435311,
-0.00408868522465257));
#52205=CARTESIAN_POINT('Ctrl Pts',(-0.0256376993502233,0.000125047966296222,
-0.00407014484895584));
#52206=CARTESIAN_POINT('Ctrl Pts',(-0.0256691971115749,0.000125132429964907,
-0.00405144207391461));
#52207=CARTESIAN_POINT('Ctrl Pts',(-0.0256838674422491,0.000125171769584499,
-0.00404273110898868));
#52208=CARTESIAN_POINT('Ctrl Pts',(-0.0256985899060688,0.000125198128355305,
-0.00403398496786023));
#52209=CARTESIAN_POINT('Ctrl Pts',(-0.0257133663180243,0.000125206745692729,
-0.00402520073294849));
#52210=CARTESIAN_POINT('Ctrl Pts',(-0.0257310516727892,0.000125217059473227,
-0.00401468719886324));
#52211=CARTESIAN_POINT('Ctrl Pts',(-0.0257484825402284,0.000125339361806644,
-0.00400438085172023));
#52212=CARTESIAN_POINT('Ctrl Pts',(-0.0257657329491683,0.000125544176069823,
-0.00399422365467317));
#52213=CARTESIAN_POINT('Ctrl Pts',(-0.0257823462027672,0.00012574142538181,
-0.00398444162046256));
#52214=CARTESIAN_POINT('Ctrl Pts',(-0.0257987928730291,0.000126015157500993,
-0.0039747974374639));
#52215=CARTESIAN_POINT('Ctrl Pts',(-0.0258151980186753,0.0001263309593292,
-0.00396520106776497));
#52216=CARTESIAN_POINT('Ctrl Pts',(-0.0258320993572177,0.00012665631295458,
-0.00395531444459447));
#52217=CARTESIAN_POINT('Ctrl Pts',(-0.0258489562467072,0.000127026371687109,
-0.00394547881739026));
#52218=CARTESIAN_POINT('Ctrl Pts',(-0.0258659177543635,0.000127395692270414,
-0.00393558539541793));
#52219=CARTESIAN_POINT('Ctrl Pts',(-0.025883265195321,0.000127773416181702,
-0.0039254668636806));
#52220=CARTESIAN_POINT('Ctrl Pts',(-0.0259007216997102,0.000128150501446182,
-0.00391528815415423));
#52221=CARTESIAN_POINT('Ctrl Pts',(-0.0259185665436356,0.00012843687551344,
-0.00390484414244605));
#52222=CARTESIAN_POINT('Ctrl Pts',(-0.0259366611520451,0.000128727257801305,
-0.00389425395163948));
#52223=CARTESIAN_POINT('Ctrl Pts',(-0.0259551529365133,0.000128925110284922,
-0.00388339255718412));
#52224=CARTESIAN_POINT('Ctrl Pts',(-0.0259745838996711,0.000128865299578265,
-0.00387186678728443));
#52225=CARTESIAN_POINT('Ctrl Pts',(-0.0259941009118485,0.000128805224002974,
-0.00386028997610637));
#52226=CARTESIAN_POINT('Ctrl Pts',(-0.0260145501188438,0.000128491487357182,
-0.0038480546690898));
#52227=CARTESIAN_POINT('Ctrl Pts',(-0.0260374058089729,0.000127165890519034,
-0.00383395735489107));
#52228=CARTESIAN_POINT('Ctrl Pts',(-0.0260488015913114,0.000126504951691511,
-0.00382692847397526));
#52229=CARTESIAN_POINT('Ctrl Pts',(-0.0260608038279689,0.000125589576025012,
-0.00381943053662304));
#52230=CARTESIAN_POINT('Ctrl Pts',(-0.0260729178646133,0.000124548724251656,
-0.00381181917277744));
#52231=CARTESIAN_POINT('Ctrl Pts',(-0.0260849702930928,0.00012351316592173,
-0.00380424651792476));
#52232=CARTESIAN_POINT('Ctrl Pts',(-0.026097136401074,0.000122351777904879,
-0.0037965591434672));
#52233=CARTESIAN_POINT('Ctrl Pts',(-0.0261086052243113,0.000121387047784687,
-0.00378937964865003));
#52234=CARTESIAN_POINT('Ctrl Pts',(-0.026131264223562,0.000119481026685734,
-0.00377519509245661));
#52235=CARTESIAN_POINT('Ctrl Pts',(-0.0261511521497109,0.000118360387665682,
-0.00376303046579071));
#52236=CARTESIAN_POINT('Ctrl Pts',(-0.0261698961696417,0.000117479077949222,
-0.0037516577649883));
#52237=CARTESIAN_POINT('Ctrl Pts',(-0.0261745200568637,0.000117261671184203,
-0.00374885227896585));
#52238=CARTESIAN_POINT('Ctrl Pts',(-0.0261790760477508,0.000117058244254152,
-0.00374609367896718));
#52239=CARTESIAN_POINT('Ctrl Pts',(-0.0261835583029753,0.000116877142890749,
-0.00374338935602184));
#52240=CARTESIAN_POINT('Ctrl Pts',(-0.0261880122804294,0.000116697184064419,
-0.00374070209418065));
#52241=CARTESIAN_POINT('Ctrl Pts',(-0.0261923929005556,0.000116539567001617,
-0.003738068887214));
#52242=CARTESIAN_POINT('Ctrl Pts',(-0.0261967973758367,0.000116354157551165,
-0.0037354094319082));
#52243=CARTESIAN_POINT('Ctrl Pts',(-0.0262011720497276,0.00011617000261096,
-0.00373276797090596));
#52244=CARTESIAN_POINT('Ctrl Pts',(-0.0262054331910358,0.000116028478557896,
-0.00373021344893865));
#52245=CARTESIAN_POINT('Ctrl Pts',(-0.0262092655210476,0.000116119637537204,
-0.00372801812796615));
#52246=CARTESIAN_POINT('Ctrl Pts',(-0.026213070257243,0.000116210140147112,
-0.00372583861390066));
#52247=CARTESIAN_POINT('Ctrl Pts',(-0.0262165886660585,0.000116460366263563,
-0.00372390094085995));
#52248=CARTESIAN_POINT('Ctrl Pts',(-0.0262201693461397,0.000116679298603018,
-0.00372191249859911));
#52249=CARTESIAN_POINT('Ctrl Pts',(-0.0262272477875872,0.000117112093410339,
-0.00371798166093806));
#52250=CARTESIAN_POINT('Ctrl Pts',(-0.0262345801580936,0.000117416809093337,
-0.00371384355418574));
#52251=CARTESIAN_POINT('Ctrl Pts',(-0.0262419010935463,0.000117740035136958,
-0.00370972144139412));
#52252=CARTESIAN_POINT('Ctrl Pts',(-0.0262491002484858,0.000118057884458753,
-0.00370566789811987));
#52253=CARTESIAN_POINT('Ctrl Pts',(-0.0262562845165814,0.000118395727247598,
-0.00370163303098062));
#52254=CARTESIAN_POINT('Ctrl Pts',(-0.0262635258941543,0.000118715228742628,
-0.00369755689516486));
#52255=CARTESIAN_POINT('Ctrl Pts',(-0.0262776136679998,0.000119336804507724,
-0.00368962695656447));
#52256=CARTESIAN_POINT('Ctrl Pts',(-0.0262919220400696,0.000119886589927717,
-0.0036815371309529));
#52257=CARTESIAN_POINT('Ctrl Pts',(-0.0263064318609315,0.000120380521748309,
-0.00367330567369189));
#52258=CARTESIAN_POINT('Ctrl Pts',(-0.0263203695794753,0.000120854978515265,
-0.00366539877149084));
#52259=CARTESIAN_POINT('Ctrl Pts',(-0.0263344916015547,0.000121278768971522,
-0.00365736250963555));
#52260=CARTESIAN_POINT('Ctrl Pts',(-0.0263488388037353,0.000121633145238242,
-0.00364916383368701));
#52261=CARTESIAN_POINT('Ctrl Pts',(-0.026362581742611,0.000121972596185628,
-0.00364131046262522));
#52262=CARTESIAN_POINT('Ctrl Pts',(-0.0263765316258872,0.000122248123640011,
-0.00363330776749834));
#52263=CARTESIAN_POINT('Ctrl Pts',(-0.0263907115489401,0.00012245196838643,
-0.00362513812701022));
#52264=CARTESIAN_POINT('Ctrl Pts',(-0.0263907115489401,0.00012245196838643,
-0.00362513812701022));
#52265=CARTESIAN_POINT('Ctrl Pts',(-0.0264171761508432,0.000122832412627479,
-0.00360989077465136));
#52266=CARTESIAN_POINT('Ctrl Pts',(-0.0264444422376895,0.000122963349712034,
-0.00359406200184561));
#52267=CARTESIAN_POINT('Ctrl Pts',(-0.0264726701882212,0.00012278141785782,
-0.00357752387041932));
#52268=CARTESIAN_POINT('Ctrl Pts',(-0.0264996579116161,0.000122607479386702,
-0.00356171236062163));
#52269=CARTESIAN_POINT('Ctrl Pts',(-0.0265266118581404,0.000122429453145089,
-0.00354592056709213));
#52270=CARTESIAN_POINT('Ctrl Pts',(-0.0265535379300483,0.000122247732016571,
-0.00353014495734327));
#52271=CARTESIAN_POINT('Ctrl Pts',(-0.02658023466759,0.000122067558640728,
-0.00351450371139899));
#52272=CARTESIAN_POINT('Ctrl Pts',(-0.0266069040078998,0.00012188375435418,
-0.00349887837252222));
#52273=CARTESIAN_POINT('Ctrl Pts',(-0.0266335514523883,0.000121696211892216,
-0.00348326543551233));
#52274=CARTESIAN_POINT('Ctrl Pts',(-0.0266600345193917,0.000121509826305098,
-0.00346774880850032));
#52275=CARTESIAN_POINT('Ctrl Pts',(-0.0266864959648013,0.000121319748016962,
-0.00345224442761254));
#52276=CARTESIAN_POINT('Ctrl Pts',(-0.0267129404584668,0.000121126029854152,
-0.00343674936402911));
#52277=CARTESIAN_POINT('Ctrl Pts',(-0.0267653682442451,0.000120741972043495,
-0.00340602947638643));
#52278=CARTESIAN_POINT('Ctrl Pts',(-0.0268177291022766,0.000120343614098467,
-0.00337534639126105));
#52279=CARTESIAN_POINT('Ctrl Pts',(-0.0268700516966129,0.000119931394892243,
-0.00334468198505257));
#52280=CARTESIAN_POINT('Ctrl Pts',(-0.0269218089411547,0.000119523629747338,
-0.00331434891019279));
#52281=CARTESIAN_POINT('Ctrl Pts',(-0.0269735288387845,0.000119102298826571,
-0.00328403405446561));
#52282=CARTESIAN_POINT('Ctrl Pts',(-0.0270252313788013,0.000118668086148498,
-0.00325372470877414));
#52283=CARTESIAN_POINT('Ctrl Pts',(-0.0270764227408043,0.000118238166489188,
-0.00322371502865278));
#52284=CARTESIAN_POINT('Ctrl Pts',(-0.0271275971424334,0.000117795617288825,
-0.00319371071572467));
#52285=CARTESIAN_POINT('Ctrl Pts',(-0.0271787707685532,0.000117341194417889,
-0.00316370145968983));
#52286=CARTESIAN_POINT('Ctrl Pts',(-0.0272797781160699,0.000116444247058001,
-0.00310446869502455));
#52287=CARTESIAN_POINT('Ctrl Pts',(-0.0273807806169518,0.00011550107514636,
-0.00304521774020601));
#52288=CARTESIAN_POINT('Ctrl Pts',(-0.0274818564446264,0.000114518630178686,
-0.00298589831181024));
#52289=CARTESIAN_POINT('Ctrl Pts',(-0.0275814324031909,0.000113550763759545,
-0.00292745912728996));
#52290=CARTESIAN_POINT('Ctrl Pts',(-0.0276810803813479,0.000112544768962472,
-0.00286895296322468));
#52291=CARTESIAN_POINT('Ctrl Pts',(-0.0277808389005263,0.000111508039264204,
-0.00281035472927768));
#52292=CARTESIAN_POINT('Ctrl Pts',(-0.0278794032326279,0.000110483720026896,
-0.00275245796177459));
#52293=CARTESIAN_POINT('Ctrl Pts',(-0.0279780759843496,0.000109429392354947,
-0.00269447100441981));
#52294=CARTESIAN_POINT('Ctrl Pts',(-0.0280768730639752,0.000108352484990015,
-0.0026363834400703));
#52295=CARTESIAN_POINT('Ctrl Pts',(-0.0281747495507818,0.000107285612265689,
-0.0025788371366044));
#52296=CARTESIAN_POINT('Ctrl Pts',(-0.028272748385646,0.000106196576723287,
-0.00252119189380465));
#52297=CARTESIAN_POINT('Ctrl Pts',(-0.0283708734488242,0.000105092655406102,
-0.00246344543367369));
#52298=CARTESIAN_POINT('Ctrl Pts',(-0.028565352107592,0.000102904742041281,
-0.00234899501956838));
#52299=CARTESIAN_POINT('Ctrl Pts',(-0.0287603242758405,0.000100658659497398,
-0.00223414774060621));
#52300=CARTESIAN_POINT('Ctrl Pts',(-0.0289556651769592,9.84109625647153E-5,
-0.00211898938119166));
#52301=CARTESIAN_POINT('Ctrl Pts',(-0.0291501751539627,9.61728266895183E-5,
-0.00200432087237855));
#52302=CARTESIAN_POINT('Ctrl Pts',(-0.0293450551540655,9.39331173919207E-5,
-0.00188934131721124));
#52303=CARTESIAN_POINT('Ctrl Pts',(-0.0295400270379856,9.17454444355415E-5,
-0.00177424100944673));
#52304=CARTESIAN_POINT('Ctrl Pts',(-0.0297359665809972,8.95469139053263E-5,
-0.00165856945080742));
#52305=CARTESIAN_POINT('Ctrl Pts',(-0.0299320019424413,8.74009587179148E-5,
-0.00154277419702442));
#52306=CARTESIAN_POINT('Ctrl Pts',(-0.0301277191821847,8.53581722133113E-5,
-0.00142713864495516));
#52307=CARTESIAN_POINT('Ctrl Pts',(-0.0303262937420681,8.32855626076416E-5,
-0.00130981490337201));
#52308=CARTESIAN_POINT('Ctrl Pts',(-0.0305245431904343,8.13191571505584E-5,
-0.00119265422654581));
#52309=CARTESIAN_POINT('Ctrl Pts',(-0.0307218894713725,7.95072456744465E-5,
-0.0010760502337852));
#52310=CARTESIAN_POINT('Ctrl Pts',(-0.0306647100227538,0.0133817289939493,
0.00107038503556915));
#52311=CARTESIAN_POINT('Ctrl Pts',(-0.0326595892334205,0.0123956391197582,
0.00151856505842931));
#52312=CARTESIAN_POINT('Ctrl Pts',(-0.0347612555974135,0.0120023262382354,
0.0022808544455469));
#52313=CARTESIAN_POINT('Ctrl Pts',(-0.030310636551541,0.0133810659960543,
0.00127926136827211));
#52314=CARTESIAN_POINT('Ctrl Pts',(-0.0323497877072503,0.0123587012333725,
0.00167896524445854));
#52315=CARTESIAN_POINT('Ctrl Pts',(-0.034504793762637,0.0119445902306563,
0.00241834291186082));
#52316=CARTESIAN_POINT('Ctrl Pts',(-0.0297913734877477,0.0133800176106531,
0.00158555997177866));
#52317=CARTESIAN_POINT('Ctrl Pts',(-0.0318905638771274,0.0123002313925209,
0.0019156374684094));
#52318=CARTESIAN_POINT('Ctrl Pts',(-0.0341203946096195,0.0118503203309816,
0.00262684653906666));
#52319=CARTESIAN_POINT('Ctrl Pts',(-0.0291134934790883,0.0133785311643582,
0.00198536147749519));
#52320=CARTESIAN_POINT('Ctrl Pts',(-0.0312684820519487,0.0122173215410984,
0.00223441391922514));
#52321=CARTESIAN_POINT('Ctrl Pts',(-0.0335750408273263,0.011704437060625,
0.00292061820949249));
#52322=CARTESIAN_POINT('Ctrl Pts',(-0.0286118977302727,0.0133773896440105,
0.0022811564471782));
#52323=CARTESIAN_POINT('Ctrl Pts',(-0.0307925845250482,0.01215366539174,
0.00247725318869305));
#52324=CARTESIAN_POINT('Ctrl Pts',(-0.0331409841609045,0.0115848853141045,
0.00315017909741456));
#52325=CARTESIAN_POINT('Ctrl Pts',(-0.0281126430422037,0.0133762319068543,
0.00257552991505409));
#52326=CARTESIAN_POINT('Ctrl Pts',(-0.0302988214468626,0.0120892008773578,
0.00272828796853001));
#52327=CARTESIAN_POINT('Ctrl Pts',(-0.0326684603969548,0.0114545241332851,
0.00339268193636275));
#52328=CARTESIAN_POINT('Ctrl Pts',(-0.0276951505456185,0.0133752613449626,
0.00282166534044536));
#52329=CARTESIAN_POINT('Ctrl Pts',(-0.0298640741459918,0.012035324868911,
0.00294920645759005));
#52330=CARTESIAN_POINT('Ctrl Pts',(-0.032228445307703,0.0113361163108333,
0.00361037592292299));
#52331=CARTESIAN_POINT('Ctrl Pts',(-0.0273575350888643,0.0133744837085808,
0.00302070115664028));
#52332=CARTESIAN_POINT('Ctrl Pts',(-0.029494718935472,0.0119923276822167,
0.00313769691396422));
#52333=CARTESIAN_POINT('Ctrl Pts',(-0.0318356844891301,0.0112346920460384,
0.00379925579609339));
#52334=CARTESIAN_POINT('Ctrl Pts',(-0.0271014943685578,0.0133738994060875,
0.00317164659443028));
#52335=CARTESIAN_POINT('Ctrl Pts',(-0.0292040699863256,0.0119601333248718,
0.00328676937427297));
#52336=CARTESIAN_POINT('Ctrl Pts',(-0.0315157814755496,0.0111548954586693,
0.00395056806280461));
#52337=CARTESIAN_POINT('Ctrl Pts',(-0.0268419576648391,0.0133733140263834,
0.00332465983562304));
#52338=CARTESIAN_POINT('Ctrl Pts',(-0.0288967835006665,0.0119280218878657,
0.00344558010096036));
#52339=CARTESIAN_POINT('Ctrl Pts',(-0.0311649277071802,0.0110710448872296,
0.00411429689112972));
#52340=CARTESIAN_POINT('Ctrl Pts',(-0.0266218956812325,0.0133728240133568,
0.00345441321228898));
#52341=CARTESIAN_POINT('Ctrl Pts',(-0.0286232624088187,0.0119012878231247,
0.00358846874310371));
#52342=CARTESIAN_POINT('Ctrl Pts',(-0.0308402062025501,0.0109973491206113,
0.00426454079291036));
#52343=CARTESIAN_POINT('Ctrl Pts',(-0.0264426154949514,0.013372428117788,
0.00356013525965011));
#52344=CARTESIAN_POINT('Ctrl Pts',(-0.0283904928968428,0.0118797957211661,
0.00371145103963453));
#52345=CARTESIAN_POINT('Ctrl Pts',(-0.0305548268488704,0.0109355978828558,
0.00439649850200783));
#52346=CARTESIAN_POINT('Ctrl Pts',(-0.0263062381182183,0.013372128177494,
0.00364056700768389));
#52347=CARTESIAN_POINT('Ctrl Pts',(-0.0282077567550798,0.0118635729881128,
0.00380883303996754));
#52348=CARTESIAN_POINT('Ctrl Pts',(-0.0303258278247013,0.0108877104255634,
0.00450262867601729));
#52349=CARTESIAN_POINT('Ctrl Pts',(-0.0261675735544255,0.013371823712976,
0.00372236023559422));
#52350=CARTESIAN_POINT('Ctrl Pts',(-0.0280153629006738,0.0118471690739344,
0.00391238329445619));
#52351=CARTESIAN_POINT('Ctrl Pts',(-0.0300792020978235,0.0108380258906879,
0.00461754277182759));
#52352=CARTESIAN_POINT('Ctrl Pts',(-0.0260497293451323,0.013371564385799,
0.00379188598430727));
#52353=CARTESIAN_POINT('Ctrl Pts',(-0.0278453661367971,0.0118332520622813,
0.00400492992782623));
#52354=CARTESIAN_POINT('Ctrl Pts',(-0.0298561034875484,0.010794879939539,
0.0047224470878419));
#52355=CARTESIAN_POINT('Ctrl Pts',(-0.0259537718308825,0.0133713518373242,
0.00384850991985681));
#52356=CARTESIAN_POINT('Ctrl Pts',(-0.0277022450165804,0.0118218790838674,
0.00408363726935057));
#52357=CARTESIAN_POINT('Ctrl Pts',(-0.029664710102224,0.0107591135472417,
0.00481341043608701));
#52358=CARTESIAN_POINT('Ctrl Pts',(-0.0258808773556986,0.0133711892996174,
0.00389153078810256));
#52359=CARTESIAN_POINT('Ctrl Pts',(-0.027590940482112,0.0118131989895311,
0.0041452868158749));
#52360=CARTESIAN_POINT('Ctrl Pts',(-0.0295139672710111,0.0107316023319646,
0.00488565938487552));
#52361=CARTESIAN_POINT('Ctrl Pts',(-0.0258069055623551,0.0133710227826421,
0.00393519478889492));
#52362=CARTESIAN_POINT('Ctrl Pts',(-0.0274751026803282,0.0118043218687226,
0.00420994459989036));
#52363=CARTESIAN_POINT('Ctrl Pts',(-0.0293550500899423,0.0107033104702102,
0.00496259135149595));
#52364=CARTESIAN_POINT('Ctrl Pts',(-0.0257443979892688,0.0133708802766567,
0.00397209877924601));
#52365=CARTESIAN_POINT('Ctrl Pts',(-0.027374523625404,0.0117967361445144,
0.00426655328520934));
#52366=CARTESIAN_POINT('Ctrl Pts',(-0.0292152465893807,0.0106790667286594,
0.00503106627065884));
#52367=CARTESIAN_POINT('Ctrl Pts',(-0.0256938523784136,0.0133707634325717,
0.00400194558902871));
#52368=CARTESIAN_POINT('Ctrl Pts',(-0.0272913586865124,0.0117905218792716,
0.00431368624165812));
#52369=CARTESIAN_POINT('Ctrl Pts',(-0.0290984582809993,0.0106592263497628,
0.00508887994392313));
#52370=CARTESIAN_POINT('Ctrl Pts',(-0.0256556496704833,0.0133706744705477,
0.00402450652784909));
#52371=CARTESIAN_POINT('Ctrl Pts',(-0.0272275704451228,0.0117857934129971,
0.00434999678655546));
#52372=CARTESIAN_POINT('Ctrl Pts',(-0.0290082867014547,0.0106441392730587,
0.0051338276680476));
#52373=CARTESIAN_POINT('Ctrl Pts',(-0.0256171358979087,0.0133705828336653,
0.00404725483162211));
#52374=CARTESIAN_POINT('Ctrl Pts',(-0.0271621083758112,0.0117809230482831,
0.00438748456117196));
#52375=CARTESIAN_POINT('Ctrl Pts',(-0.0289150444880619,0.0106286994218181,
0.00518076920054308));
#52376=CARTESIAN_POINT('Ctrl Pts',(-0.0255847661135387,0.0133705076531511,
0.00406637461446268));
#52377=CARTESIAN_POINT('Ctrl Pts',(-0.0271065553024961,0.011776932871555,
0.00441933156444236));
#52378=CARTESIAN_POINT('Ctrl Pts',(-0.0288355855642515,0.0106159367237068,
0.00522084688296197));
#52379=CARTESIAN_POINT('Ctrl Pts',(-0.025563606220307,0.0133704527601798,
0.00407887856220428));
#52380=CARTESIAN_POINT('Ctrl Pts',(-0.0270690596116852,0.0117740106014142,
0.00444114774412889));
#52381=CARTESIAN_POINT('Ctrl Pts',(-0.0287812858755557,0.010606945392152,
0.00524892446387147));
#52382=CARTESIAN_POINT('Ctrl Pts',(-0.0255538335707082,0.0133704327217964,
0.00408464950974319));
#52383=CARTESIAN_POINT('Ctrl Pts',(-0.0270523837722345,0.0117729523163032,
0.00445062705504254));
#52384=CARTESIAN_POINT('Ctrl Pts',(-0.028757478455657,0.0106034018291441,
0.00526077067671198));
#52385=CARTESIAN_POINT('Ctrl Pts',(-0.0255489142526789,0.0133704125322435,
0.00408756242539133));
#52386=CARTESIAN_POINT('Ctrl Pts',(-0.0270426052424206,0.0117718661395984,
0.00445665226233641));
#52387=CARTESIAN_POINT('Ctrl Pts',(-0.0287427442485597,0.0106004647633864,
0.00526909418370154));
#52388=CARTESIAN_POINT('Ctrl Pts',(-0.0255441020276982,0.0133704317568388,
0.00409038141371926));
#52389=CARTESIAN_POINT('Ctrl Pts',(-0.0270383028643863,0.0117729389486516,
0.00445776637193981));
#52390=CARTESIAN_POINT('Ctrl Pts',(-0.0287387840281493,0.010602043307318,
0.00526823762833236));
#52391=CARTESIAN_POINT('Ctrl Pts',(-0.0255360044973167,0.0133698094337739,
0.00409563689201563));
#52392=CARTESIAN_POINT('Ctrl Pts',(-0.026943593979902,0.0117389370272235,
0.00453928205208165));
#52393=CARTESIAN_POINT('Ctrl Pts',(-0.0285576641821581,0.0105285739785202,
0.00541515896656904));
#52394=CARTESIAN_POINT('Ctrl Pts',(-0.0255261811386256,0.0133692422925823,
0.00410186775774673));
#52395=CARTESIAN_POINT('Ctrl Pts',(-0.0268520852953097,0.0117078800431923,
0.00461653960126812));
#52396=CARTESIAN_POINT('Ctrl Pts',(-0.0283856961685775,0.0104635133099934,
0.00555576112810152));
#52397=CARTESIAN_POINT('Ctrl Pts',(-0.0255098110905591,0.0133682485098969,
0.00411229325548317));
#52398=CARTESIAN_POINT('Ctrl Pts',(-0.0266912899161765,0.0116533146508789,
0.00475265080476696));
#52399=CARTESIAN_POINT('Ctrl Pts',(-0.0280845894254988,0.0103533539204758,
0.00580828361020944));
#52400=CARTESIAN_POINT('Ctrl Pts',(-0.0254891046606487,0.013367200844991,
0.00412532497339551));
#52401=CARTESIAN_POINT('Ctrl Pts',(-0.0265144527206189,0.0115954690261533,
0.00490092637256455));
#52402=CARTESIAN_POINT('Ctrl Pts',(-0.02776023610422,0.0102447515300182,
0.00609008394105348));
#52403=CARTESIAN_POINT('Ctrl Pts',(-0.0254637875134938,0.0133661905625418,
0.00414105842990811));
#52404=CARTESIAN_POINT('Ctrl Pts',(-0.0263361898762663,0.0115393372750296,
0.00504907942993433));
#52405=CARTESIAN_POINT('Ctrl Pts',(-0.0274419161564073,0.0101475295589644,
0.00637658056716358));
#52406=CARTESIAN_POINT('Ctrl Pts',(-0.0254304056952004,0.013365133296662,
0.00416160141825757));
#52407=CARTESIAN_POINT('Ctrl Pts',(-0.0261404664461416,0.0114802432167385,
0.00521024801348284));
#52408=CARTESIAN_POINT('Ctrl Pts',(-0.027101818024583,0.0100526087199924,
0.00669107137676832));
#52409=CARTESIAN_POINT('Ctrl Pts',(-0.0253899454488653,0.0133641801502081,
0.00418626208550774));
#52410=CARTESIAN_POINT('Ctrl Pts',(-0.0259508778950532,0.0114265369067877,
0.00536445592173354));
#52411=CARTESIAN_POINT('Ctrl Pts',(-0.0267848099107839,0.00997513282770083,
0.0069935913376081));
#52412=CARTESIAN_POINT('Ctrl Pts',(-0.0253422237865103,0.0133633257894266,
0.00421515806069016));
#52413=CARTESIAN_POINT('Ctrl Pts',(-0.0257665514661048,0.0113780246677331,
0.00551263965393808));
#52414=CARTESIAN_POINT('Ctrl Pts',(-0.0264880543497171,0.00991229104416078,
0.00728329592444431));
#52415=CARTESIAN_POINT('Ctrl Pts',(-0.0252793983582859,0.0133624308307888,
0.00425304141213368));
#52416=CARTESIAN_POINT('Ctrl Pts',(-0.0255571101937992,0.0113268262759728,
0.00567935548445607));
#52417=CARTESIAN_POINT('Ctrl Pts',(-0.026162067728028,0.00985280585796018,
0.00760685205528419));
#52418=CARTESIAN_POINT('Ctrl Pts',(-0.0252036331342202,0.0133616279597208,
0.00429854296104807));
#52419=CARTESIAN_POINT('Ctrl Pts',(-0.0253443255750142,0.0112804205250411,
0.00584661692384335));
#52420=CARTESIAN_POINT('Ctrl Pts',(-0.025845297677816,0.00980768948825244,
0.00792673396362302));
#52421=CARTESIAN_POINT('Ctrl Pts',(-0.0251151268848991,0.0133609229335648,
0.00435154953715688));
#52422=CARTESIAN_POINT('Ctrl Pts',(-0.0251287969092761,0.0112392273586068,
0.00601421883870184));
#52423=CARTESIAN_POINT('Ctrl Pts',(-0.0255374031427373,0.00977586743792922,
0.00824070313324647));
#52424=CARTESIAN_POINT('Ctrl Pts',(-0.0249995654764944,0.0133602086920511,
0.00442063519669263));
#52425=CARTESIAN_POINT('Ctrl Pts',(-0.0248762138213547,0.0111970186426666,
0.00620898163584995));
#52426=CARTESIAN_POINT('Ctrl Pts',(-0.0251890442037446,0.00975199501094654,
0.00859766578095785));
#52427=CARTESIAN_POINT('Ctrl Pts',(-0.0248582632791613,0.013359600841859,
0.00450495748155972));
#52428=CARTESIAN_POINT('Ctrl Pts',(-0.0246042039362115,0.0111604345286657,
0.00641664815771456));
#52429=CARTESIAN_POINT('Ctrl Pts',(-0.0248301609530199,0.00974444741096367,
0.0089658885633592));
#52430=CARTESIAN_POINT('Ctrl Pts',(-0.0246380149274922,0.0133589809712524,
0.00463621895950101));
#52431=CARTESIAN_POINT('Ctrl Pts',(-0.0242247526957397,0.0111221183806697,
0.00670401640032051));
#52432=CARTESIAN_POINT('Ctrl Pts',(-0.0243497852666751,0.00975742460170551,
0.00945556192448081));
#52433=CARTESIAN_POINT('Ctrl Pts',(-0.0243729338683078,0.0133586358239313,
0.00479400285784582));
#52434=CARTESIAN_POINT('Ctrl Pts',(-0.0238222364174371,0.0110991446822809,
0.007006206123228));
#52435=CARTESIAN_POINT('Ctrl Pts',(-0.023864787508101,0.00980148850514733,
0.0099415894121633));
#52436=CARTESIAN_POINT('Ctrl Pts',(-0.0240639991262786,0.0133585753914925,
0.00497773811248542));
#52437=CARTESIAN_POINT('Ctrl Pts',(-0.023398651500273,0.0110923841763263,
0.00732222080231654));
#52438=CARTESIAN_POINT('Ctrl Pts',(-0.0233741410159405,0.00987436526268883,
0.0104191227673781));
#52439=CARTESIAN_POINT('Ctrl Pts',(-0.0237616794738991,0.0133587454597912,
0.00515743938209382));
#52440=CARTESIAN_POINT('Ctrl Pts',(-0.0230144604738983,0.0110993286290909,
0.00760734303674687));
#52441=CARTESIAN_POINT('Ctrl Pts',(-0.0229421337902909,0.00995878657650268,
0.0108259647819836));
#52442=CARTESIAN_POINT('Ctrl Pts',(-0.0233649946146776,0.0133591848020346,
0.00539313616345824));
#52443=CARTESIAN_POINT('Ctrl Pts',(-0.0225386758600217,0.0111213569246464,
0.00795867594547827));
#52444=CARTESIAN_POINT('Ctrl Pts',(-0.02241894455993,0.0100805004122373,
0.0113016788678717));
#52445=CARTESIAN_POINT('Ctrl Pts',(-0.0228780788425745,0.0133600265415265,
0.00568230081805398));
#52446=CARTESIAN_POINT('Ctrl Pts',(-0.0219945592608549,0.0111665834138114,
0.00835711336133469));
#52447=CARTESIAN_POINT('Ctrl Pts',(-0.0218358028786606,0.0102431535003208,
0.0118023917664635));
#52448=CARTESIAN_POINT('Ctrl Pts',(-0.022305766431248,0.0133613156346166,
0.00602199835405312));
#52449=CARTESIAN_POINT('Ctrl Pts',(-0.0213938782142982,0.0112378915781148,
0.00879089397721249));
#52450=CARTESIAN_POINT('Ctrl Pts',(-0.0212055476440137,0.0104431187383345,
0.0123039181617212));
#52451=CARTESIAN_POINT('Ctrl Pts',(-0.0219292577234598,0.0133623030344497,
0.00624536295715626));
#52452=CARTESIAN_POINT('Ctrl Pts',(-0.0210163471587063,0.0112932429550283,
0.00905875420573385));
#52453=CARTESIAN_POINT('Ctrl Pts',(-0.0208154213726988,0.010576673703214,
0.0125909030789934));
#52454=CARTESIAN_POINT('Ctrl Pts',(-0.0217418465582972,0.013362819665371,
0.00635651709279996));
#52455=CARTESIAN_POINT('Ctrl Pts',(-0.0208314744349912,0.0113223146764728,
0.00918856807479045));
#52456=CARTESIAN_POINT('Ctrl Pts',(-0.0206254586057132,0.010643066208173,
0.0127253928900171));
#52457=CARTESIAN_POINT('',(-0.0217848380421749,0.0133386308183493,0.00635794497981714));
#52458=CARTESIAN_POINT('Ctrl Pts',(-0.0311805491196909,0.0110755203513828,
0.00410667728630412));
#52459=CARTESIAN_POINT('Ctrl Pts',(-0.0303628462213495,0.0110536005240181,
0.00427642982102741));
#52460=CARTESIAN_POINT('Ctrl Pts',(-0.0291450767836391,0.0111156395935359,
0.00451528869049828));
#52461=CARTESIAN_POINT('Ctrl Pts',(-0.0275504601453372,0.0113532710676122,
0.00486779796847178));
#52462=CARTESIAN_POINT('Ctrl Pts',(-0.0259696456997476,0.0118045993808991,
0.00517760956883624));
#52463=CARTESIAN_POINT('Ctrl Pts',(-0.0240886530202461,0.0125793024532316,
0.00570384378960105));
#52464=CARTESIAN_POINT('Ctrl Pts',(-0.0225643752139947,0.0131235232054828,
0.00613182294147269));
#52465=CARTESIAN_POINT('Ctrl Pts',(-0.0217848380421749,0.0133386308183493,
0.00635794497981714));
#52466=CARTESIAN_POINT('',(-0.0227510611416183,0.0133301029619171,0.00578783038319825));
#52467=CARTESIAN_POINT('Ctrl Pts',(-0.0227510611416183,0.0133301029619171,
0.00578783038319825));
#52468=CARTESIAN_POINT('Ctrl Pts',(-0.0225988241462555,0.0133314270627633,
0.00587773671841089));
#52469=CARTESIAN_POINT('Ctrl Pts',(-0.0224468599320209,0.0133327705039863,
0.00596743869532409));
#52470=CARTESIAN_POINT('Ctrl Pts',(-0.0222953888501995,0.0133341234933048,
0.00605680312827367));
#52471=CARTESIAN_POINT('Ctrl Pts',(-0.0221243986305164,0.0133356508339562,
0.00615768340085212));
#52472=CARTESIAN_POINT('Ctrl Pts',(-0.0219540318556272,0.0133371902973775,
0.00625813645800992));
#52473=CARTESIAN_POINT('Ctrl Pts',(-0.0217847944705363,0.0133387336320324,
0.00635785581245878));
#52474=CARTESIAN_POINT('',(-0.0264065477674619,0.0133196469578813,0.0036268963164667));
#52475=CARTESIAN_POINT('Ctrl Pts',(-0.0264065477674619,0.0133196469578813,
0.00362689631646671));
#52476=CARTESIAN_POINT('Ctrl Pts',(-0.026394716629658,0.0133195174636387,
0.00363389128041229));
#52477=CARTESIAN_POINT('Ctrl Pts',(-0.0263834986769066,0.013319395206925,
0.00364052343157509));
#52478=CARTESIAN_POINT('Ctrl Pts',(-0.0263727080949494,0.0133192784627222,
0.00364690234370207));
#52479=CARTESIAN_POINT('Ctrl Pts',(-0.0263512398831163,0.0133190461963545,
0.0036595933957093));
#52480=CARTESIAN_POINT('Ctrl Pts',(-0.0263314663061818,0.0133188357788058,
0.00367128027334653));
#52481=CARTESIAN_POINT('Ctrl Pts',(-0.0263118834379465,0.0133186332101986,
0.00368285016275895));
#52482=CARTESIAN_POINT('Ctrl Pts',(-0.0262971705286196,0.0133184810172965,
0.00369154279816876));
#52483=CARTESIAN_POINT('Ctrl Pts',(-0.0262825684258451,0.0133183333998923,
0.00370016757369084));
#52484=CARTESIAN_POINT('Ctrl Pts',(-0.0262751672873967,0.0133182556390686,
0.00370454166801996));
#52485=CARTESIAN_POINT('Ctrl Pts',(-0.0262677661489483,0.0133181778782449,
0.00370891576234908));
#52486=CARTESIAN_POINT('Ctrl Pts',(-0.0262675658719951,0.0133181696127009,
0.00370903898435915));
#52487=CARTESIAN_POINT('Ctrl Pts',(-0.0262455282347752,0.0133179638674093,
0.00372204245026586));
#52488=CARTESIAN_POINT('Ctrl Pts',(-0.0262418372101996,0.0133179294076838,
0.00372422036579057));
#52489=CARTESIAN_POINT('Ctrl Pts',(-0.026237536410453,0.0133178894691057,
0.00372675793654771));
#52490=CARTESIAN_POINT('Ctrl Pts',(-0.0262327486899822,0.013317845278354,
0.00372958264011147));
#52491=CARTESIAN_POINT('Ctrl Pts',(-0.0262089508389711,0.0133176256237332,
0.00374362311615229));
#52492=CARTESIAN_POINT('Ctrl Pts',(-0.0261730618794819,0.0133173003171878,
0.0037647942828713));
#52493=CARTESIAN_POINT('Ctrl Pts',(-0.0261404843237304,0.0133170230323306,
0.00378400090645341));
#52494=CARTESIAN_POINT('Ctrl Pts',(-0.0261226794117806,0.0133168714852807,
0.00379449807954832));
#52495=CARTESIAN_POINT('Ctrl Pts',(-0.0261058493888371,0.0133167338782244,
0.00380441680035033));
#52496=CARTESIAN_POINT('Ctrl Pts',(-0.0260893950595296,0.0133166044095186,
0.00381411086136281));
#52497=CARTESIAN_POINT('Ctrl Pts',(-0.0260696860942685,0.0133164493321419,
0.00382572238974317));
#52498=CARTESIAN_POINT('Ctrl Pts',(-0.0260505173670805,0.0133163059437924,
0.00383701085155254));
#52499=CARTESIAN_POINT('Ctrl Pts',(-0.0260308178878044,0.0133161638331711,
0.00384860916443173));
#52500=CARTESIAN_POINT('Ctrl Pts',(-0.0260259891081691,0.0133161289987034,
0.00385145216836346));
#52501=CARTESIAN_POINT('Ctrl Pts',(-0.0260211296759531,0.0133160942559615,
0.00385431305907611));
#52502=CARTESIAN_POINT('Ctrl Pts',(-0.0260162408533954,0.0133160596206651,
0.00385719109461294));
#52503=CARTESIAN_POINT('Ctrl Pts',(-0.0259921529245199,0.0133158889675996,
0.00387137158786942));
#52504=CARTESIAN_POINT('Ctrl Pts',(-0.0259673511316601,0.0133157209193171,
0.00388596851921629));
#52505=CARTESIAN_POINT('Ctrl Pts',(-0.0259419782668339,0.0133155572563812,
0.00390089801887217));
#52506=CARTESIAN_POINT('Ctrl Pts',(-0.0259172996240843,0.0133153980713955,
0.00391541903535815));
#52507=CARTESIAN_POINT('Ctrl Pts',(-0.02589208018466,0.0133152430298302,
0.00393025499756256));
#52508=CARTESIAN_POINT('Ctrl Pts',(-0.0258664910751612,0.013315094022236,
0.00394530533415525));
#52509=CARTESIAN_POINT('Ctrl Pts',(-0.0258437895321223,0.0133149618291905,
0.00395865733704245));
#52510=CARTESIAN_POINT('Ctrl Pts',(-0.0258207972354934,0.0133148343859008,
0.00397217795015615));
#52511=CARTESIAN_POINT('Ctrl Pts',(-0.0257976307872261,0.0133147128628802,
0.00398579869902889));
#52512=CARTESIAN_POINT('Ctrl Pts',(-0.0257815941249314,0.0133146287402033,
0.00399522747927838));
#52513=CARTESIAN_POINT('Ctrl Pts',(-0.0257659133899357,0.0133146836001378,
0.00400433856955475));
#52514=CARTESIAN_POINT('Ctrl Pts',(-0.0257505285264267,0.0133148550678093,
0.00401318621280172));
#52515=CARTESIAN_POINT('Ctrl Pts',(-0.0257369531148523,0.013315006368743,
0.00402099326279412));
#52516=CARTESIAN_POINT('Ctrl Pts',(-0.025723607921997,0.0133152484333549,
0.00402859528929107));
#52517=CARTESIAN_POINT('Ctrl Pts',(-0.0257104486655114,0.01331556493994,
0.00403603178733425));
#52518=CARTESIAN_POINT('Ctrl Pts',(-0.02569662428812,0.0133158974440206,
0.00404384415542149));
#52519=CARTESIAN_POINT('Ctrl Pts',(-0.0256830052830809,0.0133163121828292,
0.00405147368002277));
#52520=CARTESIAN_POINT('Ctrl Pts',(-0.0256695407622072,0.0133167925088795,
0.0040589638258519));
#52521=CARTESIAN_POINT('Ctrl Pts',(-0.0256555101539921,0.013317293029224,
0.00406676887904234));
#52522=CARTESIAN_POINT('Ctrl Pts',(-0.0256416470042577,0.0133178645117327,
0.00407442295752445));
#52523=CARTESIAN_POINT('Ctrl Pts',(-0.0256278835755066,0.013318478517641,
0.004081988529265));
#52524=CARTESIAN_POINT('Ctrl Pts',(-0.0256208342766697,0.0133187929967736,
0.00408586343406058));
#52525=CARTESIAN_POINT('Ctrl Pts',(-0.0256138113920498,0.0133191187798247,
0.00408971485050543));
#52526=CARTESIAN_POINT('Ctrl Pts',(-0.025606829280161,0.0133194621940564,
0.00409352939535447));
#52527=CARTESIAN_POINT('Ctrl Pts',(-0.0256033059204389,0.0133196354900292,
0.00409545431633727));
#52528=CARTESIAN_POINT('Ctrl Pts',(-0.025599720549853,0.0133197857610566,
0.00409743396679169));
#52529=CARTESIAN_POINT('Ctrl Pts',(-0.0255962542995072,0.0133199819038571,
0.00409930787760123));
#52530=CARTESIAN_POINT('Ctrl Pts',(-0.0255927708341416,0.0133201790207944,
0.00410119109512799));
#52531=CARTESIAN_POINT('Ctrl Pts',(-0.0255882443720757,0.0133199524295486,
0.00410401805778399));
#52532=CARTESIAN_POINT('Ctrl Pts',(-0.0255828256013243,0.0133193965594662,
0.00410762851133424));
#52533=CARTESIAN_POINT('Ctrl Pts',(-0.0255773850046021,0.0133188384504251,
0.00411125350723321));
#52534=CARTESIAN_POINT('Ctrl Pts',(-0.0255722675677563,0.0133184406762622,
0.0041145654139126));
#52535=CARTESIAN_POINT('Ctrl Pts',(-0.0255670336542669,0.0133180207611486,
0.00411796495422484));
#52536=CARTESIAN_POINT('Ctrl Pts',(-0.0255617837093089,0.0133175995598357,
0.00412137490732359));
#52537=CARTESIAN_POINT('Ctrl Pts',(-0.0255564191556313,0.0133171571293206,
0.00412487069938319));
#52538=CARTESIAN_POINT('Ctrl Pts',(-0.0255511062565089,0.0133167559324299,
0.00412830573725567));
#52539=CARTESIAN_POINT('Ctrl Pts',(-0.0255404526285013,0.0133159514371192,
0.00413519380624443));
#52540=CARTESIAN_POINT('Ctrl Pts',(-0.0255300037364794,0.013315311428736,
0.00414184032636662));
#52541=CARTESIAN_POINT('Ctrl Pts',(-0.0255196915273417,0.0133147951582003,
0.00414831527807117));
#52542=CARTESIAN_POINT('Ctrl Pts',(-0.0255093777785549,0.0133142788105836,
0.00415479119650885));
#52543=CARTESIAN_POINT('Ctrl Pts',(-0.0254992007062769,0.0133138863721156,
0.00416109542777311));
#52544=CARTESIAN_POINT('Ctrl Pts',(-0.0254892398687713,0.0133135951681441,
0.00416719731466131));
#52545=CARTESIAN_POINT('Ctrl Pts',(-0.025479317298874,0.0133133050829218,
0.00417327575928203));
#52546=CARTESIAN_POINT('Ctrl Pts',(-0.0254696091039602,0.0133131154472376,
0.00417915354185311));
#52547=CARTESIAN_POINT('Ctrl Pts',(-0.0254600820614871,0.0133129889108621,
0.00418487821075715));
#52548=CARTESIAN_POINT('Ctrl Pts',(-0.0254412823347847,0.0133127392164493,
0.00419617470819175));
#52549=CARTESIAN_POINT('Ctrl Pts',(-0.0254231884885536,0.0133127349632696,
0.00420687487902349));
#52550=CARTESIAN_POINT('Ctrl Pts',(-0.0254052540728127,0.0133128084471708,
0.00421742822975724));
#52551=CARTESIAN_POINT('Ctrl Pts',(-0.0253878400671775,0.0133128797987603,
0.00422767534969703));
#52552=CARTESIAN_POINT('Ctrl Pts',(-0.0253705767865013,0.0133130248895279,
0.00423778347418303));
#52553=CARTESIAN_POINT('Ctrl Pts',(-0.0253532413158221,0.0133131683409094,
0.00424794200591349));
#52554=CARTESIAN_POINT('Ctrl Pts',(-0.0253365992332474,0.0133133060544899,
0.00425769421437813));
#52555=CARTESIAN_POINT('Ctrl Pts',(-0.0253198883280054,0.0133134423171085,
0.00426749419583593));
#52556=CARTESIAN_POINT('Ctrl Pts',(-0.0253030695365654,0.0133135281161507,
0.00427740269087294));
#52557=CARTESIAN_POINT('Ctrl Pts',(-0.025294225752135,0.0133135732316535,
0.00428261285085673));
#52558=CARTESIAN_POINT('Ctrl Pts',(-0.0252853528909199,0.0133136043649565,
0.00428785259469544));
#52559=CARTESIAN_POINT('Ctrl Pts',(-0.0252764301019966,0.0133136158059306,
0.00429313878769495));
#52560=CARTESIAN_POINT('Ctrl Pts',(-0.0252535722047203,0.0133136451147725,
0.00430668065869561));
#52561=CARTESIAN_POINT('Ctrl Pts',(-0.0252306241532069,0.0133137059755598,
0.00432025962806135));
#52562=CARTESIAN_POINT('Ctrl Pts',(-0.0252074780937085,0.0133137741353841,
0.00433395707742505));
#52563=CARTESIAN_POINT('Ctrl Pts',(-0.0251772875882765,0.0133138630394823,
0.0043518233116083));
#52564=CARTESIAN_POINT('Ctrl Pts',(-0.0251467570318961,0.0133139639258754,
0.00436989333476208));
#52565=CARTESIAN_POINT('Ctrl Pts',(-0.0251158775334444,0.0133140652437999,
0.0043881799678752));
#52566=CARTESIAN_POINT('Ctrl Pts',(-0.0250865312992789,0.0133141615309705,
0.00440555861210011));
#52567=CARTESIAN_POINT('Ctrl Pts',(-0.0250568693955269,0.0133142579509085,
0.00442313337980284));
#52568=CARTESIAN_POINT('Ctrl Pts',(-0.0250268673250634,0.0133143510110433,
0.00444092051686331));
#52569=CARTESIAN_POINT('Ctrl Pts',(-0.0249703190496052,0.0133145264119425,
0.00447444593396187));
#52570=CARTESIAN_POINT('Ctrl Pts',(-0.0249125598664124,0.0133146903323235,
0.00450872724959347));
#52571=CARTESIAN_POINT('Ctrl Pts',(-0.0248539896070711,0.0133148787353483,
0.00454349276756054));
#52572=CARTESIAN_POINT('Ctrl Pts',(-0.0247974986888213,0.013315060449754,
0.00457702405213189));
#52573=CARTESIAN_POINT('Ctrl Pts',(-0.0247402504940931,0.0133152640973943,
0.00461100801798857));
#52574=CARTESIAN_POINT('Ctrl Pts',(-0.024682654870725,0.0133155440084415,
0.00464515093357176));
#52575=CARTESIAN_POINT('Ctrl Pts',(-0.0245787095346326,0.0133160491761292,
0.00470677014398967));
#52576=CARTESIAN_POINT('Ctrl Pts',(-0.0244727850114969,0.0133166393006272,
0.00476954594658457));
#52577=CARTESIAN_POINT('Ctrl Pts',(-0.024358237683565,0.0133173697130724,
0.00483738766158962));
#52578=CARTESIAN_POINT('Ctrl Pts',(-0.0242573494148497,0.0133180130283586,
0.0048971396723708));
#52579=CARTESIAN_POINT('Ctrl Pts',(-0.024149732020381,0.0133187647412866,
0.00496084760167406));
#52580=CARTESIAN_POINT('Ctrl Pts',(-0.0240537247169841,0.013319470739504,
0.00501766384229477));
#52581=CARTESIAN_POINT('Ctrl Pts',(-0.0240407264818175,0.0133195663231787,
0.00502535607851787));
#52582=CARTESIAN_POINT('Ctrl Pts',(-0.0240279382978251,0.0133196609048211,
0.00503292375035051));
#52583=CARTESIAN_POINT('Ctrl Pts',(-0.0240154037824746,0.0133197540155003,
0.00504034113731551));
#52584=CARTESIAN_POINT('Ctrl Pts',(-0.0239174314892982,0.0133204817872973,
0.00509831692576976));
#52585=CARTESIAN_POINT('Ctrl Pts',(-0.0238351585444195,0.0133211275768285,
0.00514698203734017));
#52586=CARTESIAN_POINT('Ctrl Pts',(-0.0237503321966176,0.0133217980683467,
0.00519715584830999));
#52587=CARTESIAN_POINT('Ctrl Pts',(-0.0237441464273266,0.0133218469624221,
0.00520081465983675));
#52588=CARTESIAN_POINT('Ctrl Pts',(-0.0237379476838069,0.0133218960232413,
0.00520448110756548));
#52589=CARTESIAN_POINT('Ctrl Pts',(-0.0237317291711661,0.0133219453089548,
0.00520815920566391));
#52590=CARTESIAN_POINT('Ctrl Pts',(-0.0236402352964382,0.0133226704567771,
0.00526227559427542));
#52591=CARTESIAN_POINT('Ctrl Pts',(-0.0235443118153809,0.0133234371794813,
0.0053190105854227));
#52592=CARTESIAN_POINT('Ctrl Pts',(-0.0234494523212224,0.0133242089308042,
0.0053751038212117));
#52593=CARTESIAN_POINT('Ctrl Pts',(-0.0232597333329052,0.01332575243345,
0.00548729029278969));
#52594=CARTESIAN_POINT('Ctrl Pts',(-0.0230742704576996,0.0133273148826671,
0.0055969100218233));
#52595=CARTESIAN_POINT('Ctrl Pts',(-0.0228890601614922,0.013328908902742,
0.00570632078071611));
#52596=CARTESIAN_POINT('Ctrl Pts',(-0.0228819374396055,0.0133289702047425,
0.00571052844315698));
#52597=CARTESIAN_POINT('Ctrl Pts',(-0.0228748151351252,0.0133290315567097,
0.00571473576617383));
#52598=CARTESIAN_POINT('Ctrl Pts',(-0.0228676932904643,0.0133290929561784,
0.00571894272488699));
#52599=CARTESIAN_POINT('Ctrl Pts',(-0.0228288007996344,0.0133294282595149,
0.00574191698379919));
#52600=CARTESIAN_POINT('Ctrl Pts',(-0.022789922488709,0.0133297649870326,
0.00576488010001121));
#52601=CARTESIAN_POINT('Ctrl Pts',(-0.0227510611416183,0.0133301029619171,
0.00578783038319825));
#52602=CARTESIAN_POINT('',(-0.0307012608623869,0.0133637168977234,0.00107862162231056));
#52603=CARTESIAN_POINT('Ctrl Pts',(-0.0307012608623869,0.0133637168977234,
0.00107862162231056));
#52604=CARTESIAN_POINT('Ctrl Pts',(-0.0303353115612717,0.0133609145128637,
0.00129643444327742));
#52605=CARTESIAN_POINT('Ctrl Pts',(-0.029992089042177,0.0133579810772048,
0.00150062793971989));
#52606=CARTESIAN_POINT('Ctrl Pts',(-0.0296705263034281,0.0133550150323022,
0.00169181816446555));
#52607=CARTESIAN_POINT('Ctrl Pts',(-0.0294963157598973,0.0133534081412282,
0.00179539780525453));
#52608=CARTESIAN_POINT('Ctrl Pts',(-0.0293284943915401,0.0133517923054471,
0.00189514229389304));
#52609=CARTESIAN_POINT('Ctrl Pts',(-0.0291673512431136,0.0133501910488438,
0.00199087949557486));
#52610=CARTESIAN_POINT('Ctrl Pts',(-0.0290793930908137,0.0133493170211637,
0.00204313655675635));
#52611=CARTESIAN_POINT('Ctrl Pts',(-0.0289934229671365,0.0133484473481551,
0.00209420070809991));
#52612=CARTESIAN_POINT('Ctrl Pts',(-0.0289094017947271,0.013347585513257,
0.00214409491897803));
#52613=CARTESIAN_POINT('Ctrl Pts',(-0.0288277133008652,0.0133467476054682,
0.00219260391762897));
#52614=CARTESIAN_POINT('Ctrl Pts',(-0.0287479234814482,0.0133459165378698,
0.00223997497994222));
#52615=CARTESIAN_POINT('Ctrl Pts',(-0.0286699811757669,0.0133450946198445,
0.00228623902273471));
#52616=CARTESIAN_POINT('Ctrl Pts',(-0.0284956456525509,0.0133432562150435,
0.00238971897544866));
#52617=CARTESIAN_POINT('Ctrl Pts',(-0.0283305220174397,0.0133414637385238,
0.00248767895134269));
#52618=CARTESIAN_POINT('Ctrl Pts',(-0.0281744805302891,0.0133397409158217,
0.00258020890118065));
#52619=CARTESIAN_POINT('Ctrl Pts',(-0.0279964830986621,0.0133377756819488,
0.00268575835293535));
#52620=CARTESIAN_POINT('Ctrl Pts',(-0.0278302789703917,0.0133359010791335,
0.00278425701312616));
#52621=CARTESIAN_POINT('Ctrl Pts',(-0.0276761673782987,0.0133341465135724,
0.00287555202195714));
#52622=CARTESIAN_POINT('Ctrl Pts',(-0.0276397484012646,0.0133337318823172,
0.00289712645892705));
#52623=CARTESIAN_POINT('Ctrl Pts',(-0.0276040084430913,0.0133333239399807,
0.00291829640020815));
#52624=CARTESIAN_POINT('Ctrl Pts',(-0.0275689538164303,0.0133329230132978,
0.00293905844958548));
#52625=CARTESIAN_POINT('Ctrl Pts',(-0.0275193315674378,0.0133323554738435,
0.00296844856672347));
#52626=CARTESIAN_POINT('Ctrl Pts',(-0.0274710620702214,0.013331801765515,
0.00299703350333233));
#52627=CARTESIAN_POINT('Ctrl Pts',(-0.0274241340969779,0.0133312624917841,
0.00302482064625548));
#52628=CARTESIAN_POINT('Ctrl Pts',(-0.0273341082830727,0.0133302279583666,
0.00307812702164006));
#52629=CARTESIAN_POINT('Ctrl Pts',(-0.02724901697524,0.0133292465851678,
0.00312849901069747));
#52630=CARTESIAN_POINT('Ctrl Pts',(-0.0271689222567074,0.0133283225186183,
0.00317590502138782));
#52631=CARTESIAN_POINT('Ctrl Pts',(-0.0271344513707912,0.0133279248220762,
0.00319630745510868));
#52632=CARTESIAN_POINT('Ctrl Pts',(-0.027100906699519,0.0133275377318371,
0.0032161600660394));
#52633=CARTESIAN_POINT('Ctrl Pts',(-0.0270682927695371,0.0133271615071192,
0.00323546053550353));
#52634=CARTESIAN_POINT('Ctrl Pts',(-0.0270127281719848,0.0133265205302405,
0.00326834289034221));
#52635=CARTESIAN_POINT('Ctrl Pts',(-0.0269598553070662,0.0133259110090293,
0.00329962843520989));
#52636=CARTESIAN_POINT('Ctrl Pts',(-0.0269096234083803,0.0133253331845922,
0.00332934846738256));
#52637=CARTESIAN_POINT('Ctrl Pts',(-0.0268261533736523,0.0133243730173061,
0.00337873406065028));
#52638=CARTESIAN_POINT('Ctrl Pts',(-0.0267499648859122,0.0133235003201201,
0.00342380352386417));
#52639=CARTESIAN_POINT('Ctrl Pts',(-0.0266808066024393,0.013322714655098,
0.00346470917922637));
#52640=CARTESIAN_POINT('Ctrl Pts',(-0.026668629363042,0.0133225763169181,
0.00347191175761667));
#52641=CARTESIAN_POINT('Ctrl Pts',(-0.0266566706260414,0.0133224406803111,
0.00347898491250738));
#52642=CARTESIAN_POINT('Ctrl Pts',(-0.026644935364075,0.0133223077955545,
0.00348592572439474));
#52643=CARTESIAN_POINT('Ctrl Pts',(-0.0265959129162677,0.0133217526877038,
0.00351492001437869));
#52644=CARTESIAN_POINT('Ctrl Pts',(-0.0265507866300319,0.0133212455758331,
0.00354160707007658));
#52645=CARTESIAN_POINT('Ctrl Pts',(-0.0265099328376447,0.0133207900375879,
0.00356576558784225));
#52646=CARTESIAN_POINT('Ctrl Pts',(-0.02647159868028,0.0133203625944116,
0.00358843414240255));
#52647=CARTESIAN_POINT('Ctrl Pts',(-0.0264370276338154,0.0133199805663026,
0.00360887560115242));
#52648=CARTESIAN_POINT('Ctrl Pts',(-0.0264065477674619,0.0133196469578813,
0.00362689631646671));
#52649=CARTESIAN_POINT('Origin',(-0.0350444526050681,0.0256340492967854,
0.00853352794652652));
#52650=CARTESIAN_POINT('Ctrl Pts',(-0.0346818054102186,0.0119846858024896,
0.00232257533643425));
#52651=CARTESIAN_POINT('Ctrl Pts',(-0.0325963194414617,0.0123976569665182,
0.00153734729870167));
#52652=CARTESIAN_POINT('Ctrl Pts',(-0.03061725147117,0.0133985938507509,
0.00107061716078679));
#52653=CARTESIAN_POINT('Ctrl Pts',(-0.0354361330509732,0.0121509732395146,
0.00193216893213736));
#52654=CARTESIAN_POINT('Ctrl Pts',(-0.0330226689375074,0.0124110180713967,
0.00129825859323519));
#52655=CARTESIAN_POINT('Ctrl Pts',(-0.0307425222934407,0.0133986155780547,
0.000998140594337429));
#52656=CARTESIAN_POINT('Ctrl Pts',(-0.036011215516007,0.0123500627020912,
0.00135104585411375));
#52657=CARTESIAN_POINT('Ctrl Pts',(-0.033395569122503,0.0124397950591077,
0.000973263036901243));
#52658=CARTESIAN_POINT('Ctrl Pts',(-0.0309408025410812,0.0133986581242847,
0.000852236643677883));
#52659=CARTESIAN_POINT('Ctrl Pts',(-0.0363091803430268,0.0124790671617841,
0.000573007463839057));
#52660=CARTESIAN_POINT('Ctrl Pts',(-0.0336656182136692,0.0124888897140569,
0.000449578966366591));
#52661=CARTESIAN_POINT('Ctrl Pts',(-0.0311818867874813,0.0133987267804568,
0.000433853907110055));
#52662=CARTESIAN_POINT('Ctrl Pts',(-0.0363699702965885,0.0125113195748914,
1.02558394175085E-6));
#52663=CARTESIAN_POINT('Ctrl Pts',(-0.0337391428303402,0.0125064594535196,
5.56793826959371E-7));
#52664=CARTESIAN_POINT('Ctrl Pts',(-0.0312650822031905,0.0133987511234855,
1.37775683656485E-7));
#52665=CARTESIAN_POINT('Ctrl Pts',(-0.0363114929505171,0.0124788561197549,
-0.000573062348264479));
#52666=CARTESIAN_POINT('Ctrl Pts',(-0.0336665459476314,0.0124883464178191,
-0.00044988160607198));
#52667=CARTESIAN_POINT('Ctrl Pts',(-0.0311815545155191,0.0133987260406928,
-0.000434839939525983));
#52668=CARTESIAN_POINT('Ctrl Pts',(-0.0360173256313817,0.0123499454800039,
-0.00134821109832071));
#52669=CARTESIAN_POINT('Ctrl Pts',(-0.0333986737828021,0.0124387380183363,
-0.000971258174768614));
#52670=CARTESIAN_POINT('Ctrl Pts',(-0.0309411737711407,0.0133986566920038,
-0.000851300456162731));
#52671=CARTESIAN_POINT('Ctrl Pts',(-0.0354494076621593,0.0121512055067501,
-0.0019289935218175));
#52672=CARTESIAN_POINT('Ctrl Pts',(-0.0330293516321701,0.0124093950736726,
-0.00129574422396878));
#52673=CARTESIAN_POINT('Ctrl Pts',(-0.0307431403215359,0.0133986133925361,
-0.000997812178750743));
#52674=CARTESIAN_POINT('Ctrl Pts',(-0.0346932848386117,0.0119831034613695,
-0.00232183549083736));
#52675=CARTESIAN_POINT('Ctrl Pts',(-0.0326018426404496,0.0123955015963908,
-0.00153607898158788));
#52676=CARTESIAN_POINT('Ctrl Pts',(-0.0306171897688803,0.0133985909035257,
-0.00107065436122431));
#52677=CARTESIAN_POINT('',(-0.0307004248295923,0.0133627434399838,-0.00107761006352919));
#52678=CARTESIAN_POINT('Ctrl Pts',(-0.0307017856734144,0.0133639656227132,
-0.00107885621208017));
#52679=CARTESIAN_POINT('Ctrl Pts',(-0.0309758135796404,0.0133799891925163,
-0.000888980768471492));
#52680=CARTESIAN_POINT('Ctrl Pts',(-0.0311660487382375,0.0133854863143006,
-0.000598005060207441));
#52681=CARTESIAN_POINT('Ctrl Pts',(-0.031235681726719,0.0133876603108539,
-0.00028351370406858));
#52682=CARTESIAN_POINT('Ctrl Pts',(-0.0312563008708948,0.0133883040567185,
-0.000190389126828655));
#52683=CARTESIAN_POINT('Ctrl Pts',(-0.0312666928517517,0.0133886046897988,
-9.52395766237666E-5));
#52684=CARTESIAN_POINT('Ctrl Pts',(-0.031266718265333,0.0133885997848049,
-1.27307345280826E-7));
#52685=CARTESIAN_POINT('Ctrl Pts',(-0.0312668046408911,0.0133885831137349,
0.000323139817202629));
#52686=CARTESIAN_POINT('Ctrl Pts',(-0.0311434100165953,0.0133858216570961,
0.000646644017152718));
#52687=CARTESIAN_POINT('Ctrl Pts',(-0.0309186432993367,0.0133753622687773,
0.000890224316156055));
#52688=CARTESIAN_POINT('Ctrl Pts',(-0.0308539464933894,0.0133723516405818,
0.000960336419626767));
#52689=CARTESIAN_POINT('Ctrl Pts',(-0.0307811557550656,0.0133686447732898,
0.00102384151068166));
#52690=CARTESIAN_POINT('Ctrl Pts',(-0.0307016309076775,0.0133640088280151,
0.00107891472440616));
#52691=CARTESIAN_POINT('Origin',(-0.0350471488028758,0.025630288756216,
-0.00853808901214505));
#52692=CARTESIAN_POINT('Ctrl Pts',(-0.0347727610542622,0.012000956525018,
-0.00227981334747211));
#52693=CARTESIAN_POINT('Ctrl Pts',(-0.0326642925703876,0.01239375001385,
-0.00151682761576582));
#52694=CARTESIAN_POINT('Ctrl Pts',(-0.03066311424583,0.0133825300884908,
-0.00106998024085706));
#52695=CARTESIAN_POINT('Ctrl Pts',(-0.0345175998045572,0.0119430361337218,
-0.00241714021238289));
#52696=CARTESIAN_POINT('Ctrl Pts',(-0.0323553515124146,0.0123566043453443,
-0.00167688730984057));
#52697=CARTESIAN_POINT('Ctrl Pts',(-0.0303095288998628,0.0133818938394319,
-0.00127859035195531));
#52698=CARTESIAN_POINT('Ctrl Pts',(-0.0341371660549221,0.0118489399475177,
-0.00262427032416602));
#52699=CARTESIAN_POINT('Ctrl Pts',(-0.0318999712760361,0.0122981422085741,
-0.00191169889138664));
#52700=CARTESIAN_POINT('Ctrl Pts',(-0.029794006492062,0.0133808935020843,
-0.0015827147044274));
#52701=CARTESIAN_POINT('Ctrl Pts',(-0.03359953982734,0.0117040686094275,
-0.0029149026918325));
#52702=CARTESIAN_POINT('Ctrl Pts',(-0.0312857444835857,0.0122156780731898,
-0.0022266513258499));
#52703=CARTESIAN_POINT('Ctrl Pts',(-0.0291240247977924,0.0133794825587464,
-0.00197790333209557));
#52704=CARTESIAN_POINT('Ctrl Pts',(-0.0331700961547601,0.0115849838518695,
-0.00314276868365366));
#52705=CARTESIAN_POINT('Ctrl Pts',(-0.0308143431151271,0.012152185224641,
-0.00246736253434012));
#52706=CARTESIAN_POINT('Ctrl Pts',(-0.0286267867573773,0.0133783959197543,
-0.00227116412235461));
#52707=CARTESIAN_POINT('Ctrl Pts',(-0.0327013830619387,0.0114548347231496,
-0.0033840386214771));
#52708=CARTESIAN_POINT('Ctrl Pts',(-0.0303243200167066,0.0120877808095269,
-0.00271670426744098));
#52709=CARTESIAN_POINT('Ctrl Pts',(-0.0281311992831569,0.0133772919708067,
-0.002563413094503));
#52710=CARTESIAN_POINT('Ctrl Pts',(-0.0322633022287014,0.0113362370202907,
-0.00360133811397268));
#52711=CARTESIAN_POINT('Ctrl Pts',(-0.0298917430076046,0.0120338445178328,
-0.00293676226773174));
#52712=CARTESIAN_POINT('Ctrl Pts',(-0.0277161181765403,0.0133763644965302,
-0.00280816048294128));
#52713=CARTESIAN_POINT('Ctrl Pts',(-0.0318718490579452,0.0112346016841242,
-0.00379002559821603));
#52714=CARTESIAN_POINT('Ctrl Pts',(-0.0295242954891501,0.0119908397586535,
-0.00312456116268488));
#52715=CARTESIAN_POINT('Ctrl Pts',(-0.0273809764418348,0.013375621969192,
-0.00300576632589705));
#52716=CARTESIAN_POINT('Ctrl Pts',(-0.0315526756063215,0.0111545881961619,
-0.00394133469003171));
#52717=CARTESIAN_POINT('Ctrl Pts',(-0.0292351036521467,0.0119586531268908,
-0.00327316193381772));
#52718=CARTESIAN_POINT('Ctrl Pts',(-0.0271270696533341,0.0133750642031843,
-0.00315547587947468));
#52719=CARTESIAN_POINT('Ctrl Pts',(-0.0312014210942059,0.0110702650311837,
-0.00410563573794732));
#52720=CARTESIAN_POINT('Ctrl Pts',(-0.0289286457521131,0.0119264976660814,
-0.00343191460904337));
#52721=CARTESIAN_POINT('Ctrl Pts',(-0.0268695127905437,0.0133745044065779,
-0.00330734508306625));
#52722=CARTESIAN_POINT('Ctrl Pts',(-0.030874392335899,0.0109957669425451,
-0.00425734882219583));
#52723=CARTESIAN_POINT('Ctrl Pts',(-0.0286546244642002,0.0118996312458295,
-0.00357549439591694));
#52724=CARTESIAN_POINT('Ctrl Pts',(-0.0266506540595016,0.0133740340157121,
-0.00343640952528322));
#52725=CARTESIAN_POINT('Ctrl Pts',(-0.0305849371878325,0.0109329649976957,
-0.00439163244392445));
#52726=CARTESIAN_POINT('Ctrl Pts',(-0.0284201388623915,0.0118779356122285,
-0.00369985556253239));
#52727=CARTESIAN_POINT('Ctrl Pts',(-0.0264718895472516,0.0133736521617784,
-0.00354184514292115));
#52728=CARTESIAN_POINT('Ctrl Pts',(-0.0303517903493002,0.0108841186312876,
-0.00450011332417866));
#52729=CARTESIAN_POINT('Ctrl Pts',(-0.0282355790180237,0.0118615266852309,
-0.00379864860220248));
#52730=CARTESIAN_POINT('Ctrl Pts',(-0.0263358824933711,0.0133733622256437,
-0.00362207257248992));
#52731=CARTESIAN_POINT('Ctrl Pts',(-0.0300997675905012,0.0108332970063754,
-0.00461811904366943));
#52732=CARTESIAN_POINT('Ctrl Pts',(-0.0280408014590061,0.0118449004444461,
-0.00390403183868317));
#52733=CARTESIAN_POINT('Ctrl Pts',(-0.0261976785729545,0.0133730672528979,
-0.003703609311004));
#52734=CARTESIAN_POINT('Ctrl Pts',(-0.0298247967320212,0.0107801243754552,
-0.00474823453246165));
#52735=CARTESIAN_POINT('Ctrl Pts',(-0.0278335547303766,0.0118279104841727,
-0.00401756090056744));
#52736=CARTESIAN_POINT('Ctrl Pts',(-0.0260567792745189,0.0133727645665508,
-0.0037867540289952));
#52737=CARTESIAN_POINT('Ctrl Pts',(-0.0295719930617066,0.0107334368600793,
-0.00486975437016942));
#52738=CARTESIAN_POINT('Ctrl Pts',(-0.0276479485836656,0.0118132632712226,
-0.00412070886673605));
#52739=CARTESIAN_POINT('Ctrl Pts',(-0.0259366131982632,0.0133725025804461,
-0.00385768385443678));
#52740=CARTESIAN_POINT('Ctrl Pts',(-0.0293515712931725,0.0106942893521317,
-0.00497757727446442));
#52741=CARTESIAN_POINT('Ctrl Pts',(-0.0274895265439536,0.0118010629011895,
-0.00420990088068877));
#52742=CARTESIAN_POINT('Ctrl Pts',(-0.0258384047699654,0.01337228380016,
-0.00391566918926073));
#52743=CARTESIAN_POINT('Ctrl Pts',(-0.0291391659279289,0.0106575655708569,
-0.0050828951244524));
#52744=CARTESIAN_POINT('Ctrl Pts',(-0.0273390541578014,0.0117896259521601,
-0.00429540644467852));
#52745=CARTESIAN_POINT('Ctrl Pts',(-0.0257479800864673,0.0133720783997972,
-0.00396907047371278));
#52746=CARTESIAN_POINT('Ctrl Pts',(-0.0289674849020721,0.0106289606342586,
-0.00516976597180735));
#52747=CARTESIAN_POINT('Ctrl Pts',(-0.02721969022651,0.0117806707763832,
-0.0043641191545271));
#52748=CARTESIAN_POINT('Ctrl Pts',(-0.0256793615951877,0.0133719173903702,
-0.00400960740700386));
#52749=CARTESIAN_POINT('Ctrl Pts',(-0.0289147502730564,0.0106122180693434,
-0.00520803367000348));
#52750=CARTESIAN_POINT('Ctrl Pts',(-0.0271378379892791,0.0117745370161908,
-0.00441172434704335));
#52751=CARTESIAN_POINT('Ctrl Pts',(-0.025633907607635,0.0133718071218718,
-0.00403646747319105));
#52752=CARTESIAN_POINT('Ctrl Pts',(-0.0288614479214877,0.0105959306253864,
-0.00524578660432017));
#52753=CARTESIAN_POINT('Ctrl Pts',(-0.0271290244595121,0.0117738703384706,
-0.00441686056377363));
#52754=CARTESIAN_POINT('Ctrl Pts',(-0.0256290366711919,0.0133717951397229,
-0.00403934602138506));
#52755=CARTESIAN_POINT('Ctrl Pts',(-0.0288073858068765,0.0105787676699155,
-0.00528498245870882));
#52756=CARTESIAN_POINT('Ctrl Pts',(-0.0271217175885171,0.0117733370610431,
-0.00442110236585357));
#52757=CARTESIAN_POINT('Ctrl Pts',(-0.0256248590438472,0.0133717159890139,
-0.00404186864921482));
#52758=CARTESIAN_POINT('Ctrl Pts',(-0.028753248636285,0.0105614142183789,
-0.00532451795721782));
#52759=CARTESIAN_POINT('Ctrl Pts',(-0.0271187092444645,0.0117744642076714,
-0.00442049835616301));
#52760=CARTESIAN_POINT('Ctrl Pts',(-0.0256213618193222,0.0133716002169367,
-0.00404401940088713));
#52761=CARTESIAN_POINT('Ctrl Pts',(-0.0286972824510733,0.0105432493465016,
-0.00536565854362216));
#52762=CARTESIAN_POINT('Ctrl Pts',(-0.0271115673024987,0.0117729678320726,
-0.00442531770637433));
#52763=CARTESIAN_POINT('Ctrl Pts',(-0.0256190493030287,0.0133714876905249,
-0.00404547015830714));
#52764=CARTESIAN_POINT('Ctrl Pts',(-0.0286411031923645,0.010524877141472,
-0.00540711703952029));
#52765=CARTESIAN_POINT('Ctrl Pts',(-0.0270915719571781,0.0117662732028744,
-0.00444208328235592));
#52766=CARTESIAN_POINT('Ctrl Pts',(-0.0256171019831343,0.01337135765012,
-0.00404671993903247));
#52767=CARTESIAN_POINT('Ctrl Pts',(-0.0285828830651116,0.0105057502210374,
-0.00544990797483098));
#52768=CARTESIAN_POINT('Ctrl Pts',(-0.0270727421042012,0.0117594675002445,
-0.00445920463210022));
#52769=CARTESIAN_POINT('Ctrl Pts',(-0.0256155327883204,0.0133712308031466,
-0.00404774448896239));
#52770=CARTESIAN_POINT('Ctrl Pts',(-0.0285246450454284,0.0104864150634632,
-0.00549316804071699));
#52771=CARTESIAN_POINT('Ctrl Pts',(-0.0270423634194359,0.0117483911363854,
-0.00448636607666542));
#52772=CARTESIAN_POINT('Ctrl Pts',(-0.0256138793235271,0.0133710771466519,
-0.00404883993594807));
#52773=CARTESIAN_POINT('Ctrl Pts',(-0.028465753619234,0.0104665820148817,
-0.00553745416170548));
#52774=CARTESIAN_POINT('Ctrl Pts',(-0.0269825259250966,0.0117268108665561,
-0.00453842518565841));
#52775=CARTESIAN_POINT('Ctrl Pts',(-0.0256114990915839,0.0133708330482361,
-0.00405043536832266));
#52776=CARTESIAN_POINT('Ctrl Pts',(-0.0284067653367236,0.0104463348507675,
-0.00558277907219412));
#52777=CARTESIAN_POINT('Ctrl Pts',(-0.0269035426341023,0.011698536842693,
-0.00460702967746145));
#52778=CARTESIAN_POINT('Ctrl Pts',(-0.025608425009902,0.0133704800254569,
-0.00405252594601399));
#52779=CARTESIAN_POINT('Ctrl Pts',(-0.0280675604554757,0.0103218692995789,
-0.00587331047521013));
#52780=CARTESIAN_POINT('Ctrl Pts',(-0.0267271007860639,0.0116361165146999,
-0.00475980726027247));
#52781=CARTESIAN_POINT('Ctrl Pts',(-0.0256002489243723,0.0133693958273193,
-0.00405820166310776));
#52782=CARTESIAN_POINT('Ctrl Pts',(-0.0277460264250124,0.0102161009525818,
-0.0061634089554616));
#52783=CARTESIAN_POINT('Ctrl Pts',(-0.0265551296789588,0.011577260405049,
-0.00490730587419467));
#52784=CARTESIAN_POINT('Ctrl Pts',(-0.0255890676586056,0.0133683816772428,
-0.00406559971933516));
#52785=CARTESIAN_POINT('Ctrl Pts',(-0.0274863162998273,0.0101367292540289,
-0.00640461551926327));
#52786=CARTESIAN_POINT('Ctrl Pts',(-0.0264124795131404,0.011529920823339,
-0.0050286097627996));
#52787=CARTESIAN_POINT('Ctrl Pts',(-0.0255757644815469,0.0133675703687158,
-0.00407409533213147));
#52788=CARTESIAN_POINT('Ctrl Pts',(-0.0272914928284565,0.0100812016712519,
-0.00658978567130121));
#52789=CARTESIAN_POINT('Ctrl Pts',(-0.0263030488949675,0.0114946427485996,
-0.00512099352964556));
#52790=CARTESIAN_POINT('Ctrl Pts',(-0.0255630018470322,0.013366968727325,
-0.0040821099818228));
#52791=CARTESIAN_POINT('Ctrl Pts',(-0.0270840414635881,0.0100254412579728,
-0.00679019156849944));
#52792=CARTESIAN_POINT('Ctrl Pts',(-0.0261841898257576,0.0114573548804285,
-0.00522070556443383));
#52793=CARTESIAN_POINT('Ctrl Pts',(-0.0255464591387835,0.0133663353614209,
-0.00409238655333308));
#52794=CARTESIAN_POINT('Ctrl Pts',(-0.0268835994452472,0.00997607256763211,
-0.00698779961283796));
#52795=CARTESIAN_POINT('Ctrl Pts',(-0.0260661813151271,0.0114218163578175,
-0.00531885137188345));
#52796=CARTESIAN_POINT('Ctrl Pts',(-0.0255263021183457,0.0133657349749526,
-0.00410477867652445));
#52797=CARTESIAN_POINT('Ctrl Pts',(-0.0266908179464102,0.00993278896673545,
-0.00718096844533468));
#52798=CARTESIAN_POINT('Ctrl Pts',(-0.0259495729075507,0.0113882771479691,
-0.0054150113612664));
#52799=CARTESIAN_POINT('Ctrl Pts',(-0.0255025273298817,0.0133651713259671,
-0.00411928732511149));
#52800=CARTESIAN_POINT('Ctrl Pts',(-0.0265287433143654,0.00989956116966734,
-0.00734541975738988));
#52801=CARTESIAN_POINT('Ctrl Pts',(-0.0258491621773471,0.0113606579109212,
-0.0054972041668335));
#52802=CARTESIAN_POINT('Ctrl Pts',(-0.0254790717439256,0.0133647093906794,
-0.00413353208185679));
#52803=CARTESIAN_POINT('Ctrl Pts',(-0.0263423809876361,0.00986455026007133,
-0.00753629868729644));
#52804=CARTESIAN_POINT('Ctrl Pts',(-0.0257312574486088,0.0113295756134489,
-0.00559310886750162));
#52805=CARTESIAN_POINT('Ctrl Pts',(-0.0254484295753836,0.0133641918274074,
-0.00415207922632118));
#52806=CARTESIAN_POINT('Ctrl Pts',(-0.0261481867185806,0.00983278279304436,
-0.00773746330827286));
#52807=CARTESIAN_POINT('Ctrl Pts',(-0.0256048170539434,0.0112983188867912,
-0.00569507952915905));
#52808=CARTESIAN_POINT('Ctrl Pts',(-0.0254109127952933,0.0133636745317756,
-0.00417470466049298));
#52809=CARTESIAN_POINT('Ctrl Pts',(-0.0259520714360624,0.00980574636897381,
-0.00794239949141725));
#52810=CARTESIAN_POINT('Ctrl Pts',(-0.0254733159889546,0.0112681849843151,
-0.00580023449269352));
#52811=CARTESIAN_POINT('Ctrl Pts',(-0.0253667807403883,0.0133631791111596,
-0.00420124155186773));
#52812=CARTESIAN_POINT('Ctrl Pts',(-0.025724264374708,0.00977962414268888,
-0.00818184634833232));
#52813=CARTESIAN_POINT('Ctrl Pts',(-0.0253165660483512,0.0112348349148003,
-0.00592469000507303));
#52814=CARTESIAN_POINT('Ctrl Pts',(-0.0253088183986679,0.0133626344216237,
-0.00423602339438577));
#52815=CARTESIAN_POINT('Ctrl Pts',(-0.0254843721584209,0.00975992424360273,
-0.00843536695618243));
#52816=CARTESIAN_POINT('Ctrl Pts',(-0.0251457422557053,0.0112024178504661,
-0.00605907812247795));
#52817=CARTESIAN_POINT('Ctrl Pts',(-0.0252376676352329,0.0133621100169332,
-0.00427862501603976));
#52818=CARTESIAN_POINT('Ctrl Pts',(-0.0252392523779962,0.00974825625449607,
-0.00869475393969651));
#52819=CARTESIAN_POINT('Ctrl Pts',(-0.0249651509091306,0.0111726248652654,
-0.00619993688839688));
#52820=CARTESIAN_POINT('Ctrl Pts',(-0.0251537017368419,0.0133616335190601,
-0.00432881130383831));
#52821=CARTESIAN_POINT('Ctrl Pts',(-0.0250252274687213,0.00974459884238429,
-0.00892086419570641));
#52822=CARTESIAN_POINT('Ctrl Pts',(-0.0248029092461888,0.0111494016223978,
-0.0063256338420981));
#52823=CARTESIAN_POINT('Ctrl Pts',(-0.0250715464480529,0.0133612665548016,
-0.00437785630142376));
#52824=CARTESIAN_POINT('Ctrl Pts',(-0.0248330956640217,0.00974647630868264,
-0.00912309242891329));
#52825=CARTESIAN_POINT('Ctrl Pts',(-0.0246537608279187,0.0111309194011829,
-0.00644057507543671));
#52826=CARTESIAN_POINT('Ctrl Pts',(-0.0249907066455409,0.0133609782590991,
-0.00442607439890494));
#52827=CARTESIAN_POINT('Ctrl Pts',(-0.0245992392867989,0.00975445323702422,
-0.00936798685351651));
#52828=CARTESIAN_POINT('Ctrl Pts',(-0.0244684134772241,0.0111111737434523,
-0.00658279010480466));
#52829=CARTESIAN_POINT('Ctrl Pts',(-0.0248844024824674,0.0133606748224033,
-0.00448943937177968));
#52830=CARTESIAN_POINT('Ctrl Pts',(-0.0243393500301934,0.00977216831379076,
-0.0096375484899141));
#52831=CARTESIAN_POINT('Ctrl Pts',(-0.0242567634085124,0.0110937425586607,
-0.00674428919556468));
#52832=CARTESIAN_POINT('Ctrl Pts',(-0.0247538271850526,0.013360414619455,
-0.00456721181626968));
#52833=CARTESIAN_POINT('Ctrl Pts',(-0.0240619644435389,0.00980124135293209,
-0.00992099818357101));
#52834=CARTESIAN_POINT('Ctrl Pts',(-0.0240246691820906,0.0110807496794517,
-0.00692046297213162));
#52835=CARTESIAN_POINT('Ctrl Pts',(-0.02459988346086,0.0133602315273817,
-0.00465884060783006));
#52836=CARTESIAN_POINT('Ctrl Pts',(-0.0237256093236952,0.00984721700118359,
-0.0102590817514845));
#52837=CARTESIAN_POINT('Ctrl Pts',(-0.0237368086416349,0.0110712816730396,
-0.00713804617400964));
#52838=CARTESIAN_POINT('Ctrl Pts',(-0.0243975472063884,0.0133601146533764,
-0.00477921310507474));
#52839=CARTESIAN_POINT('Ctrl Pts',(-0.0232026024969606,0.00994122487110758,
-0.0107704884933705));
#52840=CARTESIAN_POINT('Ctrl Pts',(-0.0232762649733642,0.011070587387176,
-0.00748425252227681));
#52841=CARTESIAN_POINT('Ctrl Pts',(-0.0240493425813566,0.0133601652903972,
-0.00498624593995807));
#52842=CARTESIAN_POINT('Ctrl Pts',(-0.0225740146247116,0.0100955861323387,
-0.0113494892384633));
#52843=CARTESIAN_POINT('Ctrl Pts',(-0.0227010714720119,0.0110984998660559,
-0.00791268507570289));
#52844=CARTESIAN_POINT('Ctrl Pts',(-0.0235661364076886,0.0133606964400032,
-0.00527333232331995));
#52845=CARTESIAN_POINT('Ctrl Pts',(-0.0219161527424833,0.0102913170500384,
-0.0119097490487537));
#52846=CARTESIAN_POINT('Ctrl Pts',(-0.0220819411571392,0.0111564260647825,
-0.0083679967886967));
#52847=CARTESIAN_POINT('Ctrl Pts',(-0.0230005865620769,0.0133617162333888,
-0.00560913016806318));
#52848=CARTESIAN_POINT('Ctrl Pts',(-0.0213172350541001,0.0104904030844707,
-0.0123799586077945));
#52849=CARTESIAN_POINT('Ctrl Pts',(-0.0215073227281529,0.0112302659879934,
-0.00878379991450101));
#52850=CARTESIAN_POINT('Ctrl Pts',(-0.0224436992424846,0.0133629840096402,
-0.00593960650541536));
#52851=CARTESIAN_POINT('Ctrl Pts',(-0.0209433957024175,0.010622740123274,
-0.0126501240251599));
#52852=CARTESIAN_POINT('Ctrl Pts',(-0.0211438108508993,0.0112868011786277,
-0.00904170165224759));
#52853=CARTESIAN_POINT('Ctrl Pts',(-0.0220761122516573,0.0133639433085236,
-0.006157634856723));
#52854=CARTESIAN_POINT('Ctrl Pts',(-0.0207607720679562,0.0106884755658043,
-0.0127768900671979));
#52855=CARTESIAN_POINT('Ctrl Pts',(-0.0209653293817326,0.0113164079967516,
-0.00916689820331034));
#52856=CARTESIAN_POINT('Ctrl Pts',(-0.0218928511860286,0.0133644439833726,
-0.00626630585176376));
#52857=CARTESIAN_POINT('',(-0.0275862774756162,0.0133330202728796,-0.00292880065737905));
#52858=CARTESIAN_POINT('Ctrl Pts',(-0.0275862774763506,0.013333020272888,
-0.00292880065694408));
#52859=CARTESIAN_POINT('Ctrl Pts',(-0.0276231848556899,0.0133334417442254,
-0.00290694105669624));
#52860=CARTESIAN_POINT('Ctrl Pts',(-0.0276608954101289,0.0133338715013257,
-0.00288460358966488));
#52861=CARTESIAN_POINT('Ctrl Pts',(-0.0276994051609495,0.0133343091774083,
-0.00286179020680056));
#52862=CARTESIAN_POINT('Ctrl Pts',(-0.0278520896348891,0.0133360444870636,
-0.0027713391057887));
#52863=CARTESIAN_POINT('Ctrl Pts',(-0.0280172941783116,0.013337904690857,
-0.00267343260130032));
#52864=CARTESIAN_POINT('Ctrl Pts',(-0.0281945943953082,0.0133398597451922,
-0.00256829614352595));
#52865=CARTESIAN_POINT('Ctrl Pts',(-0.0283492772393959,0.0133415654022411,
-0.00247657145992808));
#52866=CARTESIAN_POINT('Ctrl Pts',(-0.0285131649912883,0.0133433431611263,
-0.00237934434940374));
#52867=CARTESIAN_POINT('Ctrl Pts',(-0.0286864908250938,0.0133451700007234,
-0.00227646351282891));
#52868=CARTESIAN_POINT('Ctrl Pts',(-0.0287602956774135,0.0133459478976111,
-0.00223265524268692));
#52869=CARTESIAN_POINT('Ctrl Pts',(-0.0288358183015014,0.0133467346635766,
-0.00218781802139747));
#52870=CARTESIAN_POINT('Ctrl Pts',(-0.028913095790404,0.0133475282712897,
-0.00214192925684343));
#52871=CARTESIAN_POINT('Ctrl Pts',(-0.028999694532617,0.0133484176044027,
-0.00209050536421288));
#52872=CARTESIAN_POINT('Ctrl Pts',(-0.0290884724255105,0.0133493164175403,
-0.00203777409793986));
#52873=CARTESIAN_POINT('Ctrl Pts',(-0.0291793916664724,0.0133502203639561,
-0.00198375759913417));
#52874=CARTESIAN_POINT('Ctrl Pts',(-0.0293387692148659,0.0133518049434368,
-0.0018890689824962));
#52875=CARTESIAN_POINT('Ctrl Pts',(-0.0295047162972014,0.0133534051942572,
-0.00179043711833477));
#52876=CARTESIAN_POINT('Ctrl Pts',(-0.0296771691003025,0.0133549989591328,
-0.00168790140755359));
#52877=CARTESIAN_POINT('Ctrl Pts',(-0.0299962080745732,0.013357947436061,
-0.00149820957648156));
#52878=CARTESIAN_POINT('Ctrl Pts',(-0.0303374541903357,0.0133608714375898,
-0.00129519073320025));
#52879=CARTESIAN_POINT('Ctrl Pts',(-0.0307014085265843,0.0133636696479055,
-0.00107855839000479));
#52880=CARTESIAN_POINT('',(-0.0235554094661677,0.0133260932704124,-0.0053124061551198));
#52881=CARTESIAN_POINT('Ctrl Pts',(-0.0235554094661677,0.0133260932704124,
-0.0053124061551198));
#52882=CARTESIAN_POINT('Ctrl Pts',(-0.0235658492861846,0.0133260054407238,
-0.00530623551542229));
#52883=CARTESIAN_POINT('Ctrl Pts',(-0.0235762971536648,0.0133259176534734,
-0.00530005997256611));
#52884=CARTESIAN_POINT('Ctrl Pts',(-0.0235867539693412,0.0133258299168732,
-0.00529387898775706));
#52885=CARTESIAN_POINT('Ctrl Pts',(-0.0236783788545834,0.0133250611497673,
-0.0052397198592672));
#52886=CARTESIAN_POINT('Ctrl Pts',(-0.0237706788717137,0.0133242956193828,
-0.00518515084923147));
#52887=CARTESIAN_POINT('Ctrl Pts',(-0.0238578591296201,0.0133235786917102,
-0.00513360507976362));
#52888=CARTESIAN_POINT('Ctrl Pts',(-0.0239450393875266,0.0133228617640375,
-0.00508205931029576));
#52889=CARTESIAN_POINT('Ctrl Pts',(-0.024027099956465,0.0133221920484148,
-0.00503353693195624));
#52890=CARTESIAN_POINT('Ctrl Pts',(-0.0241277543322011,0.0133213953644077,
-0.00497400492496752));
#52891=CARTESIAN_POINT('Ctrl Pts',(-0.0241309185695083,0.0133213703193241,
-0.00497213343755219));
#52892=CARTESIAN_POINT('Ctrl Pts',(-0.0241341009493045,0.0133213451392199,
-0.00497025121882874));
#52893=CARTESIAN_POINT('Ctrl Pts',(-0.0241373005541634,0.0133213198334391,
-0.00496835880990149));
#52894=CARTESIAN_POINT('Ctrl Pts',(-0.0242302889664409,0.0133205843850071,
-0.00491336073692433));
#52895=CARTESIAN_POINT('Ctrl Pts',(-0.0243379925743662,0.0133197521448476,
-0.00484964914926691));
#52896=CARTESIAN_POINT('Ctrl Pts',(-0.0244369717904454,0.013319023633445,
-0.00479108410181297));
#52897=CARTESIAN_POINT('Ctrl Pts',(-0.0244429234182031,0.0133189798279992,
-0.00478756258107495));
#52898=CARTESIAN_POINT('Ctrl Pts',(-0.0244488428242526,0.0133189363515234,
-0.00478406010566338));
#52899=CARTESIAN_POINT('Ctrl Pts',(-0.0244547247477199,0.0133188932322421,
-0.00478057979824662));
#52900=CARTESIAN_POINT('Ctrl Pts',(-0.0245018576318574,0.0133185477098804,
-0.00475269148464483));
#52901=CARTESIAN_POINT('Ctrl Pts',(-0.0245466349835242,0.0133182287644832,
-0.00472619285369439));
#52902=CARTESIAN_POINT('Ctrl Pts',(-0.0245896441130481,0.0133179292759041,
-0.00470073895623896));
#52903=CARTESIAN_POINT('Ctrl Pts',(-0.0246437743023649,0.0133175523472457,
-0.00466870333256173));
#52904=CARTESIAN_POINT('Ctrl Pts',(-0.0246951009569881,0.013317206128952,
-0.00463832423661032));
#52905=CARTESIAN_POINT('Ctrl Pts',(-0.0247448283738734,0.0133168815166838,
-0.00460889008847095));
#52906=CARTESIAN_POINT('Ctrl Pts',(-0.0247993497452306,0.0133165256102819,
-0.00457661835143318));
#52907=CARTESIAN_POINT('Ctrl Pts',(-0.0248519631573275,0.0133161963315964,
-0.00454547346378711));
#52908=CARTESIAN_POINT('Ctrl Pts',(-0.0249032755518165,0.0133158882105585,
-0.00451509898440173));
#52909=CARTESIAN_POINT('Ctrl Pts',(-0.0249305427162006,0.0133157244764924,
-0.00449895812933675));
#52910=CARTESIAN_POINT('Ctrl Pts',(-0.0249574422684759,0.013315566681462,
-0.00448303496590283));
#52911=CARTESIAN_POINT('Ctrl Pts',(-0.0249840788117782,0.0133154157723874,
-0.00446726666635377));
#52912=CARTESIAN_POINT('Ctrl Pts',(-0.0249903076308074,0.0133153804830743,
-0.00446357933038167));
#52913=CARTESIAN_POINT('Ctrl Pts',(-0.0249965220598463,0.013315345569571,
-0.00445990046775898));
#52914=CARTESIAN_POINT('Ctrl Pts',(-0.0250027234833143,0.0133153110639603,
-0.00445622923316655));
#52915=CARTESIAN_POINT('Ctrl Pts',(-0.0250243757433542,0.0133151905876761,
-0.00444341112350606));
#52916=CARTESIAN_POINT('Ctrl Pts',(-0.02504585547353,0.0133150731717387,
-0.00443069599930903));
#52917=CARTESIAN_POINT('Ctrl Pts',(-0.0250662261098503,0.0133149652173997,
-0.0044186370787462));
#52918=CARTESIAN_POINT('Ctrl Pts',(-0.0250845012624421,0.0133148683680924,
-0.00440781863351386));
#52919=CARTESIAN_POINT('Ctrl Pts',(-0.0251018839688812,0.0133147791485272,
-0.00439752819845495));
#52920=CARTESIAN_POINT('Ctrl Pts',(-0.0251176667062615,0.0133146978585057,
-0.00438818677023798));
#52921=CARTESIAN_POINT('Ctrl Pts',(-0.0251289081109167,0.0133146399589155,
-0.00438153324923498));
#52922=CARTESIAN_POINT('Ctrl Pts',(-0.0251393672296564,0.0133145908840516,
-0.00437533966333391));
#52923=CARTESIAN_POINT('Ctrl Pts',(-0.0251500524476353,0.0133145402199908,
-0.00436901342239919));
#52924=CARTESIAN_POINT('Ctrl Pts',(-0.0251710911098042,0.0133144404649778,
-0.00435655736899099));
#52925=CARTESIAN_POINT('Ctrl Pts',(-0.025192958670792,0.0133143251891466,
-0.00434362187228724));
#52926=CARTESIAN_POINT('Ctrl Pts',(-0.0252237910271604,0.013314192950973,
-0.00432536835455965));
#52927=CARTESIAN_POINT('Ctrl Pts',(-0.0252277231277903,0.0133141760864233,
-0.00432304045371105));
#52928=CARTESIAN_POINT('Ctrl Pts',(-0.0252317980417083,0.0133141584760881,
-0.00432062824806579));
#52929=CARTESIAN_POINT('Ctrl Pts',(-0.0252359977075615,0.0133141402882188,
-0.00431814238915245));
#52930=CARTESIAN_POINT('Ctrl Pts',(-0.0252620229300343,0.0133140275784557,
-0.00430273758469499));
#52931=CARTESIAN_POINT('Ctrl Pts',(-0.0252928600872312,0.013313896033216,
-0.00428448956400194));
#52932=CARTESIAN_POINT('Ctrl Pts',(-0.0253242399560579,0.0133137859078515,
-0.00426591395739906));
#52933=CARTESIAN_POINT('Ctrl Pts',(-0.025339382382456,0.0133137327666088,
-0.0042569502565838));
#52934=CARTESIAN_POINT('Ctrl Pts',(-0.025354647350045,0.0133136840671119,
-0.00424791290030452));
#52935=CARTESIAN_POINT('Ctrl Pts',(-0.0253695236850595,0.0133136397773049,
-0.00423910620272196));
#52936=CARTESIAN_POINT('Ctrl Pts',(-0.0253776637620361,0.0133136155426774,
-0.00423428732790086));
#52937=CARTESIAN_POINT('Ctrl Pts',(-0.025385686741189,0.0133135924781677,
-0.00422953805765722));
#52938=CARTESIAN_POINT('Ctrl Pts',(-0.025393504626859,0.0133135696988639,
-0.0042249113754429));
#52939=CARTESIAN_POINT('Ctrl Pts',(-0.0254011519272082,0.0133135474166018,
-0.00422038564687547));
#52940=CARTESIAN_POINT('Ctrl Pts',(-0.0254086164986546,0.0133135303432495,
-0.00421596522967111));
#52941=CARTESIAN_POINT('Ctrl Pts',(-0.0254159159734615,0.0133135158404069,
-0.00421164170555362));
#52942=CARTESIAN_POINT('Ctrl Pts',(-0.0254326936382193,0.013313482505977,
-0.00420170419085085));
#52943=CARTESIAN_POINT('Ctrl Pts',(-0.0254486018479688,0.01331346370787,
-0.00419227621541077));
#52944=CARTESIAN_POINT('Ctrl Pts',(-0.0254638936319852,0.013313440647475,
-0.00418322235340209));
#52945=CARTESIAN_POINT('Ctrl Pts',(-0.0254723457635774,0.013313427901448,
-0.0041782180692039));
#52946=CARTESIAN_POINT('Ctrl Pts',(-0.02548060973331,0.0133134137623807,
-0.00417332804958735));
#52947=CARTESIAN_POINT('Ctrl Pts',(-0.0254887509034164,0.0133133986807665,
-0.0041685132251211));
#52948=CARTESIAN_POINT('Ctrl Pts',(-0.0254974507188984,0.013313382564255,
-0.00416336800841554));
#52949=CARTESIAN_POINT('Ctrl Pts',(-0.0255060083594711,0.0133133653499205,
-0.00415830983005533));
#52950=CARTESIAN_POINT('Ctrl Pts',(-0.0255144520821152,0.0133133487170901,
-0.00415332075634523));
#52951=CARTESIAN_POINT('Ctrl Pts',(-0.0255234397510192,0.0133133310127694,
-0.0041480102855334));
#52952=CARTESIAN_POINT('Ctrl Pts',(-0.0255322998610173,0.0133133140782046,
-0.00414277712651648));
#52953=CARTESIAN_POINT('Ctrl Pts',(-0.025541138662,0.0133133103101731,-0.00413754883754291));
#52954=CARTESIAN_POINT('Ctrl Pts',(-0.0255508709169214,0.013313306161257,
-0.00413179205659573));
#52955=CARTESIAN_POINT('Ctrl Pts',(-0.0255602311446517,0.0133132097520181,
-0.00412633228609686));
#52956=CARTESIAN_POINT('Ctrl Pts',(-0.0255694251152151,0.0133131030788275,
-0.00412098283208935));
#52957=CARTESIAN_POINT('Ctrl Pts',(-0.0255745194584301,0.0133130439716289,
-0.00411801872049696));
#52958=CARTESIAN_POINT('Ctrl Pts',(-0.0255795642442733,0.0133129821416654,
-0.00411508725653711));
#52959=CARTESIAN_POINT('Ctrl Pts',(-0.0255846258569396,0.0133129422693187,
-0.00411212978689285));
#52960=CARTESIAN_POINT('Ctrl Pts',(-0.025590046090682,0.0133128995719705,
-0.00410896277712441));
#52961=CARTESIAN_POINT('Ctrl Pts',(-0.0255954859018437,0.0133128822816128,
-0.00410576560489704));
#52962=CARTESIAN_POINT('Ctrl Pts',(-0.0256010393897212,0.0133129290762867,
-0.00410245246194853));
#52963=CARTESIAN_POINT('Ctrl Pts',(-0.0256069643995486,0.0133129790014703,
-0.00409891767354846));
#52964=CARTESIAN_POINT('Ctrl Pts',(-0.0256130260218243,0.0133131040811672,
-0.00409524488678633));
#52965=CARTESIAN_POINT('Ctrl Pts',(-0.0256196460291501,0.0133134494561625,
-0.00409107144979685));
#52966=CARTESIAN_POINT('Ctrl Pts',(-0.0256266540147968,0.0133138150725268,
-0.00408665342046849));
#52967=CARTESIAN_POINT('Ctrl Pts',(-0.0256342855896086,0.0133144294524892,
-0.00408167416892234));
#52968=CARTESIAN_POINT('Ctrl Pts',(-0.0256432107295599,0.0133156374582877,
-0.00407547308559459));
#52969=CARTESIAN_POINT('Ctrl Pts',(-0.0256476607973974,0.0133162397690392,
-0.00407238123027074));
#52970=CARTESIAN_POINT('Ctrl Pts',(-0.0256524196456054,0.0133169857056992,
-0.00406899627038609));
#52971=CARTESIAN_POINT('Ctrl Pts',(-0.0256571163719194,0.0133177495159941,
-0.00406563648960932));
#52972=CARTESIAN_POINT('Ctrl Pts',(-0.0256599283179211,0.0133182068118128,
-0.0040636249774431));
#52973=CARTESIAN_POINT('Ctrl Pts',(-0.0256624304973125,0.0133185527829313,
-0.00406185835776172));
#52974=CARTESIAN_POINT('Ctrl Pts',(-0.0256652294818525,0.0133190313235768,
-0.00405982373038196));
#52975=CARTESIAN_POINT('Ctrl Pts',(-0.0256670051399155,0.0133193349067312,
-0.00405853297565989));
#52976=CARTESIAN_POINT('Ctrl Pts',(-0.02566733914117,0.0133190911623826,
-0.00405853938508495));
#52977=CARTESIAN_POINT('Ctrl Pts',(-0.0256680603283604,0.0133189950409093,
-0.00405819528840961));
#52978=CARTESIAN_POINT('Ctrl Pts',(-0.0256702238899314,0.0133187066764896,
-0.00405716299838359));
#52979=CARTESIAN_POINT('Ctrl Pts',(-0.0256722642526714,0.0133183852673014,
-0.0040562418071485));
#52980=CARTESIAN_POINT('Ctrl Pts',(-0.0256743451903822,0.0133180897561963,
-0.0040552722719998));
#52981=CARTESIAN_POINT('Ctrl Pts',(-0.0256782135456918,0.0133175404163739,
-0.0040534699564279));
#52982=CARTESIAN_POINT('Ctrl Pts',(-0.0256820420627053,0.0133170010333836,
-0.00405165031151659));
#52983=CARTESIAN_POINT('Ctrl Pts',(-0.0256861152907195,0.0133165612437565,
-0.00404961831687978));
#52984=CARTESIAN_POINT('Ctrl Pts',(-0.025691321013244,0.0133159991778079,
-0.0040470213593283));
#52985=CARTESIAN_POINT('Ctrl Pts',(-0.0256967831203199,0.0133155506355026,
-0.00404418358848677));
#52986=CARTESIAN_POINT('Ctrl Pts',(-0.0257025001964393,0.0133151975592595,
-0.00404112191995521));
#52987=CARTESIAN_POINT('Ctrl Pts',(-0.0257059262049844,0.0133149859751908,
-0.00403928718794668));
#52988=CARTESIAN_POINT('Ctrl Pts',(-0.0257094427183089,0.0133148082117484,
-0.00403737284876931));
#52989=CARTESIAN_POINT('Ctrl Pts',(-0.0257130482103409,0.0133146598176385,
-0.00403538330608558));
#52990=CARTESIAN_POINT('Ctrl Pts',(-0.025716418021914,0.0133145211236172,
-0.00403352381398255));
#52991=CARTESIAN_POINT('Ctrl Pts',(-0.0257198655625725,0.0133144080891559,
-0.00403159862363874));
#52992=CARTESIAN_POINT('Ctrl Pts',(-0.0257233896074754,0.0133143169834006,
-0.00402961139958997));
#52993=CARTESIAN_POINT('Ctrl Pts',(-0.0257298831949792,0.0133141491072214,
-0.00402594963772084));
#52994=CARTESIAN_POINT('Ctrl Pts',(-0.0257366366872511,0.0133140556780819,
-0.00402207716712653));
#52995=CARTESIAN_POINT('Ctrl Pts',(-0.0257436378676088,0.0133140135523751,
-0.0040180194655019));
#52996=CARTESIAN_POINT('Ctrl Pts',(-0.0257500497609761,0.0133139749723748,
-0.00401430329925501));
#52997=CARTESIAN_POINT('Ctrl Pts',(-0.0257566692258838,0.0133139794221993,
-0.00401043187403818));
#52998=CARTESIAN_POINT('Ctrl Pts',(-0.0257634903945885,0.0133140092147305,
-0.00400642269257857));
#52999=CARTESIAN_POINT('Ctrl Pts',(-0.0257698356340983,0.0133140369285657,
-0.00400269324126305));
#53000=CARTESIAN_POINT('Ctrl Pts',(-0.0257763480144088,0.0133140870620743,
-0.00399884850704672));
#53001=CARTESIAN_POINT('Ctrl Pts',(-0.0257831074779253,0.0133141345249859,
-0.00399486191656997));
#53002=CARTESIAN_POINT('Ctrl Pts',(-0.0257954433060206,0.0133142211434457,
-0.0039875865026726));
#53003=CARTESIAN_POINT('Ctrl Pts',(-0.0258085091621843,0.0133143164096352,
-0.00397987888238915));
#53004=CARTESIAN_POINT('Ctrl Pts',(-0.0258219986413289,0.0133144171496422,
-0.00397192062861168));
#53005=CARTESIAN_POINT('Ctrl Pts',(-0.0258467124879595,0.0133146017137055,
-0.00395734044644182));
#53006=CARTESIAN_POINT('Ctrl Pts',(-0.0258728398361485,0.013314804507215,
-0.00394192412456912));
#53007=CARTESIAN_POINT('Ctrl Pts',(-0.0258986042167096,0.0133150081123963,
-0.00392672277812987));
#53008=CARTESIAN_POINT('Ctrl Pts',(-0.0259239054514451,0.0133152080575288,
-0.00391179469423348));
#53009=CARTESIAN_POINT('Ctrl Pts',(-0.025948756672967,0.0133154073743607,
-0.00389713319324261));
#53010=CARTESIAN_POINT('Ctrl Pts',(-0.0259738210178452,0.0133156125864984,
-0.00388234554344445));
#53011=CARTESIAN_POINT('Ctrl Pts',(-0.0259941857584619,0.013315779321036,
-0.00387033060134514));
#53012=CARTESIAN_POINT('Ctrl Pts',(-0.0260146939666128,0.0133159499947089,
-0.00385823074062121));
#53013=CARTESIAN_POINT('Ctrl Pts',(-0.0260356880624994,0.0133161278974167,
-0.00384584354779159));
#53014=CARTESIAN_POINT('Ctrl Pts',(-0.0260635406891899,0.0133163639189026,
-0.00382940960086232));
#53015=CARTESIAN_POINT('Ctrl Pts',(-0.0260922691739588,0.0133166131470457,
-0.00381245761385976));
#53016=CARTESIAN_POINT('Ctrl Pts',(-0.0261207052556074,0.0133168642412803,
-0.00379567757791817));
#53017=CARTESIAN_POINT('Ctrl Pts',(-0.0261391717990104,0.0133170273032183,
-0.00378478053289456));
#53018=CARTESIAN_POINT('Ctrl Pts',(-0.0261575168897512,0.0133171911778366,
-0.00377395487041613));
#53019=CARTESIAN_POINT('Ctrl Pts',(-0.0261754345333995,0.0133173528891302,
-0.00376338113887659));
#53020=CARTESIAN_POINT('Ctrl Pts',(-0.0261981887788342,0.0133175582519858,
-0.00374995318555116));
#53021=CARTESIAN_POINT('Ctrl Pts',(-0.0262202456375072,0.0133177598241401,
-0.00373693616987632));
#53022=CARTESIAN_POINT('Ctrl Pts',(-0.0262472884083519,0.0133180118477269,
-0.00372097482579748));
#53023=CARTESIAN_POINT('Ctrl Pts',(-0.0262526205118232,0.0133180615399662,
-0.00371782768016444));
#53024=CARTESIAN_POINT('Ctrl Pts',(-0.0262581494700475,0.0133181132552533,
-0.00371456427142578));
#53025=CARTESIAN_POINT('Ctrl Pts',(-0.0262636619228426,0.0133181649442378,
-0.00371131058327889));
#53026=CARTESIAN_POINT('Ctrl Pts',(-0.0262861069165848,0.0133183754057108,
-0.003698062576845));
#53027=CARTESIAN_POINT('Ctrl Pts',(-0.0263082508432428,0.0133185851392778,
-0.00368499224816668));
#53028=CARTESIAN_POINT('Ctrl Pts',(-0.0263159809211684,0.0133186588979533,
-0.00368042925426218));
#53029=CARTESIAN_POINT('Ctrl Pts',(-0.0263256094932595,0.0133187507716358,
-0.00367474559671252));
#53030=CARTESIAN_POINT('Ctrl Pts',(-0.0263307395568127,0.0133188000401663,
-0.0036717172746909));
#53031=CARTESIAN_POINT('Ctrl Pts',(-0.0263319848737224,0.0133188134113866,
-0.00367098093719014));
#53032=CARTESIAN_POINT('Ctrl Pts',(-0.026333230190632,0.0133188267826069,
-0.00367024459968939));
#53033=CARTESIAN_POINT('Ctrl Pts',(-0.0263395456796712,0.013318889131422,
-0.00366651502588641));
#53034=CARTESIAN_POINT('Ctrl Pts',(-0.0263453162169995,0.0133189470465933,
-0.00366310656008888));
#53035=CARTESIAN_POINT('Ctrl Pts',(-0.0263568572916562,0.0133190628769359,
-0.00365628962849381));
#53036=CARTESIAN_POINT('Ctrl Pts',(-0.0263662185232684,0.0133191608357306,
-0.00365075706076423));
#53037=CARTESIAN_POINT('Ctrl Pts',(-0.0263774051172533,0.0133192790955712,
-0.00364414486510002));
#53038=CARTESIAN_POINT('Ctrl Pts',(-0.0263852136259227,0.0133193616437527,
-0.0036395293952584));
#53039=CARTESIAN_POINT('Ctrl Pts',(-0.0263939120873735,0.0133194541160037,
-0.00363438756270788));
#53040=CARTESIAN_POINT('Ctrl Pts',(-0.0264033661707149,0.0133195552484065,
-0.00362879869285044));
#53041=CARTESIAN_POINT('Ctrl Pts',(-0.0264210002283535,0.0133197438837884,
-0.00361837415462276));
#53042=CARTESIAN_POINT('Ctrl Pts',(-0.0264412619599893,0.0133199626359746,
-0.00360639506375529));
#53043=CARTESIAN_POINT('Ctrl Pts',(-0.0264632883923973,0.0133202033893144,
-0.00359337083805423));
#53044=CARTESIAN_POINT('Ctrl Pts',(-0.0264868575491462,0.0133204610049418,
-0.00357943439971524));
#53045=CARTESIAN_POINT('Ctrl Pts',(-0.0265124435758176,0.0133207437319668,
-0.00356430348948096));
#53046=CARTESIAN_POINT('Ctrl Pts',(-0.0265403341313379,0.0133210544187678,
-0.00354780836682767));
#53047=CARTESIAN_POINT('Ctrl Pts',(-0.0265524826683329,0.0133211897473773,
-0.00354062343974201));
#53048=CARTESIAN_POINT('Ctrl Pts',(-0.0265650682768647,0.0133213303791844,
-0.00353317977739553));
#53049=CARTESIAN_POINT('Ctrl Pts',(-0.0265781131869612,0.0133214765333346,
-0.0035254642574458));
#53050=CARTESIAN_POINT('Ctrl Pts',(-0.0266080173883094,0.0133218115776625,
-0.00350777717026943));
#53051=CARTESIAN_POINT('Ctrl Pts',(-0.0266403402986276,0.013322175706965,
-0.0034886584880915));
#53052=CARTESIAN_POINT('Ctrl Pts',(-0.0266750102819012,0.0133225682144268,
-0.00346815026368034));
#53053=CARTESIAN_POINT('Ctrl Pts',(-0.0266901854316553,0.0133227400160532,
-0.00345917375584149));
#53054=CARTESIAN_POINT('Ctrl Pts',(-0.0267058101198676,0.013322917254059,
-0.00344993110061026));
#53055=CARTESIAN_POINT('Ctrl Pts',(-0.0267218794657746,0.0133230998692401,
-0.00344042515662456));
#53056=CARTESIAN_POINT('Ctrl Pts',(-0.0267868074182936,0.0133238377231562,
-0.00340201653169836));
#53057=CARTESIAN_POINT('Ctrl Pts',(-0.0268589945355396,0.0133246635634664,
-0.00335930986383769));
#53058=CARTESIAN_POINT('Ctrl Pts',(-0.0269384557012431,0.0133255760705762,
-0.00331229269516491));
#53059=CARTESIAN_POINT('Ctrl Pts',(-0.0269881881929531,0.0133261471829161,
-0.00328286598174403));
#53060=CARTESIAN_POINT('Ctrl Pts',(-0.0270407743232821,0.0133267522722069,
-0.00325174815222461));
#53061=CARTESIAN_POINT('Ctrl Pts',(-0.0270962258102821,0.0133273907515286,
-0.0032189309120574));
#53062=CARTESIAN_POINT('Ctrl Pts',(-0.027128492095011,0.0133277622718738,
-0.00319983511368408));
#53063=CARTESIAN_POINT('Ctrl Pts',(-0.0271617320198951,0.0133281451225746,
-0.00318016186272851));
#53064=CARTESIAN_POINT('Ctrl Pts',(-0.0271959409457542,0.0133285390596639,
-0.00315991352662765));
#53065=CARTESIAN_POINT('Ctrl Pts',(-0.0272751668494086,0.0133294513952926,
-0.00311301954545746));
#53066=CARTESIAN_POINT('Ctrl Pts',(-0.0273595817593857,0.0133304232143139,
-0.00306304608089671));
#53067=CARTESIAN_POINT('Ctrl Pts',(-0.0274491686173471,0.0133314508324888,
-0.00300999805464631));
#53068=CARTESIAN_POINT('Ctrl Pts',(-0.0274935948706356,0.0133319604298378,
-0.00298369146119856));
#53069=CARTESIAN_POINT('Ctrl Pts',(-0.0275392950129729,0.0133324837470758,
-0.00295662755461286));
#53070=CARTESIAN_POINT('Ctrl Pts',(-0.0275862774756162,0.0133330202728796,
-0.00292880065737905));
#53071=CARTESIAN_POINT('',(-0.021934236877081,0.0133389875988728,-0.006269352674027));
#53072=CARTESIAN_POINT('Ctrl Pts',(-0.0219343960410907,0.0133402928895198,
-0.00626914890761956));
#53073=CARTESIAN_POINT('Ctrl Pts',(-0.0221010109600867,0.0133388040944903,
-0.00617097210686397));
#53074=CARTESIAN_POINT('Ctrl Pts',(-0.0222672606248728,0.0133373214146564,
-0.00607295491232374));
#53075=CARTESIAN_POINT('Ctrl Pts',(-0.0224327397694273,0.013335852111634,
-0.00597534331956286));
#53076=CARTESIAN_POINT('Ctrl Pts',(-0.0226194004271091,0.0133341947362031,
-0.00586523733520354));
#53077=CARTESIAN_POINT('Ctrl Pts',(-0.0228050863246761,0.0133325545074323,
-0.00575564406051703));
#53078=CARTESIAN_POINT('Ctrl Pts',(-0.0229892794527548,0.0133309487573771,
-0.00564687592167325));
#53079=CARTESIAN_POINT('Ctrl Pts',(-0.0230064944725306,0.0133307986810999,
-0.00563671025653309));
#53080=CARTESIAN_POINT('Ctrl Pts',(-0.0230236963551825,0.0133306489032939,
-0.00562655185798805));
#53081=CARTESIAN_POINT('Ctrl Pts',(-0.0230408849525679,0.0133304994498391,
-0.00561640081208492));
#53082=CARTESIAN_POINT('Ctrl Pts',(-0.0232125654633601,0.0133290067017762,
-0.00551501169308644));
#53083=CARTESIAN_POINT('Ctrl Pts',(-0.0233828973440132,0.0133275446063501,
-0.00541437248667966));
#53084=CARTESIAN_POINT('Ctrl Pts',(-0.0235554094655405,0.0133260932704177,
-0.00531240615549051));
#53085=CARTESIAN_POINT('Ctrl Pts',(-0.021934236877081,0.0133389875988728,
-0.006269352674027));
#53086=CARTESIAN_POINT('Ctrl Pts',(-0.0221244379879695,0.0132862526669668,
-0.00621537843223214));
#53087=CARTESIAN_POINT('Ctrl Pts',(-0.0223140219160993,0.0132306176275604,
-0.00616200003189472));
#53088=CARTESIAN_POINT('Ctrl Pts',(-0.0225030808082205,0.013172076313167,
-0.00610925172191726));
#53089=CARTESIAN_POINT('Ctrl Pts',(-0.0227866691464023,0.013084264341577,
-0.00603012925695107));
#53090=CARTESIAN_POINT('Ctrl Pts',(-0.0230691000748747,0.0129895128254907,
-0.00595283182554986));
#53091=CARTESIAN_POINT('Ctrl Pts',(-0.0233502330550342,0.012889386081325,
-0.00587583756451714));
#53092=CARTESIAN_POINT('Ctrl Pts',(-0.0234273680673945,0.0128619141082948,
-0.00585471249668248));
#53093=CARTESIAN_POINT('Ctrl Pts',(-0.0235043864468972,0.0128340534807241,
-0.00583360617318919));
#53094=CARTESIAN_POINT('Ctrl Pts',(-0.0235813254974928,0.0128057960779319,
-0.00581250261525141));
#53095=CARTESIAN_POINT('Ctrl Pts',(-0.0236445958273245,0.0127825587858024,
-0.00579514824109406));
#53096=CARTESIAN_POINT('Ctrl Pts',(-0.0237078125907882,0.0127590528916518,
-0.00577779571524744));
#53097=CARTESIAN_POINT('Ctrl Pts',(-0.0237709578668766,0.0127353398478756,
-0.00576044610301269));
#53098=CARTESIAN_POINT('Ctrl Pts',(-0.0239108901236044,0.0126827908697884,
-0.00572199872351335));
#53099=CARTESIAN_POINT('Ctrl Pts',(-0.0240505530379959,0.0126291559746613,
-0.00568358176343615));
#53100=CARTESIAN_POINT('Ctrl Pts',(-0.0241900554418891,0.0125744693256945,
-0.00564565827841772));
#53101=CARTESIAN_POINT('Ctrl Pts',(-0.0243428100869491,0.0125145876360655,
-0.00560413219476783));
#53102=CARTESIAN_POINT('Ctrl Pts',(-0.0244958325837244,0.0124536079758719,
-0.00556270802296106));
#53103=CARTESIAN_POINT('Ctrl Pts',(-0.0246485110185659,0.0123926840260268,
-0.00552149208076619));
#53104=CARTESIAN_POINT('Ctrl Pts',(-0.0248676533978527,0.0123052386750284,
-0.00546233402320219));
#53105=CARTESIAN_POINT('Ctrl Pts',(-0.0250860103864501,0.0122179134029239,
-0.00540356193702577));
#53106=CARTESIAN_POINT('Ctrl Pts',(-0.0253058428404908,0.0121317907564844,
-0.00534636928812283));
#53107=CARTESIAN_POINT('Ctrl Pts',(-0.025409854912204,0.0120910424742679,
-0.00531930901658501));
#53108=CARTESIAN_POINT('Ctrl Pts',(-0.025514105172312,0.0120506121521787,
-0.00529263864486529));
#53109=CARTESIAN_POINT('Ctrl Pts',(-0.0256185902781894,0.0120107696834393,
-0.00526661730777513));
#53110=CARTESIAN_POINT('Ctrl Pts',(-0.0258887931628178,0.0119077353811463,
-0.00519932503406196));
#53111=CARTESIAN_POINT('Ctrl Pts',(-0.0261609591863951,0.0118084686899625,
-0.00513642094242103));
#53112=CARTESIAN_POINT('Ctrl Pts',(-0.026435864555564,0.0117172838915229,
-0.00507630138131902));
#53113=CARTESIAN_POINT('Ctrl Pts',(-0.0267549594990146,0.0116114416222736,
-0.00500651792089364));
#53114=CARTESIAN_POINT('Ctrl Pts',(-0.0270772042033137,0.0115156201751239,
-0.00494196151769574));
#53115=CARTESIAN_POINT('Ctrl Pts',(-0.0274040024921295,0.0114364512905921,
-0.00487608698319497));
#53116=CARTESIAN_POINT('Ctrl Pts',(-0.0274676159407365,0.0114210405435357,
-0.00486326406931082));
#53117=CARTESIAN_POINT('Ctrl Pts',(-0.0275313957257365,0.0114062481348544,
-0.00485039082995094));
#53118=CARTESIAN_POINT('Ctrl Pts',(-0.0275952102983737,0.0113920884570937,
-0.00483746324422098));
#53119=CARTESIAN_POINT('Ctrl Pts',(-0.0276441660591478,0.0113812257690203,
-0.0048275457634916));
#53120=CARTESIAN_POINT('Ctrl Pts',(-0.0276931984743864,0.0113707704701278,
-0.00481753463435697));
#53121=CARTESIAN_POINT('Ctrl Pts',(-0.0277423037157662,0.011360693633868,
-0.00480744239356394));
#53122=CARTESIAN_POINT('Ctrl Pts',(-0.0279359503616762,0.0113209556041127,
-0.00476764361599214));
#53123=CARTESIAN_POINT('Ctrl Pts',(-0.0281307195105546,0.0112867138806755,
-0.0047269782631293));
#53124=CARTESIAN_POINT('Ctrl Pts',(-0.0283264381759335,0.0112568152902019,
-0.00468571290726134));
#53125=CARTESIAN_POINT('Ctrl Pts',(-0.0284781341834278,0.011233641737512,
-0.00465372929588281));
#53126=CARTESIAN_POINT('Ctrl Pts',(-0.0286304059966229,0.0112130804841673,
-0.00462138545453646));
#53127=CARTESIAN_POINT('Ctrl Pts',(-0.0287832375202268,0.0111944774250573,
-0.00458937054336652));
#53128=CARTESIAN_POINT('Ctrl Pts',(-0.0289476373790355,0.0111744662374502,
-0.00455493231523136));
#53129=CARTESIAN_POINT('Ctrl Pts',(-0.0291130260495294,0.0111571002073237,
-0.00452035107554437));
#53130=CARTESIAN_POINT('Ctrl Pts',(-0.0292789073303117,0.0111420264190303,
-0.00448619822421547));
#53131=CARTESIAN_POINT('Ctrl Pts',(-0.0299202700594218,0.0110837451834847,
-0.00435414977467429));
#53132=CARTESIAN_POINT('Ctrl Pts',(-0.0305690256497348,0.0110598368200697,
-0.00422848437704382));
#53133=CARTESIAN_POINT('Ctrl Pts',(-0.0312271855506422,0.0110770582020895,
-0.00409339326150648));
#53134=CARTESIAN_POINT('Ctrl Pts',(-0.0312271855506433,0.0110770582020895,
-0.00409339326150625));
#53135=CARTESIAN_POINT('Ctrl Pts',(-0.0312971725477488,0.0104364367400133,
-0.00488270156062033));
#53136=CARTESIAN_POINT('Ctrl Pts',(-0.0312862115324834,0.00944637453608863,
-0.00512344689700543));
#53137=CARTESIAN_POINT('Ctrl Pts',(-0.0305674031038234,0.0110597943661587,
-0.00422881741200909));
#53138=CARTESIAN_POINT('Ctrl Pts',(-0.0306178286006085,0.0103975205083563,
-0.00501002528531751));
#53139=CARTESIAN_POINT('Ctrl Pts',(-0.0305722734913362,0.00939656088554349,
-0.00522936460674402));
#53140=CARTESIAN_POINT('Ctrl Pts',(-0.0295956996016403,0.0110958118217198,
-0.00441702265247476));
#53141=CARTESIAN_POINT('Ctrl Pts',(-0.0296215818436791,0.0104181961783084,
-0.00517881942381199));
#53142=CARTESIAN_POINT('Ctrl Pts',(-0.0295240270448467,0.00942242940763544,
-0.00537967666314561));
#53143=CARTESIAN_POINT('Ctrl Pts',(-0.0283214216202437,0.0112464614327918,
-0.00468728444716199));
#53144=CARTESIAN_POINT('Ctrl Pts',(-0.028317220896715,0.0105655209977464,
-0.00541669869160581));
#53145=CARTESIAN_POINT('Ctrl Pts',(-0.028165494675058,0.00959724956687946,
-0.00560524719473936));
#53146=CARTESIAN_POINT('Ctrl Pts',(-0.0270873250160756,0.0114863644955833,
-0.00493805869436477));
#53147=CARTESIAN_POINT('Ctrl Pts',(-0.0270485620566154,0.0108042612517661,
-0.00566409311455983));
#53148=CARTESIAN_POINT('Ctrl Pts',(-0.0268298123068287,0.00984882112906849,
-0.00585320069877968));
#53149=CARTESIAN_POINT('Ctrl Pts',(-0.0259522259935078,0.0118716618249161,
-0.00517112075449145));
#53150=CARTESIAN_POINT('Ctrl Pts',(-0.0258585426933969,0.0112088416702644,
-0.00591420339096557));
#53151=CARTESIAN_POINT('Ctrl Pts',(-0.0255382372099837,0.0102851320010729,
-0.00612706727425103));
#53152=CARTESIAN_POINT('Ctrl Pts',(-0.0246675440919105,0.012385309732819,
-0.00551587592937417));
#53153=CARTESIAN_POINT('Ctrl Pts',(-0.0245918920667609,0.0117186747542567,
-0.00623782606164431));
#53154=CARTESIAN_POINT('Ctrl Pts',(-0.0242771565906109,0.0108089452162191,
-0.00644811086918074));
#53155=CARTESIAN_POINT('Ctrl Pts',(-0.0232306431468797,0.0129584151226383,
-0.00590506038327814));
#53156=CARTESIAN_POINT('Ctrl Pts',(-0.0232456059885352,0.0122404369636077,
-0.00664101298772188));
#53157=CARTESIAN_POINT('Ctrl Pts',(-0.0230068651290133,0.0112567720241337,
-0.00682535438580635));
#53158=CARTESIAN_POINT('Ctrl Pts',(-0.0213063980437958,0.0135554252605759,
-0.00644100233681364));
#53159=CARTESIAN_POINT('Ctrl Pts',(-0.0214852275357793,0.0127443835685822,
-0.00728906181719641));
#53160=CARTESIAN_POINT('Ctrl Pts',(-0.0213700943777464,0.0115684868389236,
-0.00741362551099617));
#53161=CARTESIAN_POINT('Ctrl Pts',(-0.0189589293125837,0.0139588978082077,
-0.00714392830883555));
#53162=CARTESIAN_POINT('Ctrl Pts',(-0.0193481840631595,0.0130853604144522,
-0.0081987090774338));
#53163=CARTESIAN_POINT('Ctrl Pts',(-0.0193354807706988,0.0116626127714134,
-0.00825016263078458));
#53164=CARTESIAN_POINT('Ctrl Pts',(-0.0170471348458498,0.0141103532818413,
-0.00776507163445552));
#53165=CARTESIAN_POINT('Ctrl Pts',(-0.0176087403647826,0.0132343476767644,
-0.00899849195367984));
#53166=CARTESIAN_POINT('Ctrl Pts',(-0.0176504495282693,0.0116214653221526,
-0.00900227953763803));
#53167=CARTESIAN_POINT('Ctrl Pts',(-0.0155198771543919,0.0141607759349565,
-0.00827772815388904));
#53168=CARTESIAN_POINT('Ctrl Pts',(-0.0162143626795666,0.0133115262354637,
-0.00966525099856111));
#53169=CARTESIAN_POINT('Ctrl Pts',(-0.0163007154697231,0.0115450617448305,
-0.00963487767203659));
#53170=CARTESIAN_POINT('Ctrl Pts',(-0.0147476420715683,0.0141642785739701,
-0.00853349038223322));
#53171=CARTESIAN_POINT('Ctrl Pts',(-0.0155272812960161,0.0133414507084357,
-0.010003407102025));
#53172=CARTESIAN_POINT('Ctrl Pts',(-0.0156467725429645,0.0114898180989373,
-0.00995062286346207));
#53173=CARTESIAN_POINT('Ctrl Pts',(-0.0143548534745897,0.0141605057808234,
-0.00865910748104471));
#53174=CARTESIAN_POINT('Ctrl Pts',(-0.0151686127038861,0.0133556215237912,
-0.0101803383457646));
#53175=CARTESIAN_POINT('Ctrl Pts',(-0.0153031792648842,0.0114576562027847,
-0.0101186490016487));
#53176=CARTESIAN_POINT('',(-0.0199408189736793,0.0133213265168279,-0.0073387013155759));
#53177=CARTESIAN_POINT('Ctrl Pts',(-0.0219342368770961,0.0133389875988686,
-0.00626935267402273));
#53178=CARTESIAN_POINT('Ctrl Pts',(-0.0217376785013481,0.0133366453122945,
-0.00639030610905115));
#53179=CARTESIAN_POINT('Ctrl Pts',(-0.0215381987658809,0.0133344476531088,
-0.00650627497520774));
#53180=CARTESIAN_POINT('Ctrl Pts',(-0.021336704249506,0.0133323524489406,
-0.00661859857317656));
#53181=CARTESIAN_POINT('Ctrl Pts',(-0.0208796013372672,0.0133275993472472,
-0.00687341168009572));
#53182=CARTESIAN_POINT('Ctrl Pts',(-0.0204118273091042,0.0133241114174165,
-0.00710983367692451));
#53183=CARTESIAN_POINT('Ctrl Pts',(-0.0199408531165797,0.0133213859277168,
-0.00733877226188682));
#53184=CARTESIAN_POINT('',(-0.0179635469613193,0.0125504668006521,-0.00868818357736758));
#53185=CARTESIAN_POINT('Ctrl Pts',(-0.019940832013525,0.013321303084259,
-0.00733866153639121));
#53186=CARTESIAN_POINT('Ctrl Pts',(-0.0199603396185445,0.0132772806325954,
-0.00736654069053705));
#53187=CARTESIAN_POINT('Ctrl Pts',(-0.0199132772454676,0.0132018530803466,
-0.00744866955051636));
#53188=CARTESIAN_POINT('Ctrl Pts',(-0.0197781204736182,0.0131072852390325,
-0.00758075520135114));
#53189=CARTESIAN_POINT('Ctrl Pts',(-0.0195745132232924,0.0130117329433713,
-0.00773781403254475));
#53190=CARTESIAN_POINT('Ctrl Pts',(-0.0193204817770644,0.0129169799429281,
-0.00790952535011119));
#53191=CARTESIAN_POINT('Ctrl Pts',(-0.0189699447034221,0.0128035104283324,
-0.00812880984283259));
#53192=CARTESIAN_POINT('Ctrl Pts',(-0.0185188307304575,0.0126793170927796,
-0.00838884190036944));
#53193=CARTESIAN_POINT('Ctrl Pts',(-0.018149541483532,0.0125918489633789,
-0.00858915670411014));
#53194=CARTESIAN_POINT('Ctrl Pts',(-0.0179635437328199,0.0125504640932136,
-0.00868817638106961));
#53195=CARTESIAN_POINT('Ctrl Pts',(-0.0179635534180534,0.0125504722160869,
-0.00868819796987369));
#53196=CARTESIAN_POINT('Ctrl Pts',(-0.0177344418480487,0.0124994925802867,
-0.00881016396521778));
#53197=CARTESIAN_POINT('Ctrl Pts',(-0.0175066087155722,0.0124440548773491,
-0.00893192475792164));
#53198=CARTESIAN_POINT('Ctrl Pts',(-0.0172802067201601,0.0123833234404231,
-0.00905334530314095));
#53199=CARTESIAN_POINT('Ctrl Pts',(-0.0172702574635162,0.0123806545918061,
-0.00905868114023916));
#53200=CARTESIAN_POINT('Ctrl Pts',(-0.0172603111720795,0.0123779754035313,
-0.00906401620513647));
#53201=CARTESIAN_POINT('Ctrl Pts',(-0.0172503677772368,0.0123752856701961,
-0.00906935054629216));
#53202=CARTESIAN_POINT('Ctrl Pts',(-0.0170340425658767,0.0123167687208602,
-0.00918540270918222));
#53203=CARTESIAN_POINT('Ctrl Pts',(-0.0168190666854423,0.0122533080221976,
-0.00930117599300669));
#53204=CARTESIAN_POINT('Ctrl Pts',(-0.0166061640651018,0.0121821155570041,
-0.00941621999680577));
#53205=CARTESIAN_POINT('Ctrl Pts',(-0.0164948197172596,0.012144883142506,
-0.00947638599925169));
#53206=CARTESIAN_POINT('Ctrl Pts',(-0.016384039145408,0.0121055365709686,
-0.00953635007489573));
#53207=CARTESIAN_POINT('Ctrl Pts',(-0.0162739869952414,0.0120629969620388,
-0.00959602607418241));
#53208=CARTESIAN_POINT('Ctrl Pts',(-0.0162700848817242,0.0120614886372785,
-0.00959814200306811));
#53209=CARTESIAN_POINT('Ctrl Pts',(-0.0162661836345646,0.0120599763009443,
-0.00960025757130618));
#53210=CARTESIAN_POINT('Ctrl Pts',(-0.0162622833351437,0.0120584598728285,
-0.00960237274228974));
#53211=CARTESIAN_POINT('Ctrl Pts',(-0.01615618264775,0.0120172081513313,
-0.00965991219531522));
#53212=CARTESIAN_POINT('Ctrl Pts',(-0.0160507954251391,0.0119729279934615,
-0.00971718141157779));
#53213=CARTESIAN_POINT('Ctrl Pts',(-0.0159468166798295,0.0119240122610053,
-0.0097736976224013));
#53214=CARTESIAN_POINT('Ctrl Pts',(-0.0158390156384532,0.0118732983686345,
-0.00983229138945709));
#53215=CARTESIAN_POINT('Ctrl Pts',(-0.0157327819795801,0.0118176187396,
-0.00989018624054665));
#53216=CARTESIAN_POINT('Ctrl Pts',(-0.0156332637808036,0.0117499022711538,
-0.00994442202611638));
#53217=CARTESIAN_POINT('Ctrl Pts',(-0.0155835046814153,0.0117160440369307,
-0.00997153991890124));
#53218=CARTESIAN_POINT('Ctrl Pts',(-0.0155354394278101,0.0116791790329133,
-0.00999777428168848));
#53219=CARTESIAN_POINT('Ctrl Pts',(-0.0154908483194925,0.0116337739903578,
-0.0100220264279572));
#53220=CARTESIAN_POINT('Ctrl Pts',(-0.0154462572111749,0.0115883689478023,
-0.0100462785742259));
#53221=CARTESIAN_POINT('Ctrl Pts',(-0.015405193404354,0.0115344307061892,
-0.0100686588757623));
#53222=CARTESIAN_POINT('Ctrl Pts',(-0.0153993022433837,0.0114667765373356,
-0.0100716954734325));
#53223=CARTESIAN_POINT('Ctrl Pts',(-0.031227186149515,0.0110770527203336,
-0.00409340001554567));
#53224=CARTESIAN_POINT('Ctrl Pts',(-0.0312640532610597,0.0107214346812047,
-0.00453189580156053));
#53225=CARTESIAN_POINT('Ctrl Pts',(-0.0312844616188089,0.0102385845359009,
-0.00486793065315416));
#53226=CARTESIAN_POINT('Ctrl Pts',(-0.031286535045435,0.00970177877551689,
-0.00504944931744486));
#53227=CARTESIAN_POINT('Ctrl Pts',(-0.0312868594344739,0.00961779514064571,
-0.00507784803882443));
#53228=CARTESIAN_POINT('Ctrl Pts',(-0.0312867487379335,0.00953254752741736,
-0.00510254750827983));
#53229=CARTESIAN_POINT('Ctrl Pts',(-0.031286211601055,0.00944638135331241,
-0.00512344524021589));
#53230=CARTESIAN_POINT('Origin',(-0.0317929661854822,0.00871120572661458,
-0.00213559619862456));
#53231=CARTESIAN_POINT('Ctrl Pts',(-0.0348080115825784,0.00509687525187179,
-0.00461569088578222));
#53232=CARTESIAN_POINT('Ctrl Pts',(-0.0347548891167709,0.00446629142979133,
-0.00433411181330694));
#53233=CARTESIAN_POINT('Ctrl Pts',(-0.0346843926247131,0.00402081228213221,
-0.0038052049414957));
#53234=CARTESIAN_POINT('Ctrl Pts',(-0.0332875621972097,0.00551905813026757,
-0.0048853855816232));
#53235=CARTESIAN_POINT('Ctrl Pts',(-0.0332621390258117,0.00478601213496154,
-0.00466482167991226));
#53236=CARTESIAN_POINT('Ctrl Pts',(-0.0332218425615931,0.00424926308106939,
-0.00412352454144985));
#53237=CARTESIAN_POINT('Ctrl Pts',(-0.0316267399577887,0.00557241894549665,
-0.00506047006495692));
#53238=CARTESIAN_POINT('Ctrl Pts',(-0.0316907003603952,0.00481889725260965,
-0.00486557021719565));
#53239=CARTESIAN_POINT('Ctrl Pts',(-0.0316934649721066,0.00425079470032948,
-0.00433058506958464));
#53240=CARTESIAN_POINT('Ctrl Pts',(-0.0298458444280582,0.00532758970197972,
-0.0052928024035983));
#53241=CARTESIAN_POINT('Ctrl Pts',(-0.0299584793993426,0.00461004696303067,
-0.00511576159414239));
#53242=CARTESIAN_POINT('Ctrl Pts',(-0.0300009414693827,0.00405085754226072,
-0.00462151390208107));
#53243=CARTESIAN_POINT('Ctrl Pts',(-0.0290810914906223,0.00518348075480775,
-0.00539636057852287));
#53244=CARTESIAN_POINT('Ctrl Pts',(-0.0292393121166008,0.00446527121083198,
-0.00521590130342139));
#53245=CARTESIAN_POINT('Ctrl Pts',(-0.0293136858521343,0.00390564420165416,
-0.0047116415943142));
#53246=CARTESIAN_POINT('Ctrl Pts',(-0.0281474033824572,0.00491192722094244,
-0.00552736398019822));
#53247=CARTESIAN_POINT('Ctrl Pts',(-0.0283533171115081,0.00421434854492473,
-0.00534056257578605));
#53248=CARTESIAN_POINT('Ctrl Pts',(-0.0284603778430982,0.00366783441342131,
-0.00483752590032366));
#53249=CARTESIAN_POINT('Ctrl Pts',(-0.0272393145892442,0.00454861707918601,
-0.00567042035975692));
#53250=CARTESIAN_POINT('Ctrl Pts',(-0.0274894758152918,0.00387773041136884,
-0.00547497754196955));
#53251=CARTESIAN_POINT('Ctrl Pts',(-0.0276272202063975,0.00334894460118206,
-0.00497305746395805));
#53252=CARTESIAN_POINT('Ctrl Pts',(-0.0265464409363679,0.00419219894647591,
-0.00578556885600068));
#53253=CARTESIAN_POINT('Ctrl Pts',(-0.0268232619974109,0.00355649862073227,
-0.00558171480714852));
#53254=CARTESIAN_POINT('Ctrl Pts',(-0.0269828211829138,0.00305252022388036,
-0.00508905472630933));
#53255=CARTESIAN_POINT('Ctrl Pts',(-0.025861152465289,0.00386425555365813,
-0.00591958411161263));
#53256=CARTESIAN_POINT('Ctrl Pts',(-0.0261693159050445,0.00323236615942843,
-0.00571374798206362));
#53257=CARTESIAN_POINT('Ctrl Pts',(-0.0263470523169275,0.00272876851477799,
-0.00521258592314838));
#53258=CARTESIAN_POINT('Ctrl Pts',(-0.0250286088285531,0.0034052289470929,
-0.00610437205199126));
#53259=CARTESIAN_POINT('Ctrl Pts',(-0.0253626046700147,0.00278416555730594,
-0.00589816148590217));
#53260=CARTESIAN_POINT('Ctrl Pts',(-0.0255523751777655,0.00228207997173738,
-0.0053963585446636));
#53261=CARTESIAN_POINT('Ctrl Pts',(-0.0237145546648394,0.00263062411308175,
-0.00645442168636818));
#53262=CARTESIAN_POINT('Ctrl Pts',(-0.0240193050878441,0.00200028219795834,
-0.00626378438987051));
#53263=CARTESIAN_POINT('Ctrl Pts',(-0.024174135008249,0.00147561881341623,
-0.00578692718671447));
#53264=CARTESIAN_POINT('Ctrl Pts',(-0.0219731049140079,0.00187183481145798,
-0.0070682386857302));
#53265=CARTESIAN_POINT('Ctrl Pts',(-0.0221573770271123,0.00111225139363262,
-0.00692816079214065));
#53266=CARTESIAN_POINT('Ctrl Pts',(-0.0221889912973933,0.000481700437360768,
-0.00644789501881987));
#53267=CARTESIAN_POINT('Ctrl Pts',(-0.0196577522133193,0.00149257628269449,
-0.00806059618661361));
#53268=CARTESIAN_POINT('Ctrl Pts',(-0.01973610478976,0.00050921641839706,
-0.00798804692450031));
#53269=CARTESIAN_POINT('Ctrl Pts',(-0.0195902622436619,-0.000263255730683529,
-0.00738835747518616));
#53270=CARTESIAN_POINT('Ctrl Pts',(-0.0173546263616046,0.00138324422282633,
-0.00913020895521079));
#53271=CARTESIAN_POINT('Ctrl Pts',(-0.0173769785163834,0.000198590709853074,
-0.00910811698131738));
#53272=CARTESIAN_POINT('Ctrl Pts',(-0.0170772860700991,-0.00066260666126077,
-0.00835060388230459));
#53273=CARTESIAN_POINT('Ctrl Pts',(-0.0158446688321696,0.00138690879226211,
-0.00986871486838659));
#53274=CARTESIAN_POINT('Ctrl Pts',(-0.0158406071373422,8.7294300466045E-5,
-0.00987123115306857));
#53275=CARTESIAN_POINT('Ctrl Pts',(-0.0154232695854763,-0.000803047871763627,
-0.0090213459552702));
#53276=CARTESIAN_POINT('Ctrl Pts',(-0.0150619153852245,0.00140071328882223,
-0.0102593577757051));
#53277=CARTESIAN_POINT('Ctrl Pts',(-0.0150568244437027,4.45394858915551E-5,
-0.0102669524250396));
#53278=CARTESIAN_POINT('Ctrl Pts',(-0.0145987801442292,-0.000854777680999614,
-0.00936101918622224));
#53279=CARTESIAN_POINT('',(-0.0168559418075085,0.000684768142416315,-0.00927936853839009));
#53280=CARTESIAN_POINT('Ctrl Pts',(-0.0151728897383989,0.00139471190135993,
-0.0102040357394328));
#53281=CARTESIAN_POINT('Ctrl Pts',(-0.0151702322536255,0.00130488215101023,
-0.0102055148167351));
#53282=CARTESIAN_POINT('Ctrl Pts',(-0.015239223527948,0.00124141684161519,
-0.0101673535957409));
#53283=CARTESIAN_POINT('Ctrl Pts',(-0.015307419695405,0.00119164723569968,
-0.0101297968191818));
#53284=CARTESIAN_POINT('Ctrl Pts',(-0.0153756158628621,0.00114187762978418,
-0.0100922400426227));
#53285=CARTESIAN_POINT('Ctrl Pts',(-0.0154428915182541,0.0011058242963998,
-0.0100550351968635));
#53286=CARTESIAN_POINT('Ctrl Pts',(-0.0155132948332529,0.00107284990167657,
-0.0100162560632439));
#53287=CARTESIAN_POINT('Ctrl Pts',(-0.0155836981482517,0.00103987550695335,
-0.00997747692962429));
#53288=CARTESIAN_POINT('Ctrl Pts',(-0.0156571625546665,0.00100999302216499,
-0.00993698931508581));
#53289=CARTESIAN_POINT('Ctrl Pts',(-0.0157307971901185,0.000982771995278683,
-0.0098964483681575));
#53290=CARTESIAN_POINT('Ctrl Pts',(-0.0158044318255704,0.00095555096839237,
-0.00985590742122919));
#53291=CARTESIAN_POINT('Ctrl Pts',(-0.0158782380885874,0.000930990288587306,
-0.00981531602417939));
#53292=CARTESIAN_POINT('Ctrl Pts',(-0.0159524436492681,0.000907913501193525,
-0.00977452964654521));
#53293=CARTESIAN_POINT('Ctrl Pts',(-0.0161008547706294,0.000861759926405962,
-0.00969295689127685));
#53294=CARTESIAN_POINT('Ctrl Pts',(-0.0162508630387447,0.000821543067736549,
-0.00961060403861727));
#53295=CARTESIAN_POINT('Ctrl Pts',(-0.0164016269412466,0.000784896664753995,
-0.00952797982903137));
#53296=CARTESIAN_POINT('Ctrl Pts',(-0.0165523908437485,0.000748250261771441,
-0.00944535561944546));
#53297=CARTESIAN_POINT('Ctrl Pts',(-0.0167038987539332,0.000715179656409445,
-0.00936243640413805));
#53298=CARTESIAN_POINT('Ctrl Pts',(-0.0168559418075085,0.000684768142416308,
-0.00927936853839006));
#53299=CARTESIAN_POINT('',(-0.0184101558320655,0.000106937857928987,-0.00826148684386422));
#53300=CARTESIAN_POINT('Ctrl Pts',(-0.0168559106004127,0.000684785839446314,
-0.00927930493960189));
#53301=CARTESIAN_POINT('Ctrl Pts',(-0.0169994384641672,0.000656074616975346,
-0.00920091587798125));
#53302=CARTESIAN_POINT('Ctrl Pts',(-0.0171422855111684,0.000625624189261452,
-0.00912181819303145));
#53303=CARTESIAN_POINT('Ctrl Pts',(-0.0172838503930251,0.000592876796398921,
-0.00904172279456659));
#53304=CARTESIAN_POINT('Ctrl Pts',(-0.0172953475013133,0.000590217236224398,
-0.00903521789407531));
#53305=CARTESIAN_POINT('Ctrl Pts',(-0.0173068366582681,0.000587541830465944,
-0.00902870590106529));
#53306=CARTESIAN_POINT('Ctrl Pts',(-0.0173183167955872,0.000584850350612705,
-0.00902218702064899));
#53307=CARTESIAN_POINT('Ctrl Pts',(-0.0174481925751245,0.000554401407857755,
-0.0089484383665829));
#53308=CARTESIAN_POINT('Ctrl Pts',(-0.0175769158543567,0.000521907202193238,
-0.00887381668562478));
#53309=CARTESIAN_POINT('Ctrl Pts',(-0.0177038524404219,0.000486178880005269,
-0.00879763432014667));
#53310=CARTESIAN_POINT('Ctrl Pts',(-0.0177226207864461,0.000480896230341577,
-0.00878637029422195));
#53311=CARTESIAN_POINT('Ctrl Pts',(-0.0177413352367826,0.000475534680172062,
-0.00877507626560524));
#53312=CARTESIAN_POINT('Ctrl Pts',(-0.017760009234808,0.000470092158801244,
-0.00876374276261054));
#53313=CARTESIAN_POINT('Ctrl Pts',(-0.0178100664404382,0.000455503027377121,
-0.00873336236473615));
#53314=CARTESIAN_POINT('Ctrl Pts',(-0.0178598386157251,0.000440337954000094,
-0.00870269839544443));
#53315=CARTESIAN_POINT('Ctrl Pts',(-0.017909104476756,0.000424382586793304,
-0.00867169456780072));
#53316=CARTESIAN_POINT('Ctrl Pts',(-0.0179767491222203,0.000402475019659202,
-0.00862912466472574));
#53317=CARTESIAN_POINT('Ctrl Pts',(-0.0180435462459668,0.000379119629529094,
-0.00858589778545374));
#53318=CARTESIAN_POINT('Ctrl Pts',(-0.0181099233481851,0.000352507988189935,
-0.00854072977249054));
#53319=CARTESIAN_POINT('Ctrl Pts',(-0.0181289719923642,0.000344871082239675,
-0.008527767630751));
#53320=CARTESIAN_POINT('Ctrl Pts',(-0.0181478033724562,0.000337023540513838,
-0.00851476104835145));
#53321=CARTESIAN_POINT('Ctrl Pts',(-0.0181663678145007,0.00032895373681883,
-0.00850172329166989));
#53322=CARTESIAN_POINT('Ctrl Pts',(-0.0182124932189159,0.000308903419222881,
-0.00846932954678046));
#53323=CARTESIAN_POINT('Ctrl Pts',(-0.0182569831984907,0.000287497097208199,
-0.00843674620973055));
#53324=CARTESIAN_POINT('Ctrl Pts',(-0.0182974687017753,0.000262756868223345,
-0.00840386569127419));
#53325=CARTESIAN_POINT('Ctrl Pts',(-0.0183104033003802,0.00025485268264208,
-0.00839336078770008));
#53326=CARTESIAN_POINT('Ctrl Pts',(-0.0183233624796087,0.000246284839621537,
-0.00838244445279732));
#53327=CARTESIAN_POINT('Ctrl Pts',(-0.0183361960489214,0.000236921585224982,
-0.00837109800055212));
#53328=CARTESIAN_POINT('Ctrl Pts',(-0.0183515307372761,0.000225733537328151,
-0.00835754025173936));
#53329=CARTESIAN_POINT('Ctrl Pts',(-0.0183667534635429,0.000213411283286992,
-0.00834333641976299));
#53330=CARTESIAN_POINT('Ctrl Pts',(-0.0183798354311663,0.000199713718176209,
-0.00832931041010002));
#53331=CARTESIAN_POINT('Ctrl Pts',(-0.0184038656707308,0.000174552688846439,
-0.00830354606164427));
#53332=CARTESIAN_POINT('Ctrl Pts',(-0.0184222097745657,0.000144872070237118,
-0.00827771743599519));
#53333=CARTESIAN_POINT('Ctrl Pts',(-0.0184101558320613,0.000106937857930527,
-0.00826148684386729));
#53334=CARTESIAN_POINT('Ctrl Pts',(-0.0184101558320655,0.000106937857928987,
-0.00826148684386422));
#53335=CARTESIAN_POINT('Ctrl Pts',(-0.0191899749903914,0.00010230128487336,
-0.00785918081542734));
#53336=CARTESIAN_POINT('Ctrl Pts',(-0.0199660898324893,9.51225642974071E-5,
-0.00744873103086231));
#53337=CARTESIAN_POINT('Ctrl Pts',(-0.0207149455884367,8.43554830514994E-5,
-0.00699117714319491));
#53338=CARTESIAN_POINT('Ctrl Pts',(-0.0328171226457405,0.00544959479189026,
-0.00491819444776802));
#53339=CARTESIAN_POINT('Ctrl Pts',(-0.0328195640571706,0.00498233590672909,
-0.00477513152938287));
#53340=CARTESIAN_POINT('Ctrl Pts',(-0.0328127292790594,0.00455105192850437,
-0.00451607286816002));
#53341=CARTESIAN_POINT('Ctrl Pts',(-0.0327968763129483,0.00420555010966588,
-0.0041712068084503));
#53342=CARTESIAN_POINT('Origin',(-0.034273100524039,0.0063892955694362,
-0.00193093091927896));
#53343=CARTESIAN_POINT('Ctrl Pts',(-0.0337145948616341,0.00415833566999661,
0.00401503462776478));
#53344=CARTESIAN_POINT('Ctrl Pts',(-0.0337504898950536,0.00448210638016595,
0.00435737005883901));
#53345=CARTESIAN_POINT('Ctrl Pts',(-0.0337798713312579,0.00488841094225288,
0.00462212049130278));
#53346=CARTESIAN_POINT('Ctrl Pts',(-0.0337993965723764,0.00533366251113205,
0.00478061601362495));
#53347=CARTESIAN_POINT('Ctrl Pts',(-0.0326387926265156,0.00424057900937983,
0.00419929895082685));
#53348=CARTESIAN_POINT('Ctrl Pts',(-0.0326521120878623,0.00459856815265706,
0.0045522680694765));
#53349=CARTESIAN_POINT('Ctrl Pts',(-0.0326523815453445,0.00504644076338797,
0.00481398643458415));
#53350=CARTESIAN_POINT('Ctrl Pts',(-0.0326395047684778,0.00552995296452442,
0.00495256740652356));
#53351=CARTESIAN_POINT('Ctrl Pts',(-0.0307995994291534,0.00425190175201537,
0.004505296988018));
#53352=CARTESIAN_POINT('Ctrl Pts',(-0.0307898334715919,0.00462109727731803,
0.00482527566892104));
#53353=CARTESIAN_POINT('Ctrl Pts',(-0.0307597745982798,0.00506856871463487,
0.00505436659406124));
#53354=CARTESIAN_POINT('Ctrl Pts',(-0.0307129201916643,0.00554291348277156,
0.00516623054628213));
#53355=CARTESIAN_POINT('Ctrl Pts',(-0.0284413845216665,0.00372335549694271,
0.00483605952326099));
#53356=CARTESIAN_POINT('Ctrl Pts',(-0.0283698180551898,0.00408268647934982,
0.00516184559608916));
#53357=CARTESIAN_POINT('Ctrl Pts',(-0.0282601549337502,0.00451602599614115,
0.00539830518908961));
#53358=CARTESIAN_POINT('Ctrl Pts',(-0.0281250818282017,0.00497353878031065,
0.00551806473009416));
#53359=CARTESIAN_POINT('Ctrl Pts',(-0.026503416926424,0.00285775025295423,
0.00515034561794722));
#53360=CARTESIAN_POINT('Ctrl Pts',(-0.0263806195395379,0.00317751670560064,
0.00547519490900795));
#53361=CARTESIAN_POINT('Ctrl Pts',(-0.0262066562740293,0.0035592412880712,
0.00571951320274019));
#53362=CARTESIAN_POINT('Ctrl Pts',(-0.0260003497552778,0.0039618848035107,
0.00585689946815495));
#53363=CARTESIAN_POINT('Ctrl Pts',(-0.0245731919014548,0.00166880228110552,
0.00564722242151088));
#53364=CARTESIAN_POINT('Ctrl Pts',(-0.0244513567483743,0.00199858974938907,
0.0059608556267388));
#53365=CARTESIAN_POINT('Ctrl Pts',(-0.0242720553711055,0.00238236582209498,
0.00619499515250578));
#53366=CARTESIAN_POINT('Ctrl Pts',(-0.0240543129347437,0.00277916645442249,
0.00632454923114672));
#53367=CARTESIAN_POINT('Ctrl Pts',(-0.0221706253086404,0.00046612601988525,
0.00645018290437898));
#53368=CARTESIAN_POINT('Ctrl Pts',(-0.0221581341038569,0.000880257985322814,
0.00675728529047529));
#53369=CARTESIAN_POINT('Ctrl Pts',(-0.0220849415751972,0.00136253175593733,
0.00696991151781838));
#53370=CARTESIAN_POINT('Ctrl Pts',(-0.0219616170038293,0.00185499085047183,
0.00706158768923822));
#53371=CARTESIAN_POINT('Ctrl Pts',(-0.0195701738987167,-0.000266550805092657,
0.00739523959835644));
#53372=CARTESIAN_POINT('Ctrl Pts',(-0.0196760856193404,0.000234542108405088,
0.00777465949313878));
#53373=CARTESIAN_POINT('Ctrl Pts',(-0.0197001203513376,0.000858128190769441,
0.00801082445085077));
#53374=CARTESIAN_POINT('Ctrl Pts',(-0.0196397060603481,0.0014900587499245,
0.00805989029189566));
#53375=CARTESIAN_POINT('Ctrl Pts',(-0.0167705697451759,-0.000704592537367574,
0.00847417313657492));
#53376=CARTESIAN_POINT('Ctrl Pts',(-0.0169829836419465,-0.000149778270697148,
0.00895736442962707));
#53377=CARTESIAN_POINT('Ctrl Pts',(-0.0170929548817286,0.000609089429017907,
0.00924272341216823));
#53378=CARTESIAN_POINT('Ctrl Pts',(-0.0170734273265382,0.00137323317849824,
0.00925507608132262));
#53379=CARTESIAN_POINT('Ctrl Pts',(-0.0148407380900652,-0.000839331357905782,
0.00927002324422269));
#53380=CARTESIAN_POINT('Ctrl Pts',(-0.015129397707141,-0.000273240055481486,
0.00981783425117302));
#53381=CARTESIAN_POINT('Ctrl Pts',(-0.0153048081511204,0.000560629512514839,
0.0101375931190703));
#53382=CARTESIAN_POINT('Ctrl Pts',(-0.015311716611075,0.00139891690278659,
0.0101278799490686));
#53383=CARTESIAN_POINT('Ctrl Pts',(-0.0137268720321833,-0.000892677918735118,
0.00973665336335839));
#53384=CARTESIAN_POINT('Ctrl Pts',(-0.0140290905698997,-0.000325814591128036,
0.0103371273983254));
#53385=CARTESIAN_POINT('Ctrl Pts',(-0.0142143926766274,0.000548607912082809,
0.0106939538304117));
#53386=CARTESIAN_POINT('Ctrl Pts',(-0.0142179384615059,0.00142799346296082,
0.0106828353729555));
#53387=CARTESIAN_POINT('',(-0.0184512676916217,0.000107246345742279,0.00823734004344498));
#53388=CARTESIAN_POINT('Ctrl Pts',(-0.0207569019187454,8.46249604678063E-5,
0.00696635255655076));
#53389=CARTESIAN_POINT('Ctrl Pts',(-0.0200077628358915,9.54352636376166E-5,
0.00742407896483524));
#53390=CARTESIAN_POINT('Ctrl Pts',(-0.0192312828839955,0.000102624232462172,
0.00783467988302133));
#53391=CARTESIAN_POINT('Ctrl Pts',(-0.0184512581841375,0.000107246022242465,
0.0082373457726289));
#53392=CARTESIAN_POINT('',(-0.0168949674403344,0.000683552764475077,0.00925478469399231));
#53393=CARTESIAN_POINT('Ctrl Pts',(-0.0184512676916217,0.000107246345742279,
0.00823734004344498));
#53394=CARTESIAN_POINT('Ctrl Pts',(-0.0184622301433659,0.000141599751249758,
0.00825191867407648));
#53395=CARTESIAN_POINT('Ctrl Pts',(-0.0184456858101158,0.000172716967409295,
0.00827767057001621));
#53396=CARTESIAN_POINT('Ctrl Pts',(-0.018421873317597,0.000198254458454251,
0.00830351846934873));
#53397=CARTESIAN_POINT('Ctrl Pts',(-0.0184104929975665,0.00021045917917544,
0.0083158715384904));
#53398=CARTESIAN_POINT('Ctrl Pts',(-0.0183975628351906,0.000221439064276058,
0.00832822607534285));
#53399=CARTESIAN_POINT('Ctrl Pts',(-0.0183844216172855,0.000231486145171871,
0.00834010980452181));
#53400=CARTESIAN_POINT('Ctrl Pts',(-0.0183700657918549,0.000242461850808103,
0.00835309191491602));
#53401=CARTESIAN_POINT('Ctrl Pts',(-0.01835540146337,0.000252330125039528,
0.00836554321037133));
#53402=CARTESIAN_POINT('Ctrl Pts',(-0.0183404924684894,0.000261530264194091,
0.00837769350203077));
#53403=CARTESIAN_POINT('Ctrl Pts',(-0.0183019237969097,0.000285330469934476,
0.00840912557457252));
#53404=CARTESIAN_POINT('Ctrl Pts',(-0.0182596528414629,0.000305730744391114,
0.00844011593411856));
#53405=CARTESIAN_POINT('Ctrl Pts',(-0.0182160609702212,0.000324884503226279,
0.00847085444561481));
#53406=CARTESIAN_POINT('Ctrl Pts',(-0.0181951012398468,0.000334093963829995,
0.00848563405692127));
#53407=CARTESIAN_POINT('Ctrl Pts',(-0.0181738267201503,0.000343006968918949,
0.00850035502957633));
#53408=CARTESIAN_POINT('Ctrl Pts',(-0.0181522729621096,0.000351651856950548,
0.00851502182610127));
#53409=CARTESIAN_POINT('Ctrl Pts',(-0.018085891879075,0.000378276310522332,
0.00856019250288709));
#53410=CARTESIAN_POINT('Ctrl Pts',(-0.0180189689159113,0.000401641369382736,
0.00860349488247737));
#53411=CARTESIAN_POINT('Ctrl Pts',(-0.0179511291677144,0.000423553630764221,
0.00864618006740678));
#53412=CARTESIAN_POINT('Ctrl Pts',(-0.0179036725263837,0.000438882141803327,
0.00867604007669589));
#53413=CARTESIAN_POINT('Ctrl Pts',(-0.0178557140104046,0.000453480053782304,
0.00870560687033));
#53414=CARTESIAN_POINT('Ctrl Pts',(-0.017807482880896,0.000467540968088816,
0.00873491305520521));
#53415=CARTESIAN_POINT('Ctrl Pts',(-0.0177867671235334,0.000473580272829081,
0.0087475003576649));
#53416=CARTESIAN_POINT('Ctrl Pts',(-0.0177660002240907,0.000479519756530131,
0.0087600396106193));
#53417=CARTESIAN_POINT('Ctrl Pts',(-0.0177451711391999,0.000485363451470148,
0.00877254070523275));
#53418=CARTESIAN_POINT('Ctrl Pts',(-0.0176186513664753,0.000520859151812222,
0.00884847470125778));
#53419=CARTESIAN_POINT('Ctrl Pts',(-0.0174903687188125,0.000553070032504836,
0.00892284009755575));
#53420=CARTESIAN_POINT('Ctrl Pts',(-0.0173611017027544,0.000583240788244276,
0.00899628311459254));
#53421=CARTESIAN_POINT('Ctrl Pts',(-0.017348709986102,0.000586132999016321,
0.0090033234647528));
#53422=CARTESIAN_POINT('Ctrl Pts',(-0.0173363090600306,0.000589006309522193,
0.00901035529404749));
#53423=CARTESIAN_POINT('Ctrl Pts',(-0.0173238992320563,0.000591861210441433,
0.00901737890518302));
#53424=CARTESIAN_POINT('Ctrl Pts',(-0.017182033455642,0.000624497660868489,
0.00909767091640441));
#53425=CARTESIAN_POINT('Ctrl Pts',(-0.0170390390744304,0.000654793151863181,
0.00917689686737658));
#53426=CARTESIAN_POINT('Ctrl Pts',(-0.0168953032845727,0.000683360688020473,
0.00925546810437223));
#53427=CARTESIAN_POINT('Ctrl Pts',(-0.0168945268806226,0.000683804758467406,
0.00925388800048686));
#53428=CARTESIAN_POINT('Ctrl Pts',(-0.0167416908614446,0.000714147179609983,
0.00933751330057378));
#53429=CARTESIAN_POINT('Ctrl Pts',(-0.0165893391680148,0.000747133161909586,
0.00942105041880093));
#53430=CARTESIAN_POINT('Ctrl Pts',(-0.0164377067953043,0.000783648753803687,
0.00950434172638755));
#53431=CARTESIAN_POINT('Ctrl Pts',(-0.0162860744225938,0.000820164345697787,
0.00958763303397418));
#53432=CARTESIAN_POINT('Ctrl Pts',(-0.016135172427679,0.000860204085166195,
0.00967070099051174));
#53433=CARTESIAN_POINT('Ctrl Pts',(-0.0159861906776217,0.00090600098099338,
0.0097528594815456));
#53434=CARTESIAN_POINT('Ctrl Pts',(-0.015911699802593,0.000928899428906973,
0.00979393872706254));
#53435=CARTESIAN_POINT('Ctrl Pts',(-0.0158376888222992,0.000953237109203088,
0.00983479027696665));
#53436=CARTESIAN_POINT('Ctrl Pts',(-0.0157637840768862,0.000980108361912485,
0.0098756285401895));
#53437=CARTESIAN_POINT('Ctrl Pts',(-0.0156898793314732,0.00100697961462188,
0.00991646680341235));
#53438=CARTESIAN_POINT('Ctrl Pts',(-0.0156160814995489,0.0010363844824535,
0.00995729312691053));
#53439=CARTESIAN_POINT('Ctrl Pts',(-0.0155451624184428,0.00106910118935474,
0.00999654935387522));
#53440=CARTESIAN_POINT('Ctrl Pts',(-0.0154742433373368,0.00110181789625599,
0.0100358055808399));
#53441=CARTESIAN_POINT('Ctrl Pts',(-0.0154062607310772,0.00113783598555345,
0.0100736076277172));
#53442=CARTESIAN_POINT('Ctrl Pts',(-0.0153367057996425,0.0011864783152364,
0.0101120703301702));
#53443=CARTESIAN_POINT('Ctrl Pts',(-0.0152671508682078,0.00123512064491935,
0.0101505330326231));
#53444=CARTESIAN_POINT('Ctrl Pts',(-0.0151962210891276,0.00129636052306388,
0.010190052413572));
#53445=CARTESIAN_POINT('Ctrl Pts',(-0.0151955011741265,0.00138726386004148,
0.010190435150715));
#53446=CARTESIAN_POINT('Ctrl Pts',(-0.0328029017533461,0.00420876907691088,
0.00416971954492692));
#53447=CARTESIAN_POINT('Ctrl Pts',(-0.0328178241773457,0.00455258395424896,
0.00451249633250882));
#53448=CARTESIAN_POINT('Ctrl Pts',(-0.032824617798705,0.00498124122173345,
0.00477032439575802));
#53449=CARTESIAN_POINT('Ctrl Pts',(-0.0328230352836128,0.00544566811076568,
0.00491342087848278));
#53450=CARTESIAN_POINT('Origin',(-0.034735005000479,0.00640255695754379,
0.00190578554004708));
#53451=CARTESIAN_POINT('Origin',(-0.0319546402921759,0.00870364387463654,
0.00212141796726865));
#53452=CARTESIAN_POINT('Ctrl Pts',(-0.0312397316818193,0.00944581611174232,
0.00513213161553135));
#53453=CARTESIAN_POINT('Ctrl Pts',(-0.0312427451291909,0.0099961712863933,
0.00499938556413842));
#53454=CARTESIAN_POINT('Ctrl Pts',(-0.0312280639560642,0.0105069403051091,
0.0047080293508316));
#53455=CARTESIAN_POINT('Ctrl Pts',(-0.0311964657406625,0.0109004375755286,
0.00430330249027805));
#53456=CARTESIAN_POINT('Ctrl Pts',(-0.0311915498707958,0.0109616556332477,
0.00424033739706811));
#53457=CARTESIAN_POINT('Ctrl Pts',(-0.0311862383752956,0.0110200907724982,
0.00417471052484215));
#53458=CARTESIAN_POINT('Ctrl Pts',(-0.0311805498203867,0.0110755139672511,
0.00410668511418156));
#53459=CARTESIAN_POINT('Ctrl Pts',(-0.0323289055074392,0.00956463425415454,
0.00496775823408284));
#53460=CARTESIAN_POINT('Ctrl Pts',(-0.0322835345259748,0.0105323987449126,
0.00469073673727539));
#53461=CARTESIAN_POINT('Ctrl Pts',(-0.0321832620259936,0.0111351594703581,
0.0038896157471382));
#53462=CARTESIAN_POINT('Ctrl Pts',(-0.0312200346161952,0.00937861982895493,
0.005143320519133));
#53463=CARTESIAN_POINT('Ctrl Pts',(-0.0312346609291161,0.010392145765573,
0.00491292268688717));
#53464=CARTESIAN_POINT('Ctrl Pts',(-0.0311666295055617,0.0110485670062122,
0.00411075495197673));
#53465=CARTESIAN_POINT('Ctrl Pts',(-0.0297913603172275,0.00936877543822054,
0.00533931757967592));
#53466=CARTESIAN_POINT('Ctrl Pts',(-0.0298729635552801,0.010373653877553,
0.00514091880759088));
#53467=CARTESIAN_POINT('Ctrl Pts',(-0.0298366841122876,0.0110548585358543,
0.00437421338280484));
#53468=CARTESIAN_POINT('Ctrl Pts',(-0.0282450431755874,0.00956902209544001,
0.00560006763975001));
#53469=CARTESIAN_POINT('Ctrl Pts',(-0.0283949818456436,0.0105482847054643,
0.00541290036078366));
#53470=CARTESIAN_POINT('Ctrl Pts',(-0.028395990827051,0.0112342387571675,
0.00467417110487153));
#53471=CARTESIAN_POINT('Ctrl Pts',(-0.0275655213410194,0.00968883811290509,
0.00572471869657096));
#53472=CARTESIAN_POINT('Ctrl Pts',(-0.0277376631422493,0.0106490933625841,
0.00554219914270759));
#53473=CARTESIAN_POINT('Ctrl Pts',(-0.0277512049297973,0.0113334753293838,
0.00482364841791884));
#53474=CARTESIAN_POINT('Ctrl Pts',(-0.0265559503873459,0.00990413801644446,
0.00591995560007617));
#53475=CARTESIAN_POINT('Ctrl Pts',(-0.0267967998478078,0.0108655812357791,
0.00572891428999259));
#53476=CARTESIAN_POINT('Ctrl Pts',(-0.0268463635570509,0.0115505484415826,
0.0049905610344629));
#53477=CARTESIAN_POINT('Ctrl Pts',(-0.0254134410921188,0.0102924262124582,
0.00616699453409525));
#53478=CARTESIAN_POINT('Ctrl Pts',(-0.0257285874563407,0.0112136516860456,
0.00595948028213227));
#53479=CARTESIAN_POINT('Ctrl Pts',(-0.0258174256338695,0.0118799491673231,
0.0052256231497365));
#53480=CARTESIAN_POINT('Ctrl Pts',(-0.0241333918107377,0.0108163472585975,
0.0065002849396036));
#53481=CARTESIAN_POINT('Ctrl Pts',(-0.0244436384112718,0.0117250628952979,
0.00629519856091718));
#53482=CARTESIAN_POINT('Ctrl Pts',(-0.0245157153622336,0.012395142022738,
0.00558085893470258));
#53483=CARTESIAN_POINT('Ctrl Pts',(-0.0228483409677525,0.0112659510356338,
0.00688891895195866));
#53484=CARTESIAN_POINT('Ctrl Pts',(-0.0230856742818988,0.0122441558971299,
0.00670982953098516));
#53485=CARTESIAN_POINT('Ctrl Pts',(-0.0230700961407223,0.0129638411427807,
0.00598451454320165));
#53486=CARTESIAN_POINT('Ctrl Pts',(-0.0212004840786695,0.0115773550466138,
0.00748986583980058));
#53487=CARTESIAN_POINT('Ctrl Pts',(-0.0213153046899869,0.0127481902765968,
0.0073719420427496));
#53488=CARTESIAN_POINT('Ctrl Pts',(-0.021136532193506,0.0135629220950769,
0.00653554204472973));
#53489=CARTESIAN_POINT('Ctrl Pts',(-0.019167042709017,0.0116660893942,0.0083356198639276));
#53490=CARTESIAN_POINT('Ctrl Pts',(-0.0191804598076967,0.0130869110402204,
0.00829326114742038));
#53491=CARTESIAN_POINT('Ctrl Pts',(-0.0187900587222371,0.0139677007175143,
0.00724790416315883));
#53492=CARTESIAN_POINT('Ctrl Pts',(-0.0174670465709295,0.0116196738300899,
0.00910191951123781));
#53493=CARTESIAN_POINT('Ctrl Pts',(-0.0174262819740025,0.0132365547392771,
0.00910993735381814));
#53494=CARTESIAN_POINT('Ctrl Pts',(-0.0168589854819659,0.0141212857391936,
0.00788011740047476));
#53495=CARTESIAN_POINT('Ctrl Pts',(-0.0158059579855905,0.0115214530689453,
0.00988765845793635));
#53496=CARTESIAN_POINT('Ctrl Pts',(-0.0157056048103155,0.0133294903173838,
0.00994296969637082));
#53497=CARTESIAN_POINT('Ctrl Pts',(-0.0149832859165724,0.0141820295951835,
0.00851735457057802));
#53498=CARTESIAN_POINT('Ctrl Pts',(-0.0148654266643081,0.0114297302076929,
0.010351940251372));
#53499=CARTESIAN_POINT('Ctrl Pts',(-0.0147095818741422,0.013367376733051,
0.0104450157835826));
#53500=CARTESIAN_POINT('Ctrl Pts',(-0.0138532836292959,0.0141734567758274,
0.0088943488081759));
#53501=CARTESIAN_POINT('Ctrl Pts',(-0.0141214309450543,0.0113497268442424,
0.010725020327289));
#53502=CARTESIAN_POINT('Ctrl Pts',(-0.013953871480134,0.0133905329094632,
0.0108226494532548));
#53503=CARTESIAN_POINT('Ctrl Pts',(-0.0130838251198689,0.0141473730896605,
0.00912716600625515));
#53504=CARTESIAN_POINT('',(-0.0177980642249198,0.0125583362975071,0.00878211032055315));
#53505=CARTESIAN_POINT('Ctrl Pts',(-0.0152016054147685,0.0114763663362328,
0.0101879079879127));
#53506=CARTESIAN_POINT('Ctrl Pts',(-0.0152050402282475,0.0115448524639896,
0.0101862046141003));
#53507=CARTESIAN_POINT('Ctrl Pts',(-0.015246578657923,0.0115988404990711,
0.01016347688237));
#53508=CARTESIAN_POINT('Ctrl Pts',(-0.0152916884420663,0.0116441867557964,
0.0101388600044451));
#53509=CARTESIAN_POINT('Ctrl Pts',(-0.0153367982262096,0.0116895330125218,
0.0101142431265201));
#53510=CARTESIAN_POINT('Ctrl Pts',(-0.01538541673375,0.0117262297566457,
0.0100876082435883));
#53511=CARTESIAN_POINT('Ctrl Pts',(-0.0154357715420465,0.0117599086203434,
0.0100600660888032));
#53512=CARTESIAN_POINT('Ctrl Pts',(-0.0155364811586393,0.0118272663477389,
0.0100049817792332));
#53513=CARTESIAN_POINT('Ctrl Pts',(-0.0156440742586175,0.0118825435032204,
0.0099461410209836));
#53514=CARTESIAN_POINT('Ctrl Pts',(-0.0157531598918773,0.0119329055094452,
0.00988663924228184));
#53515=CARTESIAN_POINT('Ctrl Pts',(-0.015857875517086,0.0119812499963496,
0.00982952112533473));
#53516=CARTESIAN_POINT('Ctrl Pts',(-0.0159639163376693,0.0120250494639677,
0.00977169149544583));
#53517=CARTESIAN_POINT('Ctrl Pts',(-0.0160709107474822,0.0120659590805672,
0.00971346327977728));
#53518=CARTESIAN_POINT('Ctrl Pts',(-0.0160753758541115,0.0120676663267738,
0.00971103329121761));
#53519=CARTESIAN_POINT('Ctrl Pts',(-0.0160798426028328,0.012069368537373,
0.00970860256749819));
#53520=CARTESIAN_POINT('Ctrl Pts',(-0.0160843109022008,0.0120710658302876,
0.00970617114887469));
#53521=CARTESIAN_POINT('Ctrl Pts',(-0.0161958501168776,0.012113434235619,
0.00964547724690497));
#53522=CARTESIAN_POINT('Ctrl Pts',(-0.0163083952064916,0.0121527396216367,
0.00958434693869943));
#53523=CARTESIAN_POINT('Ctrl Pts',(-0.0164214891938709,0.012189946046317,
0.00952302377047061));
#53524=CARTESIAN_POINT('Ctrl Pts',(-0.0166343834177911,0.0122599854276378,
0.00940758572985573));
#53525=CARTESIAN_POINT('Ctrl Pts',(-0.0168492373888548,0.0123225837024365,
0.00929147343309498));
#53526=CARTESIAN_POINT('Ctrl Pts',(-0.0170652210318034,0.0123803691306557,
0.00917518725110595));
#53527=CARTESIAN_POINT('Ctrl Pts',(-0.0170787076951882,0.0123839774252853,
0.00916792599478407));
#53528=CARTESIAN_POINT('Ctrl Pts',(-0.0170921988550825,0.0123875667820013,
0.00916066382123329));
#53529=CARTESIAN_POINT('Ctrl Pts',(-0.0171056945549107,0.0123911377037813,
0.0091534006632344));
#53530=CARTESIAN_POINT('Ctrl Pts',(-0.0173353186127975,0.0124518955422013,
0.00902982086863233));
#53531=CARTESIAN_POINT('Ctrl Pts',(-0.0175661531830874,0.0125073758986016,
0.00890601385220129));
#53532=CARTESIAN_POINT('Ctrl Pts',(-0.0177980683695447,0.0125583397025061,
0.0087821194794289));
#53533=CARTESIAN_POINT('',(-0.0197685317455456,0.0133197512836476,0.00744191810867941));
#53534=CARTESIAN_POINT('Ctrl Pts',(-0.0177980642249198,0.0125583362975071,
0.00878211032055315));
#53535=CARTESIAN_POINT('Ctrl Pts',(-0.0179830006717361,0.0125989757247538,
0.00868331054782076));
#53536=CARTESIAN_POINT('Ctrl Pts',(-0.0181668800802558,0.0126419851714326,
0.00858330934992592));
#53537=CARTESIAN_POINT('Ctrl Pts',(-0.0183486946939373,0.0126879577019625,
0.00848144524952353));
#53538=CARTESIAN_POINT('Ctrl Pts',(-0.0183653017055318,0.0126921568492812,
0.00847214094629841));
#53539=CARTESIAN_POINT('Ctrl Pts',(-0.0183818925050772,0.0126963819437408,
0.00846281999090755));
#53540=CARTESIAN_POINT('Ctrl Pts',(-0.0183984647163266,0.0127006332497774,
0.00845348258635921));
#53541=CARTESIAN_POINT('Ctrl Pts',(-0.0185633261223776,0.0127429255112143,
0.00836059349512425));
#53542=CARTESIAN_POINT('Ctrl Pts',(-0.0187263554908639,0.0127877966895147,
0.00826609507339865));
#53543=CARTESIAN_POINT('Ctrl Pts',(-0.0188865527000641,0.0128364005614957,
0.00816870025540869));
#53544=CARTESIAN_POINT('Ctrl Pts',(-0.0189126820926947,0.0128443282255337,
0.00815281441412496));
#53545=CARTESIAN_POINT('Ctrl Pts',(-0.0189387119608945,0.0128523658573526,
0.00813685671555506));
#53546=CARTESIAN_POINT('Ctrl Pts',(-0.0189646627927476,0.0128605170269426,
0.00812081022830822));
#53547=CARTESIAN_POINT('Ctrl Pts',(-0.0190262598499789,0.0128798646941995,
0.00808272218554736));
#53548=CARTESIAN_POINT('Ctrl Pts',(-0.0190874192852412,0.0128998465199453,
0.00804413453101425));
#53549=CARTESIAN_POINT('Ctrl Pts',(-0.0191478356195508,0.0129206632446099,
0.00800493934770974));
#53550=CARTESIAN_POINT('Ctrl Pts',(-0.0192337053473069,0.0129502500525509,
0.0079492312389976));
#53551=CARTESIAN_POINT('Ctrl Pts',(-0.0193182418693047,0.0129814734970053,
0.0078922852084602));
#53552=CARTESIAN_POINT('Ctrl Pts',(-0.0194019483291107,0.0130164329880073,
0.0078320587920224));
#53553=CARTESIAN_POINT('Ctrl Pts',(-0.0194269273356376,0.0130268653173155,
0.00781408651063836));
#53554=CARTESIAN_POINT('Ctrl Pts',(-0.0194515537016336,0.0130375426930232,
0.00779600101439142));
#53555=CARTESIAN_POINT('Ctrl Pts',(-0.019475745499314,0.0130484770573286,
0.00777781862192818));
#53556=CARTESIAN_POINT('Ctrl Pts',(-0.0195326221675865,0.0130741845396575,
0.00773507050051131));
#53557=CARTESIAN_POINT('Ctrl Pts',(-0.0195871070281101,0.0131012997696144,
0.00769179228940438));
#53558=CARTESIAN_POINT('Ctrl Pts',(-0.0196364499341613,0.0131318484117174,
0.00764734735079382));
#53559=CARTESIAN_POINT('Ctrl Pts',(-0.0196529910828398,0.0131420891873707,
0.00763244814042303));
#53560=CARTESIAN_POINT('Ctrl Pts',(-0.019668874008655,0.0131526812624034,
0.00761748454393024));
#53561=CARTESIAN_POINT('Ctrl Pts',(-0.0196847074254495,0.0131642647987755,
0.00760167899627938));
#53562=CARTESIAN_POINT('Ctrl Pts',(-0.0197025345823486,0.0131773069313128,
0.00758388321779995));
#53563=CARTESIAN_POINT('Ctrl Pts',(-0.0197204841177018,0.0131915916001444,
0.00756495057568836));
#53564=CARTESIAN_POINT('Ctrl Pts',(-0.0197365286335694,0.013208312962062,
0.00754479399121415));
#53565=CARTESIAN_POINT('Ctrl Pts',(-0.0197668232558055,0.0132398855783219,
0.00750673512317151));
#53566=CARTESIAN_POINT('Ctrl Pts',(-0.0197875780156799,0.0132754871342319,
0.00746915089349625));
#53567=CARTESIAN_POINT('Ctrl Pts',(-0.0197684666960677,0.0133196392804432,
0.00744178318769348));
#53568=CARTESIAN_POINT('Ctrl Pts',(-0.0197685329350908,0.0133197531415193,
0.00744192027110921));
#53569=CARTESIAN_POINT('Ctrl Pts',(-0.0202415101381015,0.0133224462394573,
0.00721107381044522));
#53570=CARTESIAN_POINT('Ctrl Pts',(-0.0207109595596229,0.0133260249537321,
0.00697296703985871));
#53571=CARTESIAN_POINT('Ctrl Pts',(-0.0211704028999606,0.0133306505564277,
0.00671687894543797));
#53572=CARTESIAN_POINT('Ctrl Pts',(-0.0213774769702589,0.0133327353453313,
0.00660145839319391));
#53573=CARTESIAN_POINT('Ctrl Pts',(-0.0215825720015505,0.0133348962657808,
0.0064823124554158));
#53574=CARTESIAN_POINT('Ctrl Pts',(-0.0217846042317191,0.0133372723154647,
0.0063580695368299));
#53575=CARTESIAN_POINT('Origin',(0.,0.0012,0.));
#53576=CARTESIAN_POINT('Origin',(0.00625,0.0012,-0.0110556546617557));
#53577=CARTESIAN_POINT('Origin',(-0.000371408500209017,0.0012,-0.0126945679613751));
#53578=CARTESIAN_POINT('Origin',(-0.000359710594690623,0.0012,-0.0122947390492059));
#53579=CARTESIAN_POINT('Origin',(-0.000359710594690623,0.0012,-0.0122947390492059));
#53580=CARTESIAN_POINT('Origin',(-0.000492372526715892,0.0012,-0.0126720993701079));
#53581=CARTESIAN_POINT('Origin',(-0.000359710594690623,0.013,-0.0122947390492059));
#53582=CARTESIAN_POINT('Origin',(-0.000359710594690623,0.0128,-0.0122947390492059));
#53583=CARTESIAN_POINT('Origin',(0.00396253460616978,0.0012,0.));
#53584=CARTESIAN_POINT('Ctrl Pts',(-0.00872901544041542,0.001,-0.00439918826870922));
#53585=CARTESIAN_POINT('Ctrl Pts',(-0.0087111501862006,0.000999999999999996,
-0.00439284638245222));
#53586=CARTESIAN_POINT('Ctrl Pts',(-0.00869279015334147,0.00100269294713495,
-0.00438918614424969));
#53587=CARTESIAN_POINT('Ctrl Pts',(-0.00865158834960436,0.00101409730914674,
-0.00438662535591686));
#53588=CARTESIAN_POINT('Ctrl Pts',(-0.00862973231641669,0.00102389408403334,
-0.00438921693392455));
#53589=CARTESIAN_POINT('Ctrl Pts',(-0.00858288340936395,0.00105172009043307,
-0.00440193254517403));
#53590=CARTESIAN_POINT('Ctrl Pts',(-0.00855789795273511,0.00107226428316071,
-0.00441469677569042));
#53591=CARTESIAN_POINT('Ctrl Pts',(-0.00850849314601994,0.00112697168989658,
-0.00445471537180711));
#53592=CARTESIAN_POINT('Ctrl Pts',(-0.00848731866338639,0.00116211739589943,
-0.00448414297043919));
#53593=CARTESIAN_POINT('Ctrl Pts',(-0.00847459052587701,0.00119866682631849,
-0.00451811498504207));
#53594=CARTESIAN_POINT('Ctrl Pts',(-0.00847436147598704,0.00119933341534008,
-0.00451873568775905));
#53595=CARTESIAN_POINT('Ctrl Pts',(-0.00847413551305999,0.0012,-0.00451935750764786));
#53596=CARTESIAN_POINT('Origin',(0.00396253460616978,0.0128,0.));
#53597=CARTESIAN_POINT('Origin',(-0.000359710594690623,0.0128,-0.0122947390492059));
#53598=CARTESIAN_POINT('Origin',(-0.00828616193994173,0.0128,-0.00445104985208033));
#53599=CARTESIAN_POINT('Origin',(-0.00866210908617835,0.0172426406871193,
-0.00458766516321543));
#53600=CARTESIAN_POINT('Origin',(-0.00866210908617835,0.0128,-0.00458766516321543));
#53601=CARTESIAN_POINT('Origin',(-0.00866210908617835,0.0128,-0.00458766516321543));
#53602=CARTESIAN_POINT('Origin',(-0.00880510120094866,0.0128,-0.00421409688951767));
#53603=CARTESIAN_POINT('Origin',(-0.00926982557395217,0.0128,-0.003));
#53604=CARTESIAN_POINT('Ctrl Pts',(-0.00918425288415917,0.0128,-0.00150244288430738));
#53605=CARTESIAN_POINT('Ctrl Pts',(-0.00918425288415917,0.0128170824847327,
-0.00150244288430738));
#53606=CARTESIAN_POINT('Ctrl Pts',(-0.00918178381291453,0.012833758703744,
-0.00150477127744238));
#53607=CARTESIAN_POINT('Ctrl Pts',(-0.00917185354020169,0.0128680675590347,
-0.00151419537016038));
#53608=CARTESIAN_POINT('Ctrl Pts',(-0.00916385928771597,0.0128847555751617,
-0.00152180700263329));
#53609=CARTESIAN_POINT('Ctrl Pts',(-0.00914084612141564,0.0129201248655613,
-0.00154396884133387));
#53610=CARTESIAN_POINT('Ctrl Pts',(-0.00912437900625805,0.0129369061311702,
-0.00156000826915972));
#53611=CARTESIAN_POINT('Ctrl Pts',(-0.00908494519633725,0.0129671782156686,
-0.00159920014865634));
#53612=CARTESIAN_POINT('Ctrl Pts',(-0.00906084370069278,0.0129790454674433,
-0.00162368238643171));
#53613=CARTESIAN_POINT('Ctrl Pts',(-0.00900991177359934,0.0129957386317182,
-0.00167693589417492));
#53614=CARTESIAN_POINT('Ctrl Pts',(-0.0089823266678177,0.0129997703556913,
-0.00170667450021843));
#53615=CARTESIAN_POINT('Ctrl Pts',(-0.00895480987854902,0.012999996823628,
-0.00173740215050066));
#53616=CARTESIAN_POINT('Ctrl Pts',(-0.00895403629968172,0.013,-0.00173826686170102));
#53617=CARTESIAN_POINT('Ctrl Pts',(-0.00895326315945257,0.013,-0.00173913195070767));
#53618=CARTESIAN_POINT('Origin',(0.00396253460616978,0.0128,0.));
#53619=CARTESIAN_POINT('Ctrl Pts',(-0.00918425288415917,0.0128,0.00150244288430739));
#53620=CARTESIAN_POINT('Ctrl Pts',(-0.00918425288415917,0.0128170859338975,
0.00150244288430739));
#53621=CARTESIAN_POINT('Ctrl Pts',(-0.00918178281693229,0.0128337653687318,
0.0015047722151673));
#53622=CARTESIAN_POINT('Ctrl Pts',(-0.00917184364876475,0.0128680979862759,
0.00151420476610174));
#53623=CARTESIAN_POINT('Ctrl Pts',(-0.00916383629565585,0.0128848026420203,
0.00152182891425387));
#53624=CARTESIAN_POINT('Ctrl Pts',(-0.00914076136990567,0.0129202386542352,
0.00154405078036908));
#53625=CARTESIAN_POINT('Ctrl Pts',(-0.00912423199790756,0.0129370521043853,
0.00156015189581716));
#53626=CARTESIAN_POINT('Ctrl Pts',(-0.00908485146689577,0.0129672080432688,
0.00159929645791205));
#53627=CARTESIAN_POINT('Ctrl Pts',(-0.00906089667755369,0.0129790067173995,
0.00162363067642026));
#53628=CARTESIAN_POINT('Ctrl Pts',(-0.00901006148627273,0.0129957136180202,
0.00167677521626035));
#53629=CARTESIAN_POINT('Ctrl Pts',(-0.00898242682592675,0.0129997643999604,
0.0017065640468175));
#53630=CARTESIAN_POINT('Ctrl Pts',(-0.00895484578996856,0.0129999966744636,
0.00173736200896392));
#53631=CARTESIAN_POINT('Ctrl Pts',(-0.00895405424500949,0.013,0.00173824678215373));
#53632=CARTESIAN_POINT('Ctrl Pts',(-0.00895326315945257,0.013,0.00173913195070767));
#53633=CARTESIAN_POINT('Origin',(-0.00926982557395217,0.0128,0.003));
#53634=CARTESIAN_POINT('Origin',(-0.00880510120094866,0.0128,0.00421409688951767));
#53635=CARTESIAN_POINT('Origin',(-0.00866210908617835,0.0128,0.00458766516321543));
#53636=CARTESIAN_POINT('Origin',(-0.00828616193994173,0.0128,0.00445104985208033));
#53637=CARTESIAN_POINT('Origin',(-0.00866210908617835,0.0128,0.00458766516321543));
#53638=CARTESIAN_POINT('Origin',(0.00396253460616978,0.0128,0.));
#53639=CARTESIAN_POINT('Origin',(-0.000358432971552437,0.0127995376138349,
0.0122885638920572));
#53640=CARTESIAN_POINT('Origin',(-0.00866210908617835,0.0172426406871193,
0.00458766516321543));
#53641=CARTESIAN_POINT('Ctrl Pts',(-0.00872901544041542,0.001,0.00439918826870923));
#53642=CARTESIAN_POINT('Ctrl Pts',(-0.00871115018620075,0.000999999999999995,
0.00439284638245227));
#53643=CARTESIAN_POINT('Ctrl Pts',(-0.00869279015334176,0.0010026929471349,
0.00438918614424975));
#53644=CARTESIAN_POINT('Ctrl Pts',(-0.00865158834960484,0.00101409730914656,
0.00438662535591684));
#53645=CARTESIAN_POINT('Ctrl Pts',(-0.0086297323164172,0.0010238940840331,
0.00438921693392447));
#53646=CARTESIAN_POINT('Ctrl Pts',(-0.0085828834093646,0.00105172009043261,
0.00440193254517378));
#53647=CARTESIAN_POINT('Ctrl Pts',(-0.00855789795273577,0.0010722642831601,
0.00441469677569001));
#53648=CARTESIAN_POINT('Ctrl Pts',(-0.00850849314601959,0.00112697168989682,
0.00445471537180723));
#53649=CARTESIAN_POINT('Ctrl Pts',(-0.00848731866338683,0.00116211739590194,
0.00448414297043797));
#53650=CARTESIAN_POINT('Ctrl Pts',(-0.008474590525877,0.00119866682631824,
0.00451811498504211));
#53651=CARTESIAN_POINT('Ctrl Pts',(-0.00847436147598702,0.00119933341534014,
0.00451873568775911));
#53652=CARTESIAN_POINT('Ctrl Pts',(-0.00847413551305999,0.0012,0.00451935750764786));
#53653=CARTESIAN_POINT('Origin',(-0.000359710594690623,-0.0267643850402721,
0.0122947390492058));
#53654=CARTESIAN_POINT('Origin',(-0.000359710594690623,0.0012,0.0122947390492058));
#53655=CARTESIAN_POINT('Origin',(0.00396253460616978,0.0012,0.));
#53656=CARTESIAN_POINT('Origin',(-0.000492372526715893,0.0012,0.0126720993701079));
#53657=CARTESIAN_POINT('Origin',(-0.000359710594690623,0.0012,0.0122947390492058));
#53658=CARTESIAN_POINT('Origin',(-0.000371408500209017,0.0012,0.0126945679613751));
#53659=CARTESIAN_POINT('Origin',(0.,0.0012,0.));
#53660=CARTESIAN_POINT('Origin',(0.00625,0.0012,0.0110556546617557));
#53661=CARTESIAN_POINT('Ctrl Pts',(-0.0217851806760967,0.0133379298455257,
0.00635852171619724));
#53662=CARTESIAN_POINT('Ctrl Pts',(-0.0217547869618247,0.0134,0.00630782040048327));
#53663=CARTESIAN_POINT('Ctrl Pts',(-0.0217107156962388,0.0134,0.00623430285898128));
#53664=CARTESIAN_POINT('Ctrl Pts',(-0.0211059273377224,0.0133284526427957,
0.00677623426358248));
#53665=CARTESIAN_POINT('Ctrl Pts',(-0.0210679711108307,0.0133999999999989,
0.00672870310400759));
#53666=CARTESIAN_POINT('Ctrl Pts',(-0.0210335277181246,0.0134,0.00664025400640994));
#53667=CARTESIAN_POINT('Ctrl Pts',(-0.0204008307143018,0.0133220811407593,
0.00713526585043071));
#53668=CARTESIAN_POINT('Ctrl Pts',(-0.0203697574984378,0.0134000000000006,
0.00708353647612649));
#53669=CARTESIAN_POINT('Ctrl Pts',(-0.0203298528305533,0.0134,0.00699354067580272));
#53670=CARTESIAN_POINT('Ctrl Pts',(-0.0196903594652534,0.0133183218342735,
0.0074805711203105));
#53671=CARTESIAN_POINT('Ctrl Pts',(-0.0196643483248125,0.0134,0.00742657395762507));
#53672=CARTESIAN_POINT('Ctrl Pts',(-0.0196203815614496,0.0134,0.00733530227811308));
#53673=CARTESIAN_POINT('Ctrl Pts',(-0.0196330752852868,0.0134,0.00732918600636585));
#53674=CARTESIAN_POINT('Ctrl Pts',(-0.0196818597813691,0.0134,0.00736910397047182));
#53675=CARTESIAN_POINT('Ctrl Pts',(-0.0197202603260748,0.0133753834465396,
0.00740233387196754));
#53676=CARTESIAN_POINT('Ctrl Pts',(-0.0197452145249671,0.0133494224881884,
0.00742268581627776));
#53677=CARTESIAN_POINT('Ctrl Pts',(-0.0197546009360699,0.0133396573889856,
0.00743034110975611));
#53678=CARTESIAN_POINT('Ctrl Pts',(-0.0197622739680707,0.0133295676857738,
0.00743656499904525));
#53679=CARTESIAN_POINT('Ctrl Pts',(-0.0197684494911197,0.013319646237248,
0.00744180675098383));
#53680=CARTESIAN_POINT('Origin',(-0.0217118521071243,0.0132000091012597,
0.00623362616163613));
#53681=CARTESIAN_POINT('Origin',(0.,0.0148,0.));
#53682=CARTESIAN_POINT('Origin',(-0.00829461958536103,0.0148,0.0140317242680344));
#53683=CARTESIAN_POINT('Origin',(-5.55111512312578E-20,0.0148,0.0163));
#53684=CARTESIAN_POINT('Origin',(0.000968491838391537,0.0132,0.0195074579675537));
#53685=CARTESIAN_POINT('',(-0.0196508596780355,0.0133196394337182,0.00750485043938584));
#53686=CARTESIAN_POINT('Ctrl Pts',(-0.0196330752852202,0.0133999065795009,
0.00732918623248855));
#53687=CARTESIAN_POINT('Ctrl Pts',(-0.01964049658091,0.0134002169462812,
0.00740499113020126));
#53688=CARTESIAN_POINT('Ctrl Pts',(-0.019646536705005,0.0133653010300346,
0.00746003419317941));
#53689=CARTESIAN_POINT('Ctrl Pts',(-0.0196493113876324,0.0133341571395498,
0.00749087942416069));
#53690=CARTESIAN_POINT('Ctrl Pts',(-0.0196497622599861,0.013329096409697,
0.00749589162330514));
#53691=CARTESIAN_POINT('Ctrl Pts',(-0.0196501721052253,0.0133240756827054,
0.007500349096231));
#53692=CARTESIAN_POINT('Ctrl Pts',(-0.0196505706684233,0.01331918635986,
0.00750430757167277));
#53693=CARTESIAN_POINT('Ctrl Pts',(-0.0196508596780355,0.0133196394337182,
0.00750485043938584));
#53694=CARTESIAN_POINT('Ctrl Pts',(-0.0196517301463747,0.0133094372306776,
0.00751318281902652));
#53695=CARTESIAN_POINT('Ctrl Pts',(-0.0196359506058628,0.0133103209938461,
0.00752127600829986));
#53696=CARTESIAN_POINT('Ctrl Pts',(-0.0196236297821887,0.0133096914985585,
0.00752903889497462));
#53697=CARTESIAN_POINT('Ctrl Pts',(-0.0196113089585145,0.0133090620032709,
0.00753680178164939));
#53698=CARTESIAN_POINT('Ctrl Pts',(-0.0196022669562798,0.0133066853648818,
0.00754393004283313));
#53699=CARTESIAN_POINT('Ctrl Pts',(-0.0195925258808658,0.0133048042394914,
0.00755103279544104));
#53700=CARTESIAN_POINT('Ctrl Pts',(-0.0195730437300377,0.0133010419887106,
0.00756523830065686));
#53701=CARTESIAN_POINT('Ctrl Pts',(-0.0195508365550145,0.0132993344156868,
0.00757946233409064));
#53702=CARTESIAN_POINT('Ctrl Pts',(-0.0195289992545459,0.013297538858661,
0.00759353629382882));
#53703=CARTESIAN_POINT('Ctrl Pts',(-0.0194853246536087,0.0132939477446093,
0.0076216842133052));
#53704=CARTESIAN_POINT('Ctrl Pts',(-0.0194430435141633,0.0132899297432538,
0.00764908629261058));
#53705=CARTESIAN_POINT('Ctrl Pts',(-0.0194001542186181,0.013286475558855,
0.00767636368086573));
#53706=CARTESIAN_POINT('Ctrl Pts',(-0.0193572649230729,0.0132830213744561,
0.00770364106912088));
#53707=CARTESIAN_POINT('Ctrl Pts',(-0.0193137841852262,0.013280139625784,
0.00773082204048671));
#53708=CARTESIAN_POINT('Ctrl Pts',(-0.019270341051663,0.0132773369080536,
0.00775786787866913));
#53709=CARTESIAN_POINT('Ctrl Pts',(-0.0192268979180997,0.0132745341903232,
0.00778491371685154));
#53710=CARTESIAN_POINT('Ctrl Pts',(-0.0191834870690465,0.013271808031535,
0.00781181542257173));
#53711=CARTESIAN_POINT('Ctrl Pts',(-0.0191399980595519,0.013269199341757,
0.00783864075413296));
#53712=CARTESIAN_POINT('Ctrl Pts',(-0.0190530200405629,0.013263981962201,
0.00789229141725542));
#53713=CARTESIAN_POINT('Ctrl Pts',(-0.0189657348924197,0.0132592362260527,
0.0079456459092374));
#53714=CARTESIAN_POINT('Ctrl Pts',(-0.0188783451923207,0.0132547235819708,
0.0079987961202624));
#53715=CARTESIAN_POINT('Ctrl Pts',(-0.0187909554922218,0.013250210937889,
0.0080519463312874));
#53716=CARTESIAN_POINT('Ctrl Pts',(-0.018703457929881,0.0132459303061245,
0.00810488666145772));
#53717=CARTESIAN_POINT('Ctrl Pts',(-0.0186158618349587,0.0132418368276672,
0.0081576848485452));
#53718=CARTESIAN_POINT('Ctrl Pts',(-0.018440669645114,0.0132336498707526,
0.00826328122272014));
#53719=CARTESIAN_POINT('Ctrl Pts',(-0.0182650877987147,0.013226212373642,
0.0083683165926902));
#53720=CARTESIAN_POINT('Ctrl Pts',(-0.0180892882551675,0.0132192925299878,
0.00847301660256035));
#53721=CARTESIAN_POINT('Ctrl Pts',(-0.0179134887116204,0.0132123726863335,
0.00857771661243049));
#53722=CARTESIAN_POINT('Ctrl Pts',(-0.0177374668317145,0.0132059702596472,
0.00868207341420632));
#53723=CARTESIAN_POINT('Ctrl Pts',(-0.0175612941370432,0.0131999999999863,
0.00878621496200948));
#53724=CARTESIAN_POINT('Origin',(-0.0170139362062251,0.0132,0.00887744578929155));
#53725=CARTESIAN_POINT('Origin',(-0.0315929984201515,0.0132338047728166,
0.000421641309267139));
#53726=CARTESIAN_POINT('Origin',(-0.0306447771669106,0.0131997021086423,
0.00097908882428757));
#53727=CARTESIAN_POINT('Origin',(0.0125,0.0148,0.0163));
#53728=CARTESIAN_POINT('Origin',(0.0125000000000002,0.0148,0.0163));
#53729=CARTESIAN_POINT('Origin',(0.000968491838391537,0.0148,0.0195074579675537));
#53730=CARTESIAN_POINT('Origin',(-0.0166089107357433,0.0148,0.00911686983553521));
#53731=CARTESIAN_POINT('Origin',(-0.0166089107357433,-0.0233872477181734,
0.00911686983553521));
#53732=CARTESIAN_POINT('Origin',(-0.0166089107357433,0.0136,0.00911686983553521));
#53733=CARTESIAN_POINT('Origin',(-0.0166089107357433,0.0148,0.00911686983553521));
#53734=CARTESIAN_POINT('Ctrl Pts',(-0.016701694953409,0.0136,0.00893969452982875));
#53735=CARTESIAN_POINT('Ctrl Pts',(-0.0170198255739522,0.0136,0.00910629506495907));
#53736=CARTESIAN_POINT('Ctrl Pts',(-0.0167106852091834,0.0136,0.00928903823146202));
#53737=CARTESIAN_POINT('Ctrl Pts',(-0.0167016949536332,0.0135476400133573,
0.00893969452994618));
#53738=CARTESIAN_POINT('Ctrl Pts',(-0.0170198255700888,0.013605866918945,
0.00910629506724286));
#53739=CARTESIAN_POINT('Ctrl Pts',(-0.0167106852095972,0.0134952800267145,
0.00928903823121737));
#53740=CARTESIAN_POINT('Ctrl Pts',(-0.0167693533640173,0.0134433372808467,
0.00892620607872109));
#53741=CARTESIAN_POINT('Ctrl Pts',(-0.0169535261534895,0.0135821048236451,
0.00914548686070417));
#53742=CARTESIAN_POINT('Ctrl Pts',(-0.0167984486911777,0.0132866745615678,
0.00923715831401753));
#53743=CARTESIAN_POINT('Ctrl Pts',(-0.0169321915143027,0.0134,0.00889374249599453));
#53744=CARTESIAN_POINT('Ctrl Pts',(-0.0170429823123482,0.0134296096361944,
0.0090926063455859));
#53745=CARTESIAN_POINT('Ctrl Pts',(-0.0170096750997843,0.0132000000002514,
0.00911229534833304));
#53746=CARTESIAN_POINT('Ctrl Pts',(-0.0170139362062252,0.0134,0.00887744578929154));
#53747=CARTESIAN_POINT('Ctrl Pts',(-0.0171157106796652,0.0134,0.00904961418521835));
#53748=CARTESIAN_POINT('Ctrl Pts',(-0.0171157106796652,0.0132,0.00904961418521835));
#53749=CARTESIAN_POINT('Origin',(-0.0170139362062251,0.0136,0.00887744578929155));
#53750=CARTESIAN_POINT('Origin',(-0.0300600678275123,0.0132000279471769,
2.05249395217151E-8));
#53751=CARTESIAN_POINT('Origin',(-0.0306415836854525,0.0132275415761495,
-0.000977259614057599));
#53752=CARTESIAN_POINT('Origin',(0.0125,0.0148,-4.59242549680257E-18));
#53753=CARTESIAN_POINT('Origin',(0.0125,0.0148,-0.0163));
#53754=CARTESIAN_POINT('Origin',(-0.0166089107357433,0.0148,0.00911686983553521));
#53755=CARTESIAN_POINT('Origin',(-0.0166089107357433,0.0148,0.00911686983553521));
#53756=CARTESIAN_POINT('Origin',(-0.0171126097916178,0.0136,0.0089291197592526));
#53757=CARTESIAN_POINT('Origin',(-0.00395280707079757,0.0136,0.00203751601562436));
#53758=CARTESIAN_POINT('Origin',(-0.031417620514871,0.0132317057944348,
-0.000523328499505522));
#53759=CARTESIAN_POINT('Origin',(-0.0218622149050354,0.0132000088155134,
-0.00614623259346473));
#53760=CARTESIAN_POINT('Origin',(-5.75539309396805E-17,0.0148,-0.0163));
#53761=CARTESIAN_POINT('Origin',(-5.5913058681838E-17,0.0148,-0.0163));
#53762=CARTESIAN_POINT('Origin',(-0.0169270413562866,0.0148,0.00928347037066553));
#53763=CARTESIAN_POINT('Origin',(-0.00376723863546634,0.0148,0.00239186662703728));
#53764=CARTESIAN_POINT('Origin',(-0.00501982557395217,0.0136,-2.16840434497101E-19));
#53765=CARTESIAN_POINT('Origin',(-0.00395280707079757,0.0136,-0.00203751601562436));
#53766=CARTESIAN_POINT('Ctrl Pts',(-0.0218610959359586,0.0134,-0.00614689907887383));
#53767=CARTESIAN_POINT('Ctrl Pts',(-0.0219044727354385,0.0134,-0.00621925440718493));
#53768=CARTESIAN_POINT('Ctrl Pts',(-0.0219347456955486,0.0133395813452038,
-0.00626975167747655));
#53769=CARTESIAN_POINT('Ctrl Pts',(-0.0211908357465453,0.0134,-0.00654871801303158));
#53770=CARTESIAN_POINT('Ctrl Pts',(-0.0212247955992385,0.0134,-0.00663581415013928));
#53771=CARTESIAN_POINT('Ctrl Pts',(-0.0212623782205978,0.0133302265401987,
-0.0066834625777092));
#53772=CARTESIAN_POINT('Ctrl Pts',(-0.0204946261712406,0.0134,-0.00689690575881084));
#53773=CARTESIAN_POINT('Ctrl Pts',(-0.020533789466998,0.0134000000000018,
-0.00698567815694382));
#53774=CARTESIAN_POINT('Ctrl Pts',(-0.0205647582082835,0.0133238888195004,
-0.00703748207612315));
#53775=CARTESIAN_POINT('Ctrl Pts',(-0.0197927551089427,0.0134,-0.00723339256190528));
#53776=CARTESIAN_POINT('Ctrl Pts',(-0.0198359543513604,0.0134,-0.00732350099258878));
#53777=CARTESIAN_POINT('Ctrl Pts',(-0.019861893665148,0.0133200915216836,
-0.00737760728537532));
#53778=CARTESIAN_POINT('Ctrl Pts',(-0.0199408118980957,0.0133213184223535,
-0.00733868056421511));
#53779=CARTESIAN_POINT('Ctrl Pts',(-0.019922092925456,0.0133504885578351,
-0.00732298807146352));
#53780=CARTESIAN_POINT('Ctrl Pts',(-0.0198891712274851,0.0133836292280226,
-0.00729672973567592));
#53781=CARTESIAN_POINT('Ctrl Pts',(-0.0198402998718966,0.01339574276528,
-0.00725610951526527));
#53782=CARTESIAN_POINT('Ctrl Pts',(-0.0198293072782953,0.0133984674531988,
-0.00724697284267681));
#53783=CARTESIAN_POINT('Ctrl Pts',(-0.019817587588659,0.0134,-0.00723727462473279));
#53784=CARTESIAN_POINT('Ctrl Pts',(-0.0198053128358601,0.0134,-0.00722737066271768));
#53785=CARTESIAN_POINT('Origin',(0.,0.0148,0.));
#53786=CARTESIAN_POINT('Origin',(-0.00829461958536102,0.0148,-0.0140317242680344));
#53787=CARTESIAN_POINT('Origin',(-0.00501982557395217,0.0148,-2.16840434497101E-19));
#53788=CARTESIAN_POINT('Origin',(-0.00376723863546634,0.0148,-0.00239186662703728));
#53789=CARTESIAN_POINT('Origin',(-0.0171126097916178,0.0136,-0.0089291197592526));
#53790=CARTESIAN_POINT('Origin',(-0.0170139362062251,0.0136,-0.00887744578929154));
#53791=CARTESIAN_POINT('Origin',(0.00096849183839154,0.0132,-0.0195074579675537));
#53792=CARTESIAN_POINT('',(-0.0198215803223295,0.013321303084244,-0.00740247338649423));
#53793=CARTESIAN_POINT('Ctrl Pts',(-0.0177200739051678,0.0132,-0.00869235495241354));
#53794=CARTESIAN_POINT('Ctrl Pts',(-0.0178972982560502,0.0132061003755682,
-0.00858759173559485));
#53795=CARTESIAN_POINT('Ctrl Pts',(-0.0180743645746548,0.0132126395146285,
-0.00848260398841626));
#53796=CARTESIAN_POINT('Ctrl Pts',(-0.0182511976186223,0.0132197008401163,
-0.00837726012578567));
#53797=CARTESIAN_POINT('Ctrl Pts',(-0.0184280306625898,0.0132267621656041,
-0.00827191626315508));
#53798=CARTESIAN_POINT('Ctrl Pts',(-0.0186046351512701,0.0132343459282969,
-0.00816622426863558));
#53799=CARTESIAN_POINT('Ctrl Pts',(-0.018780836856243,0.0132426797505751,
-0.00805995094578348));
#53800=CARTESIAN_POINT('Ctrl Pts',(-0.0188689377087295,0.0132468466617142,
-0.00800681428435743));
#53801=CARTESIAN_POINT('Ctrl Pts',(-0.0189569367254928,0.0132512008628788,
-0.0079535303626938));
#53802=CARTESIAN_POINT('Ctrl Pts',(-0.0190448205904563,0.0132557864815963,
-0.00790003202857749));
#53803=CARTESIAN_POINT('Ctrl Pts',(-0.0191327044554197,0.0132603721003139,
-0.00784653369446118));
#53804=CARTESIAN_POINT('Ctrl Pts',(-0.0192204765343328,0.0132651902745664,
-0.00779282664161546));
#53805=CARTESIAN_POINT('Ctrl Pts',(-0.0193079453907042,0.0132704778764169,
-0.0077388080222866));
#53806=CARTESIAN_POINT('Ctrl Pts',(-0.0193516798188899,0.0132731216773421,
-0.00771179871262217));
#53807=CARTESIAN_POINT('Ctrl Pts',(-0.019395337056506,0.0132758823759434,
-0.00768470916849096));
#53808=CARTESIAN_POINT('Ctrl Pts',(-0.0194390290153232,0.013278720806396,
-0.00765746961801436));
#53809=CARTESIAN_POINT('Ctrl Pts',(-0.0194827209741404,0.0132815592368486,
-0.00763023006753776));
#53810=CARTESIAN_POINT('Ctrl Pts',(-0.0195264529796914,0.013284477938968,
-0.00760284951973719));
#53811=CARTESIAN_POINT('Ctrl Pts',(-0.0195695851804412,0.013287962453304,
-0.00757537035271812));
#53812=CARTESIAN_POINT('Ctrl Pts',(-0.0196127173811911,0.0132914469676401,
-0.00754789118569905));
#53813=CARTESIAN_POINT('Ctrl Pts',(-0.0196552331874147,0.0132954885780045,
-0.00752028533519109));
#53814=CARTESIAN_POINT('Ctrl Pts',(-0.0196991269521685,0.0132991224730883,
-0.00749192947659815));
#53815=CARTESIAN_POINT('Ctrl Pts',(-0.0197210738345454,0.0133009394206302,
-0.00747775154730168));
#53816=CARTESIAN_POINT('Ctrl Pts',(-0.0197433866480824,0.0133026735298679,
-0.00746342238788288));
#53817=CARTESIAN_POINT('Ctrl Pts',(-0.0197629783330933,0.0133064335087228,
-0.00744909564974968));
#53818=CARTESIAN_POINT('Ctrl Pts',(-0.0197727741755988,0.0133083134981502,
-0.00744193228068309));
#53819=CARTESIAN_POINT('Ctrl Pts',(-0.0197818720451141,0.0133106815439565,
-0.00743473958991742));
#53820=CARTESIAN_POINT('Ctrl Pts',(-0.0197942328454585,0.0133113429113141,
-0.00742691782953974));
#53821=CARTESIAN_POINT('Ctrl Pts',(-0.0198065936458028,0.0133120042786716,
-0.00741909606916207));
#53822=CARTESIAN_POINT('Ctrl Pts',(-0.0198223960209913,0.0133111962794624,
-0.00741094744514287));
#53823=CARTESIAN_POINT('Ctrl Pts',(-0.0198215803223295,0.013321303084244,
-0.00740247338649423));
#53824=CARTESIAN_POINT('Ctrl Pts',(-0.0198213244982509,0.0133208884971597,
-0.00740199237898985));
#53825=CARTESIAN_POINT('Ctrl Pts',(-0.0198186243540202,0.0133553313782365,
-0.00737322845529448));
#53826=CARTESIAN_POINT('Ctrl Pts',(-0.0198153027363176,0.0133810561537279,
-0.0073370106567662));
#53827=CARTESIAN_POINT('Ctrl Pts',(-0.0198101938602386,0.0133939472752386,
-0.0072809710310928));
#53828=CARTESIAN_POINT('Ctrl Pts',(-0.0198087235859192,0.0133976571880671,
-0.00726484348733972));
#53829=CARTESIAN_POINT('Ctrl Pts',(-0.0198070715857852,0.0134000059680804,
-0.00724701116723406));
#53830=CARTESIAN_POINT('Ctrl Pts',(-0.0198053126720851,0.0133999709244785,
-0.00722737055260438));
#53831=CARTESIAN_POINT('Origin',(-0.0170139362062251,0.0132,-0.00887744578929154));
#53832=CARTESIAN_POINT('Origin',(0.00096849183839154,0.0148,-0.0195074579675537));
#53833=CARTESIAN_POINT('Origin',(-0.0166089107357434,0.0148,-0.00911686983553521));
#53834=CARTESIAN_POINT('Origin',(-0.0169270413562866,0.0148,-0.00928347037066553));
#53835=CARTESIAN_POINT('Origin',(-0.0166089107357433,0.0148,-0.0091168698355352));
#53836=CARTESIAN_POINT('Ctrl Pts',(-0.0170139362062251,0.0134,-0.00887744578929154));
#53837=CARTESIAN_POINT('Ctrl Pts',(-0.0171157106796652,0.0134,-0.00904961418521834));
#53838=CARTESIAN_POINT('Ctrl Pts',(-0.0171157106796652,0.0132,-0.00904961418521834));
#53839=CARTESIAN_POINT('Ctrl Pts',(-0.0169321915143036,0.0134,-0.00889374249599441));
#53840=CARTESIAN_POINT('Ctrl Pts',(-0.017042982312349,0.0134296096361945,
-0.00909260634558574));
#53841=CARTESIAN_POINT('Ctrl Pts',(-0.0170096750997843,0.0132000000002514,
-0.00911229534833303));
#53842=CARTESIAN_POINT('Ctrl Pts',(-0.0167693533640169,0.0134433372808467,
-0.00892620607872114));
#53843=CARTESIAN_POINT('Ctrl Pts',(-0.0169535261534889,0.0135821048236453,
-0.00914548686070429));
#53844=CARTESIAN_POINT('Ctrl Pts',(-0.0167984486911777,0.0132866745615676,
-0.00923715831401752));
#53845=CARTESIAN_POINT('Ctrl Pts',(-0.0167016949536332,0.0135476400133573,
-0.00893969452994617));
#53846=CARTESIAN_POINT('Ctrl Pts',(-0.0170198255700888,0.0136058669189446,
-0.00910629506724285));
#53847=CARTESIAN_POINT('Ctrl Pts',(-0.0167106852095972,0.0134952800267149,
-0.00928903823121736));
#53848=CARTESIAN_POINT('Ctrl Pts',(-0.016701694953409,0.0136,-0.00893969452982874));
#53849=CARTESIAN_POINT('Ctrl Pts',(-0.0170198255739522,0.0136,-0.00910629506495906));
#53850=CARTESIAN_POINT('Ctrl Pts',(-0.0167106852091834,0.0136,-0.00928903823146201));
#53851=CARTESIAN_POINT('Origin',(-0.0166089107357433,0.0136,-0.0091168698355352));
#53852=CARTESIAN_POINT('Origin',(-0.0166089107357433,0.0148,-0.00911686983553521));
#53853=CARTESIAN_POINT('Origin',(-0.0166089107357433,0.0148,-0.00911686983553521));
#53854=CARTESIAN_POINT('Origin',(-0.0166089107357433,0.015,-0.00911686983553521));
#53855=CARTESIAN_POINT('Origin',(0.0125,0.0132,-4.59242549680257E-18));
#53856=CARTESIAN_POINT('Origin',(0.0125,0.0132,-4.59242549680257E-18));
#53857=CARTESIAN_POINT('Origin',(0.0125,0.0132,-0.0123));
#53858=CARTESIAN_POINT('Origin',(0.0125,0.0136,-4.59242549680257E-18));
#53859=CARTESIAN_POINT('Origin',(0.0125,0.0136,-0.0092));
#53860=CARTESIAN_POINT('Ctrl Pts',(-0.0206729454446971,0.,0.00682621009066018));
#53861=CARTESIAN_POINT('Ctrl Pts',(-0.0207261905924628,0.,0.00691508186067457));
#53862=CARTESIAN_POINT('Ctrl Pts',(-0.0207569064148775,8.46248955869717E-5,
0.00696634980939847));
#53863=CARTESIAN_POINT('Ctrl Pts',(-0.0199012495314622,0.,0.00728855107959443));
#53864=CARTESIAN_POINT('Ctrl Pts',(-0.0199411001596944,3.10281366133179E-17,
0.00739573685041475));
#53865=CARTESIAN_POINT('Ctrl Pts',(-0.0199830342135227,9.5792117705873E-5,
0.00743918849379106));
#53866=CARTESIAN_POINT('Ctrl Pts',(-0.0191043571886283,0.,0.00770407151128956));
#53867=CARTESIAN_POINT('Ctrl Pts',(-0.0191527383496395,-4.83326594045924E-17,
0.00781167719406153));
#53868=CARTESIAN_POINT('Ctrl Pts',(-0.0191854693058945,0.000103035383687346,
0.00785914556601559));
#53869=CARTESIAN_POINT('Ctrl Pts',(-0.0183042279408874,0.,0.0081135770554014));
#53870=CARTESIAN_POINT('Ctrl Pts',(-0.0183595141901171,1.35525271560688E-20,
0.00822160036715122));
#53871=CARTESIAN_POINT('Ctrl Pts',(-0.0183850475118973,0.000107632287825602,
0.00827148969799038));
#53872=CARTESIAN_POINT('Ctrl Pts',(-0.018451268973799,0.000107232892182658,
0.00823734560780459));
#53873=CARTESIAN_POINT('Ctrl Pts',(-0.01843973701703,7.76784087736853E-5,
0.0082258681813287));
#53874=CARTESIAN_POINT('Ctrl Pts',(-0.018417431856287,4.69122920424372E-5,
0.00820537292668292));
#53875=CARTESIAN_POINT('Ctrl Pts',(-0.0183963224542028,2.89310499208856E-5,
0.0081828289210615));
#53876=CARTESIAN_POINT('Ctrl Pts',(-0.0183752130521186,1.09498077993341E-5,
0.00816028491544008));
#53877=CARTESIAN_POINT('Ctrl Pts',(-0.0183568899610538,-3.23379581101954E-19,
0.00813879781574077));
#53878=CARTESIAN_POINT('Ctrl Pts',(-0.0183185440104958,0.,0.00810624927208572));
#53879=CARTESIAN_POINT('Origin',(-0.0206729454446971,0.0002,0.0068262100906602));
#53880=CARTESIAN_POINT('Origin',(-0.00829461958536102,0.0002,0.0140317242680344));
#53881=CARTESIAN_POINT('',(-0.0183580519175386,0.000107246172780706,0.00828872892562513));
#53882=CARTESIAN_POINT('Ctrl Pts',(-0.0167335787825944,0.0002,0.0092755050776766));
#53883=CARTESIAN_POINT('Ctrl Pts',(-0.016870203120021,0.00019553998556168,
0.00919474188112224));
#53884=CARTESIAN_POINT('Ctrl Pts',(-0.017006750934428,0.000190796366481944,
0.00911385415689994));
#53885=CARTESIAN_POINT('Ctrl Pts',(-0.0171431642092931,0.000185672027589209,
0.00903278828563277));
#53886=CARTESIAN_POINT('Ctrl Pts',(-0.0171601411622557,0.000185034291559247,
0.00902269944725));
#53887=CARTESIAN_POINT('Ctrl Pts',(-0.0171771158819337,0.000184390696478422,
0.00901260792396832));
#53888=CARTESIAN_POINT('Ctrl Pts',(-0.017194088540261,0.000183741048692459,
0.00900251343072304));
#53889=CARTESIAN_POINT('Ctrl Pts',(-0.0173134946485287,0.000179170644200067,
0.00893149661472916));
#53890=CARTESIAN_POINT('Ctrl Pts',(-0.0174328055967938,0.000174302961947506,
0.00886033035739381));
#53891=CARTESIAN_POINT('Ctrl Pts',(-0.0175519749817655,0.000168986864193267,
0.00878891407725371));
#53892=CARTESIAN_POINT('Ctrl Pts',(-0.0175826051732513,0.00016762046381948,
0.00877055790014992));
#53893=CARTESIAN_POINT('Ctrl Pts',(-0.0176132055874596,0.000166226880574114,
0.00875219768570016));
#53894=CARTESIAN_POINT('Ctrl Pts',(-0.0176438103849298,0.000164798089442301,
0.00873380982018834));
#53895=CARTESIAN_POINT('Ctrl Pts',(-0.0176812033644573,0.000163052390664412,
0.00871134350328783));
#53896=CARTESIAN_POINT('Ctrl Pts',(-0.0177186037909279,0.000161254130880076,
0.00868883543588592));
#53897=CARTESIAN_POINT('Ctrl Pts',(-0.0177559384513345,0.000159383309477981,
0.00866631559980144));
#53898=CARTESIAN_POINT('Ctrl Pts',(-0.017823830177126,0.000155981288614457,
0.00862536409469426));
#53899=CARTESIAN_POINT('Ctrl Pts',(-0.017891627135883,0.000152374921470389,
0.00858431261540693));
#53900=CARTESIAN_POINT('Ctrl Pts',(-0.017959730776856,0.000148368781047435,
0.00854280759069639));
#53901=CARTESIAN_POINT('Ctrl Pts',(-0.0179937825973424,0.000146365710835958,
0.00852205507834112));
#53902=CARTESIAN_POINT('Ctrl Pts',(-0.0180276481757308,0.000144276554852942,
0.00850134808399079));
#53903=CARTESIAN_POINT('Ctrl Pts',(-0.0180610836837602,0.000142090071389666,
0.00848081907584841));
#53904=CARTESIAN_POINT('Ctrl Pts',(-0.0180641279310168,0.000141890995716018,
0.00847894994388656));
#53905=CARTESIAN_POINT('Ctrl Pts',(-0.0180671802477625,0.000141690388311206,
0.00847707515616403));
#53906=CARTESIAN_POINT('Ctrl Pts',(-0.0180702400274756,0.000141488245959845,
0.00847519505648417));
#53907=CARTESIAN_POINT('Ctrl Pts',(-0.0181007863515196,0.000139470222982215,
0.00845642568762774));
#53908=CARTESIAN_POINT('Ctrl Pts',(-0.0181320898039847,0.000137301614487281,
0.00843712071736009));
#53909=CARTESIAN_POINT('Ctrl Pts',(-0.0181631255264992,0.0001348977973457,
0.00841781421912194));
#53910=CARTESIAN_POINT('Ctrl Pts',(-0.0181951710770037,0.000132415765758458,
0.00839787953372627));
#53911=CARTESIAN_POINT('Ctrl Pts',(-0.0182269603831239,0.000129687237058521,
0.0083779292554878));
#53912=CARTESIAN_POINT('Ctrl Pts',(-0.018257910967522,0.000126502915985151,
0.00835816520630279));
#53913=CARTESIAN_POINT('Ctrl Pts',(-0.0182764271408461,0.000124597897321993,
0.00834634137268504));
#53914=CARTESIAN_POINT('Ctrl Pts',(-0.0182955815663513,0.000122537179335476,
0.00833401545302579));
#53915=CARTESIAN_POINT('Ctrl Pts',(-0.0183155463531549,0.000121053263352702,
0.00832148692383736));
#53916=CARTESIAN_POINT('Ctrl Pts',(-0.0183280943035645,0.000120120616069915,
0.00831361269184541));
#53917=CARTESIAN_POINT('Ctrl Pts',(-0.0183424285341103,0.000119559534132814,
0.00830491130196657));
#53918=CARTESIAN_POINT('Ctrl Pts',(-0.018352680267871,0.000117343276337867,
0.00829769431201892));
#53919=CARTESIAN_POINT('Ctrl Pts',(-0.0183569540028375,0.000116419364475319,
0.0082946856987431));
#53920=CARTESIAN_POINT('Ctrl Pts',(-0.0183619411006891,0.00011063305116798,
0.00828848899624926));
#53921=CARTESIAN_POINT('Ctrl Pts',(-0.0183580519175386,0.000107246172780706,
0.00828872892562513));
#53922=CARTESIAN_POINT('Ctrl Pts',(-0.0183580389868516,0.000107244345009705,
0.00828873553226112));
#53923=CARTESIAN_POINT('Ctrl Pts',(-0.0183545804956432,7.77877261786513E-5,
0.00827286717337471));
#53924=CARTESIAN_POINT('Ctrl Pts',(-0.0183484379957968,4.67935037000903E-5,
0.00824319447998794));
#53925=CARTESIAN_POINT('Ctrl Pts',(-0.0183415805299276,2.89354452288591E-5,
0.0082130004877248));
#53926=CARTESIAN_POINT('Ctrl Pts',(-0.0183347229526445,1.10770966161947E-5,
0.00818280600489723));
#53927=CARTESIAN_POINT('Ctrl Pts',(-0.0183291093400749,4.59203235844747E-11,
0.00815540410168465));
#53928=CARTESIAN_POINT('Ctrl Pts',(-0.0183185438351041,2.1987620058006E-16,
0.00810624911031649));
#53929=CARTESIAN_POINT('Origin',(-0.00829461958536103,0.0002,0.0140317242680344));
#53930=CARTESIAN_POINT('Ctrl Pts',(-0.0309032482137635,5.85734536233529E-23,
0.000785457753406084));
#53931=CARTESIAN_POINT('Ctrl Pts',(-0.0309559999151988,-1.50815768680036E-17,
0.000872145039779753));
#53932=CARTESIAN_POINT('Ctrl Pts',(-0.0309844293408926,8.18824655704908E-5,
0.000924893432060964));
#53933=CARTESIAN_POINT('Ctrl Pts',(-0.029149510808606,-7.4625993722284E-22,
0.00180911851837678));
#53934=CARTESIAN_POINT('Ctrl Pts',(-0.0291437117667778,1.04850129722553E-16,
0.00194412775273983));
#53935=CARTESIAN_POINT('Ctrl Pts',(-0.0292400312363699,9.70131778003069E-5,
0.00195671427143983));
#53936=CARTESIAN_POINT('Ctrl Pts',(-0.025627466945566,1.50079397457481E-20,
0.00383185361080478));
#53937=CARTESIAN_POINT('Ctrl Pts',(-0.0256979250879764,-3.97855078320796E-16,
0.00398301591764444));
#53938=CARTESIAN_POINT('Ctrl Pts',(-0.0257319678794474,0.000164701302145256,
0.00400469466052874));
#53939=CARTESIAN_POINT('Ctrl Pts',(-0.0221555720892475,-2.92696195542735E-20,
0.00593921914836097));
#53940=CARTESIAN_POINT('Ctrl Pts',(-0.0222772613022354,5.99710111691989E-16,
0.00600319472741784));
#53941=CARTESIAN_POINT('Ctrl Pts',(-0.0222424088775952,0.000101917892232826,
0.00609197690023176));
#53942=CARTESIAN_POINT('Ctrl Pts',(-0.0204130553218997,-2.6933217319899E-20,
0.00698181563372554));
#53943=CARTESIAN_POINT('Ctrl Pts',(-0.0204657712517479,-9.3070861245427E-17,
0.00707344620791871));
#53944=CARTESIAN_POINT('Ctrl Pts',(-0.0204980517498235,8.73388957981665E-5,
0.00712348788289622));
#53945=CARTESIAN_POINT('Origin',(-0.030641586298985,0.000200000000000081,
0.00093807325632101));
#53946=CARTESIAN_POINT('Origin',(0.,0.0002,0.));
#53947=CARTESIAN_POINT('Origin',(0.,0.0002,0.0163));
#53948=CARTESIAN_POINT('Origin',(-0.0300842090696186,0.000199852455921088,
8.94993350727811E-8));
#53949=CARTESIAN_POINT('Origin',(-0.0306415078682799,0.000199999999999959,
-0.000938136151693087));
#53950=CARTESIAN_POINT('Origin',(1.72772815121504E-16,0.0002,0.0163));
#53951=CARTESIAN_POINT('Origin',(0.0125000000000002,0.0002,0.0163));
#53952=CARTESIAN_POINT('Ctrl Pts',(-0.0317225298040676,7.50059049772727E-5,
-0.000485888810412572));
#53953=CARTESIAN_POINT('Ctrl Pts',(-0.0317230373664694,9.08601866987305E-17,
-0.000416899367108417));
#53954=CARTESIAN_POINT('Ctrl Pts',(-0.0316451978945082,3.68628738645122E-21,
-0.000351300671161231));
#53955=CARTESIAN_POINT('Ctrl Pts',(-0.0297282606927244,8.49471121739984E-5,
-0.0016703560700287));
#53956=CARTESIAN_POINT('Ctrl Pts',(-0.0295579817604276,-1.51798941380492E-16,
-0.00169727441023402));
#53957=CARTESIAN_POINT('Ctrl Pts',(-0.0296397149165271,-1.19262238973414E-20,
-0.001528175376318));
#53958=CARTESIAN_POINT('Ctrl Pts',(-0.0257089904949931,0.00017109120157702,
-0.00401385795055467));
#53959=CARTESIAN_POINT('Ctrl Pts',(-0.0256722463681587,1.57875331656574E-16,
-0.0039952472777838));
#53960=CARTESIAN_POINT('Ctrl Pts',(-0.0256027281016292,6.6136332521626E-20,
-0.00383798124397724));
#53961=CARTESIAN_POINT('Ctrl Pts',(-0.0217137335921404,9.01571409957985E-5,
-0.00640668094362288));
#53962=CARTESIAN_POINT('Ctrl Pts',(-0.0218192026594173,-1.19741391585379E-16,
-0.0062719224035291));
#53963=CARTESIAN_POINT('Ctrl Pts',(-0.0216309143172447,-1.19262238973602E-20,
-0.00625785011357261));
#53964=CARTESIAN_POINT('Ctrl Pts',(-0.0197159421381394,8.02117903232503E-5,
-0.007583667403771));
#53965=CARTESIAN_POINT('Ctrl Pts',(-0.019655679728747,6.9889437387932E-17,
-0.00755045068836614));
#53966=CARTESIAN_POINT('Ctrl Pts',(-0.0196329910336286,3.68628738646249E-21,
-0.00744749148838045));
#53967=CARTESIAN_POINT('Origin',(-0.0206310823726759,0.0002,-0.00685120104972884));
#53968=CARTESIAN_POINT('Origin',(0.0125,0.0002,-4.59242549680257E-18));
#53969=CARTESIAN_POINT('Origin',(0.0125,0.0002,-0.0163));
#53970=CARTESIAN_POINT('Ctrl Pts',(-0.0207149455884366,8.43554830515145E-5,
-0.00699117714319487));
#53971=CARTESIAN_POINT('Ctrl Pts',(-0.0206842201344661,2.71050543121376E-20,
-0.00693989328795921));
#53972=CARTESIAN_POINT('Ctrl Pts',(-0.0206310823726745,0.,-0.00685120104972968));
#53973=CARTESIAN_POINT('Ctrl Pts',(-0.0199409189296865,9.54844683703659E-5,
-0.00746411055047154));
#53974=CARTESIAN_POINT('Ctrl Pts',(-0.0198990171876475,-1.98578856459192E-16,
-0.00742058444715366));
#53975=CARTESIAN_POINT('Ctrl Pts',(-0.0198592188402909,0.,-0.00731364399254252));
#53976=CARTESIAN_POINT('Ctrl Pts',(-0.0191437777603039,0.000102714870596185,
-0.00788384498404907));
#53977=CARTESIAN_POINT('Ctrl Pts',(-0.0191110107219842,-9.66541334231093E-17,
-0.00783631487172919));
#53978=CARTESIAN_POINT('Ctrl Pts',(-0.0190627669411057,0.,-0.00772891778103133));
#53979=CARTESIAN_POINT('Ctrl Pts',(-0.0183437447309265,0.000107326685769658,
-0.00829571182140303));
#53980=CARTESIAN_POINT('Ctrl Pts',(-0.018318191433809,-2.71050543121376E-20,
-0.00824574709711051));
#53981=CARTESIAN_POINT('Ctrl Pts',(-0.0182630443888809,0.,-0.00813791729797689));
#53982=CARTESIAN_POINT('Ctrl Pts',(-0.0182773531951025,0.,-0.00813059853245909));
#53983=CARTESIAN_POINT('Ctrl Pts',(-0.0183237401938969,-8.98673656062578E-19,
-0.00817597996129781));
#53984=CARTESIAN_POINT('Ctrl Pts',(-0.0183607091081757,2.90441480504016E-5,
-0.00821410741789105));
#53985=CARTESIAN_POINT('Ctrl Pts',(-0.0183837110698202,5.95874444262312E-5,
-0.00823616086343279));
#53986=CARTESIAN_POINT('Ctrl Pts',(-0.0183954716764099,7.52038382876884E-5,
-0.00824743650596148));
#53987=CARTESIAN_POINT('Ctrl Pts',(-0.0184040580625986,9.13930728185299E-5,
-0.00825544127361943));
#53988=CARTESIAN_POINT('Ctrl Pts',(-0.0184101483244441,0.000106933920730451,
-0.00826150146239095));
#53989=CARTESIAN_POINT('Origin',(0.0125,0.0002,-0.0163));
#53990=CARTESIAN_POINT('Origin',(-5.65435973303839E-17,0.0002,-0.0163));
#53991=CARTESIAN_POINT('Origin',(-0.00829461958536102,0.0002,-0.0140317242680344));
#53992=CARTESIAN_POINT('',(-0.0183165728615313,0.000106937857928121,-0.00831306077174831));
#53993=CARTESIAN_POINT('Ctrl Pts',(-0.0182773531237792,7.17402004746925E-8,
-0.00813059857217221));
#53994=CARTESIAN_POINT('Ctrl Pts',(-0.0182932596990271,-1.52680597115539E-7,
-0.00820516392882934));
#53995=CARTESIAN_POINT('Ctrl Pts',(-0.0183058695106016,3.83262775878502E-5,
-0.00826053175246635));
#53996=CARTESIAN_POINT('Ctrl Pts',(-0.0183119352413553,7.48753524682983E-5,
-0.00829084006900245));
#53997=CARTESIAN_POINT('Ctrl Pts',(-0.0183137536871268,8.58324017288368E-5,
-0.00829992620095999));
#53998=CARTESIAN_POINT('Ctrl Pts',(-0.01831515966709,9.67863519129567E-5,
-0.00830707883474611));
#53999=CARTESIAN_POINT('Ctrl Pts',(-0.0183163613629249,0.000107167142621255,
-0.00831267637528232));
#54000=CARTESIAN_POINT('Ctrl Pts',(-0.0183165728615313,0.000106937857928121,
-0.00831306077174831));
#54001=CARTESIAN_POINT('Ctrl Pts',(-0.0183176231313522,0.000115898484335213,
-0.00831791187551959));
#54002=CARTESIAN_POINT('Ctrl Pts',(-0.0183111189228912,0.000119376381868073,
-0.00832325866390957));
#54003=CARTESIAN_POINT('Ctrl Pts',(-0.0183019709395841,0.000120385225192318,
-0.00832917488410512));
#54004=CARTESIAN_POINT('Ctrl Pts',(-0.018292822956277,0.000121394068516563,
-0.00833509110430068));
#54005=CARTESIAN_POINT('Ctrl Pts',(-0.0182809403413241,0.000120021160600134,
-0.00834142305696103));
#54006=CARTESIAN_POINT('Ctrl Pts',(-0.0182706958539365,0.000119737357772785,
-0.00834733446742616));
#54007=CARTESIAN_POINT('Ctrl Pts',(-0.0182502068791613,0.000119169752118088,
-0.00835915728835641));
#54008=CARTESIAN_POINT('Ctrl Pts',(-0.018236279580929,0.000122970334818699,
-0.00836931344679148));
#54009=CARTESIAN_POINT('Ctrl Pts',(-0.0182210301194234,0.000125744392548628,
-0.00837961645538245));
#54010=CARTESIAN_POINT('Ctrl Pts',(-0.018190531196412,0.000131292508008485,
-0.0084002224725644));
#54011=CARTESIAN_POINT('Ctrl Pts',(-0.0181549294123503,0.000132620974976354,
-0.00842173018841584));
#54012=CARTESIAN_POINT('Ctrl Pts',(-0.0181205693182617,0.000134659993822246,
-0.00844286034392449));
#54013=CARTESIAN_POINT('Ctrl Pts',(-0.0180862092241731,0.000136699012668137,
-0.00846399049943315));
#54014=CARTESIAN_POINT('Ctrl Pts',(-0.0180530376061649,0.00013947305191,
-0.00848465307447684));
#54015=CARTESIAN_POINT('Ctrl Pts',(-0.0180194763349309,0.000141851554879295,
-0.00850533184841774));
#54016=CARTESIAN_POINT('Ctrl Pts',(-0.0179859150636969,0.00014423005784859,
-0.00852601062235864));
#54017=CARTESIAN_POINT('Ctrl Pts',(-0.0179519742820119,0.000146210446335367,
-0.00854672275338189));
#54018=CARTESIAN_POINT('Ctrl Pts',(-0.0179180631172835,0.000148146545055578,
-0.0085673725291748));
#54019=CARTESIAN_POINT('Ctrl Pts',(-0.0178502407878267,0.000152018742496001,
-0.00860867208076062));
#54020=CARTESIAN_POINT('Ctrl Pts',(-0.0177825274511162,0.00015571476862617,
-0.00864970618275563));
#54021=CARTESIAN_POINT('Ctrl Pts',(-0.0177146741348683,0.000159152003925665,
-0.00869064960328432));
#54022=CARTESIAN_POINT('Ctrl Pts',(-0.0176468208186205,0.000162589239225159,
-0.00873159302381301));
#54023=CARTESIAN_POINT('Ctrl Pts',(-0.0175788293634593,0.000165768310811214,
-0.00877244887659585));
#54024=CARTESIAN_POINT('Ctrl Pts',(-0.0175107954445577,0.000168810309252196,
-0.00881322390054543));
#54025=CARTESIAN_POINT('Ctrl Pts',(-0.0173747276067545,0.00017489430613416,
-0.00889477394844459));
#54026=CARTESIAN_POINT('Ctrl Pts',(-0.0172384887971941,0.000180428777406025,
-0.00897599879176508));
#54027=CARTESIAN_POINT('Ctrl Pts',(-0.0171021151044633,0.00018558234577026,
-0.00905704651762882));
#54028=CARTESIAN_POINT('Ctrl Pts',(-0.0169657414117325,0.000190735914134494,
-0.00913809424349255));
#54029=CARTESIAN_POINT('Ctrl Pts',(-0.0168292310524291,0.000195509330278561,
-0.00921896183497885));
#54030=CARTESIAN_POINT('Ctrl Pts',(-0.0166926437830518,0.0002,-0.00929970311937459));
#54031=CARTESIAN_POINT('Origin',(-0.00829461958536102,0.0002,-0.0140317242680344));
#54032=CARTESIAN_POINT('Origin',(0.,0.0002,0.));
#54033=CARTESIAN_POINT('Origin',(0.,0.0002,0.));
#54034=CARTESIAN_POINT('Ctrl Pts',(0.00624999999999999,0.0002,-0.0119660979437743));
#54035=CARTESIAN_POINT('Ctrl Pts',(0.00624999999999999,0.000198767450384323,
-0.0119660979437743));
#54036=CARTESIAN_POINT('Ctrl Pts',(0.00625000000000002,0.000197533969384649,
-0.011966110798073));
#54037=CARTESIAN_POINT('Ctrl Pts',(0.00625000000000002,0.000173042294632174,
-0.0119666221033105));
#54038=CARTESIAN_POINT('Ctrl Pts',(0.00624999999999949,0.000150239173956967,
-0.0119716741195774));
#54039=CARTESIAN_POINT('Ctrl Pts',(0.00624999999999945,0.000106108800044296,
-0.0119906202070117));
#54040=CARTESIAN_POINT('Ctrl Pts',(0.00624999999984408,8.55756873717683E-5,
-0.0120047838446837));
#54041=CARTESIAN_POINT('Ctrl Pts',(0.00624999999980556,4.81558075462784E-5,
-0.0120418505678853));
#54042=CARTESIAN_POINT('Ctrl Pts',(0.00625,3.23863339961406E-5,-0.0120652740542929));
#54043=CARTESIAN_POINT('Ctrl Pts',(0.00625,1.42587886819356E-5,-0.01210614745887));
#54044=CARTESIAN_POINT('Ctrl Pts',(0.00624999999996748,9.08500765451901E-6,
-0.0121221892847626));
#54045=CARTESIAN_POINT('Ctrl Pts',(0.00624999999993779,2.01730384467436E-6,
-0.0121551698535138));
#54046=CARTESIAN_POINT('Ctrl Pts',(0.00625000000000007,1.60816358981751E-7,
-0.0121720926860831));
#54047=CARTESIAN_POINT('Ctrl Pts',(0.00624999999999998,3.33362078418518E-9,
-0.0121897894713504));
#54048=CARTESIAN_POINT('Ctrl Pts',(0.00624999999999999,1.25106139975955E-19,
-0.0121905386717337));
#54049=CARTESIAN_POINT('Ctrl Pts',(0.00624999999999999,3.52129387358801E-30,
-0.0121912878729033));
#54050=CARTESIAN_POINT('Ctrl Pts',(0.00625000000000001,0.0002,0.0119660979437743));
#54051=CARTESIAN_POINT('Ctrl Pts',(0.00625000000000001,0.000177324851142135,
0.0119660979437743));
#54052=CARTESIAN_POINT('Ctrl Pts',(0.00624999999999523,0.000154964926961076,
0.0119704464772441));
#54053=CARTESIAN_POINT('Ctrl Pts',(0.0062499999999948,0.000109689157076455,
0.0119883494086744));
#54054=CARTESIAN_POINT('Ctrl Pts',(0.00624999999999042,8.78747849009445E-5,
0.0120028296365125));
#54055=CARTESIAN_POINT('Ctrl Pts',(0.00624999999998795,4.80234630210931E-5,
0.0120416364875857));
#54056=CARTESIAN_POINT('Ctrl Pts',(0.00625,3.13504886185185E-5,0.0120666257463726));
#54057=CARTESIAN_POINT('Ctrl Pts',(0.00625,6.91440040481353E-6,0.0121239135558641));
#54058=CARTESIAN_POINT('Ctrl Pts',(0.00624999999999996,3.00400145182888E-7,
0.0121564072571944));
#54059=CARTESIAN_POINT('Ctrl Pts',(0.00625,3.33362078410748E-9,0.0121897894713504));
#54060=CARTESIAN_POINT('Ctrl Pts',(0.00625000000000001,1.12063813495364E-19,
0.0121905386717337));
#54061=CARTESIAN_POINT('Ctrl Pts',(0.00625000000000001,2.82537309454408E-30,
0.0121912878729033));
#54062=CARTESIAN_POINT('Origin',(0.0125,0.0002,-4.59242549680257E-18));
#54063=CARTESIAN_POINT('Origin',(0.0125,0.0148,-4.59242549680257E-18));
#54064=CARTESIAN_POINT('Origin',(0.0125,0.0148,-0.0092));
#54065=CARTESIAN_POINT('Origin',(-0.00501982557395217,0.0132,-2.16840434497101E-19));
#54066=CARTESIAN_POINT('Origin',(-0.00501982557395217,0.0132,-0.0012));
#54067=CARTESIAN_POINT('Origin',(-0.000359710594690623,0.0128,-0.0122947390492059));
#54068=CARTESIAN_POINT('Origin',(-0.000359710594690624,0.0128,-0.0122947390492059));
#54069=CARTESIAN_POINT('Origin',(0.0125,0.0012,-4.59242549680257E-18));
#54070=CARTESIAN_POINT('Origin',(0.00625,0.0012,-0.0110556546617557));
#54071=CARTESIAN_POINT('Origin',(0.00625,0.0012,0.0110556546617557));
#54072=CARTESIAN_POINT('Origin',(0.00625,0.0012,-0.0110556546617557));
#54073=CARTESIAN_POINT('Origin',(0.00625,0.0012,-0.0110556546617557));
#54074=CARTESIAN_POINT('Origin',(0.00625,0.0012,0.0110556546617557));
#54075=CARTESIAN_POINT('Origin',(0.00625,0.0012,0.0110556546617557));
#54076=CARTESIAN_POINT('Origin',(0.00625,0.013,-0.0110556546617557));
#54077=CARTESIAN_POINT('Origin',(0.00625,0.0128,-0.0110556546617557));
#54078=CARTESIAN_POINT('Origin',(0.,0.0128,0.));
#54079=CARTESIAN_POINT('Ctrl Pts',(0.00585,0.013,-0.0108197735650983));
#54080=CARTESIAN_POINT('Ctrl Pts',(0.00585411539525861,0.013,-0.0108206833115983));
#54081=CARTESIAN_POINT('Ctrl Pts',(0.00585822747590886,0.0129999328797805,
-0.0108215885294959));
#54082=CARTESIAN_POINT('Ctrl Pts',(0.00586233275092189,0.0129998007010341,
-0.0108224887009578));
#54083=CARTESIAN_POINT('Ctrl Pts',(0.00587772753222075,0.012999305030735,
-0.0108258643439401));
#54084=CARTESIAN_POINT('Ctrl Pts',(0.00589302794065804,0.0129978980557532,
-0.0108291492821836));
#54085=CARTESIAN_POINT('Ctrl Pts',(0.00590815479426512,0.0129956754601165,
-0.0108323086673227));
#54086=CARTESIAN_POINT('Ctrl Pts',(0.00595353535508637,0.0129890076732063,
-0.0108417868227401));
#54087=CARTESIAN_POINT('Ctrl Pts',(0.00599741622959946,0.0129757147702998,
-0.0108502251386974));
#54088=CARTESIAN_POINT('Ctrl Pts',(0.00603890034360096,0.0129532705003051,
-0.0108585674477248));
#54089=CARTESIAN_POINT('Ctrl Pts',(0.00604258782040109,0.0129512754540834,
-0.010859308986305));
#54090=CARTESIAN_POINT('Ctrl Pts',(0.0060462546765892,0.012949201590918,
-0.0108600473853386));
#54091=CARTESIAN_POINT('Ctrl Pts',(0.00604988903132446,0.0129470486489094,
-0.0108607801373845));
#54092=CARTESIAN_POINT('Ctrl Pts',(0.00605329623888877,0.0129450302657765,
-0.0108614670924275));
#54093=CARTESIAN_POINT('Ctrl Pts',(0.00605667487947485,0.012942942385175,
-0.0108621490828373));
#54094=CARTESIAN_POINT('Ctrl Pts',(0.00606001515277547,0.0129407851029365,
-0.0108628240276582));
#54095=CARTESIAN_POINT('Ctrl Pts',(0.00608506720253009,0.0129246054861478,
-0.0108678861138156));
#54096=CARTESIAN_POINT('Ctrl Pts',(0.00610795458539415,0.0129044764792163,
-0.0108725465433551));
#54097=CARTESIAN_POINT('Ctrl Pts',(0.00612457636998883,0.0128808171431182,
-0.0108759551040394));
#54098=CARTESIAN_POINT('Ctrl Pts',(0.00613288726228617,0.0128689874750691,
-0.0108776593843815));
#54099=CARTESIAN_POINT('Ctrl Pts',(0.00613963379098558,0.0128562829565036,
-0.0108790527622001));
#54100=CARTESIAN_POINT('Ctrl Pts',(0.00614430549704848,0.0128427837238958,
-0.0108800251995936));
#54101=CARTESIAN_POINT('Ctrl Pts',(0.00614664135007993,0.0128360341075919,
-0.0108805114182903));
#54102=CARTESIAN_POINT('Ctrl Pts',(0.00614845841299802,0.0128290859420224,
-0.0108808921908321));
#54103=CARTESIAN_POINT('Ctrl Pts',(0.00614969177849169,0.0128219510061821,
-0.0108811518076324));
#54104=CARTESIAN_POINT('Ctrl Pts',(0.00615030846123852,0.012818383538262,
-0.0108812816160325));
#54105=CARTESIAN_POINT('Ctrl Pts',(0.0061507792028679,0.0128147694050756,
-0.0108813811091681));
#54106=CARTESIAN_POINT('Ctrl Pts',(0.00615109578867784,0.0128111103044368,
-0.0108814481716018));
#54107=CARTESIAN_POINT('Ctrl Pts',(0.00615141237448779,0.0128074512037979,
-0.0108815152340356));
#54108=CARTESIAN_POINT('Ctrl Pts',(0.00615157480559109,0.0128037471326604,
-0.0108815498625526));
#54109=CARTESIAN_POINT('Ctrl Pts',(0.00615157480314964,0.0128,-0.0108815498639328));
#54110=CARTESIAN_POINT('Origin',(0.00625,0.013,0.0110556546617557));
#54111=CARTESIAN_POINT('Ctrl Pts',(0.00615157480314962,0.013027940984764,
0.0108815498639328));
#54112=CARTESIAN_POINT('Ctrl Pts',(0.00615579813640361,0.0130304241847365,
0.0108791623225664));
#54113=CARTESIAN_POINT('Ctrl Pts',(0.00616006090484548,0.0130330332307525,
0.0108769553183616));
#54114=CARTESIAN_POINT('Ctrl Pts',(0.00618946868719457,0.0130516853607504,
0.0108630181858572));
#54115=CARTESIAN_POINT('Ctrl Pts',(0.00621674266005389,0.0130722240653073,
0.0108564778400306));
#54116=CARTESIAN_POINT('Ctrl Pts',(0.00628029283816163,0.0131269380048229,
0.0108547662808061));
#54117=CARTESIAN_POINT('Ctrl Pts',(0.00631551530880234,0.0131621010483139,
0.010863362352979));
#54118=CARTESIAN_POINT('Ctrl Pts',(0.00634727221305767,0.0131986668442575,
0.010880901825112));
#54119=CARTESIAN_POINT('Ctrl Pts',(0.00634784951391209,0.0131993334243132,
0.0108812244179529));
#54120=CARTESIAN_POINT('Ctrl Pts',(0.00634842519685039,0.0132,0.0108815498639327));
#54121=CARTESIAN_POINT('Ctrl Pts',(0.00585,0.013,-0.0108197735650983));
#54122=CARTESIAN_POINT('Ctrl Pts',(0.00595507260106555,0.013,-0.0106488169107487));
#54123=CARTESIAN_POINT('Ctrl Pts',(0.00595472383252994,0.0132006638620003,
-0.0106493843688813));
#54124=CARTESIAN_POINT('Ctrl Pts',(0.00599769697787199,0.013,-0.0108524233594023));
#54125=CARTESIAN_POINT('Ctrl Pts',(0.00606053271701144,0.0130441963819751,
-0.0107138924935219));
#54126=CARTESIAN_POINT('Ctrl Pts',(0.00614674466944171,0.0132005816098407,
-0.0107674030221155));
#54127=CARTESIAN_POINT('Ctrl Pts',(0.0061515748771313,0.012913544903149,
-0.0108815498221093));
#54128=CARTESIAN_POINT('Ctrl Pts',(0.00625026576929827,0.0129522781147389,
-0.0108257578692845));
#54129=CARTESIAN_POINT('Ctrl Pts',(0.00634882743980344,0.0130273960626492,
-0.0108817778740662));
#54130=CARTESIAN_POINT('Ctrl Pts',(0.0061515748031496,0.0128,-0.0108815498639328));
#54131=CARTESIAN_POINT('Ctrl Pts',(0.00625026565008664,0.0128,-0.0108257577998508));
#54132=CARTESIAN_POINT('Ctrl Pts',(0.00634882729611851,0.0128,-0.0108817777928458));
#54133=CARTESIAN_POINT('Origin',(0.00585,0.0132,-0.0108197735650983));
#54134=CARTESIAN_POINT('Origin',(0.0125,0.0132,-4.59242549680257E-18));
#54135=CARTESIAN_POINT('Ctrl Pts',(-0.127521969753009,0.00292791234232007,
0.0014375007351075));
#54136=CARTESIAN_POINT('Ctrl Pts',(-0.127521790582252,0.0027228384863398,
0.00149851530284674));
#54137=CARTESIAN_POINT('Ctrl Pts',(-0.127524929244986,0.00279751942631414,
0.0016989922391411));
#54138=CARTESIAN_POINT('Ctrl Pts',(-0.127135930686132,0.00292980295225595,
0.00144284563795753));
#54139=CARTESIAN_POINT('Ctrl Pts',(-0.127128303332053,0.00272468023725761,
0.00150425289890664));
#54140=CARTESIAN_POINT('Ctrl Pts',(-0.127086989041986,0.00279975471284059,
0.00170530652254589));
#54141=CARTESIAN_POINT('Ctrl Pts',(-0.126359755598941,0.00281040271795957,
0.00116400921661829));
#54142=CARTESIAN_POINT('Ctrl Pts',(-0.126391171205071,0.00262787967136648,
0.00125349479954768));
#54143=CARTESIAN_POINT('Ctrl Pts',(-0.126205867042022,0.00265838342822912,
0.00137542120560247));
#54144=CARTESIAN_POINT('Ctrl Pts',(-0.125844810804675,0.00261243102946704,
2.73686784602689E-5));
#54145=CARTESIAN_POINT('Ctrl Pts',(-0.125809482099816,0.00243981891809853,
3.02504277461029E-5));
#54146=CARTESIAN_POINT('Ctrl Pts',(-0.125622107008347,0.00242419343546421,
3.23331464449823E-5));
#54147=CARTESIAN_POINT('Ctrl Pts',(-0.126324661426851,0.00279922894991231,
-0.00113315917795553));
#54148=CARTESIAN_POINT('Ctrl Pts',(-0.126353424833284,0.00261785874660316,
-0.00122287857653872));
#54149=CARTESIAN_POINT('Ctrl Pts',(-0.126166065338315,0.00264516117224187,
-0.00133894667362534));
#54150=CARTESIAN_POINT('Ctrl Pts',(-0.127475667560966,0.00298937709191257,
-0.00158152248003426));
#54151=CARTESIAN_POINT('Ctrl Pts',(-0.127477698215336,0.00277625525457815,
-0.00163733766341933));
#54152=CARTESIAN_POINT('Ctrl Pts',(-0.127472373507598,0.00287024649410682,
-0.00186926883315216));
#54153=CARTESIAN_POINT('Ctrl Pts',(-0.128639088312426,0.00281072577948569,
-0.0011657258572821));
#54154=CARTESIAN_POINT('Ctrl Pts',(-0.128607647449207,0.00262816948297644,
-0.00125530022942571));
#54155=CARTESIAN_POINT('Ctrl Pts',(-0.12879282120482,0.00265876571215961,
-0.00137744992107518));
#54156=CARTESIAN_POINT('Ctrl Pts',(-0.129155327766085,0.00261238743571346,
-2.56552014421315E-5));
#54157=CARTESIAN_POINT('Ctrl Pts',(-0.129190650203713,0.00243978444592542,
-2.85609443698061E-5));
#54158=CARTESIAN_POINT('Ctrl Pts',(-0.129378050332955,0.00242414178609797,
-3.03066921534991E-5));
#54159=CARTESIAN_POINT('Ctrl Pts',(-0.128676003572727,0.00279905892909026,
0.00113193946402897));
#54160=CARTESIAN_POINT('Ctrl Pts',(-0.128647225777398,0.00261770650436977,
0.00122160652879797));
#54161=CARTESIAN_POINT('Ctrl Pts',(-0.12883468948467,0.00264495997721762,
0.00133750508047789));
#54162=CARTESIAN_POINT('Ctrl Pts',(-0.127908008885461,0.00292602173206305,
0.00143215583134956));
#54163=CARTESIAN_POINT('Ctrl Pts',(-0.127914748354504,0.00272099921368907,
0.00149278542731802));
#54164=CARTESIAN_POINT('Ctrl Pts',(-0.127962875152517,0.00279528411067127,
0.00169267787348758));
#54165=CARTESIAN_POINT('Ctrl Pts',(-0.127521969753009,0.00292791234232007,
0.0014375007351075));
#54166=CARTESIAN_POINT('Ctrl Pts',(-0.127521790582252,0.0027228384863398,
0.00149851530284674));
#54167=CARTESIAN_POINT('Ctrl Pts',(-0.127524929244986,0.00279751942631414,
0.0016989922391411));
#54168=CARTESIAN_POINT('Ctrl Pts',(-0.107521969753009,0.00292791234232008,
0.0014375007351075));
#54169=CARTESIAN_POINT('Ctrl Pts',(-0.107521790582252,0.00272283848633961,
0.00149851530284679));
#54170=CARTESIAN_POINT('Ctrl Pts',(-0.107524929244986,0.00279751942631421,
0.00169899223914127));
#54171=CARTESIAN_POINT('Ctrl Pts',(-0.107135930686132,0.00292980295225595,
0.00144284563795752));
#54172=CARTESIAN_POINT('Ctrl Pts',(-0.107128303332053,0.00272468023725742,
0.00150425289890669));
#54173=CARTESIAN_POINT('Ctrl Pts',(-0.107086989041985,0.00279975471284066,
0.00170530652254606));
#54174=CARTESIAN_POINT('Ctrl Pts',(-0.106359755598941,0.00281040271795956,
0.00116400921661828));
#54175=CARTESIAN_POINT('Ctrl Pts',(-0.106391171205071,0.00262787967136631,
0.00125349479954775));
#54176=CARTESIAN_POINT('Ctrl Pts',(-0.106205867042022,0.00265838342822915,
0.00137542120560257));
#54177=CARTESIAN_POINT('Ctrl Pts',(-0.105844810804675,0.00261243102946704,
2.73686784602542E-5));
#54178=CARTESIAN_POINT('Ctrl Pts',(-0.105809482099816,0.00243981891809839,
3.02504277460862E-5));
#54179=CARTESIAN_POINT('Ctrl Pts',(-0.105622107008346,0.00242419343546419,
3.23331464449678E-5));
#54180=CARTESIAN_POINT('Ctrl Pts',(-0.106324661426851,0.00279922894991231,
-0.00113315917795554));
#54181=CARTESIAN_POINT('Ctrl Pts',(-0.106353424833284,0.002617858746603,
-0.00122287857653881));
#54182=CARTESIAN_POINT('Ctrl Pts',(-0.106166065338315,0.0026451611722419,
-0.00133894667362546));
#54183=CARTESIAN_POINT('Ctrl Pts',(-0.107475667560966,0.00298937709191257,
-0.00158152248003427));
#54184=CARTESIAN_POINT('Ctrl Pts',(-0.107477698215336,0.00277625525457795,
-0.00163733766341938));
#54185=CARTESIAN_POINT('Ctrl Pts',(-0.107472373507598,0.0028702464941069,
-0.00186926883315237));
#54186=CARTESIAN_POINT('Ctrl Pts',(-0.108639088312426,0.00281072577948568,
-0.00116572585728207));
#54187=CARTESIAN_POINT('Ctrl Pts',(-0.108607647449207,0.00262816948297624,
-0.00125530022942576));
#54188=CARTESIAN_POINT('Ctrl Pts',(-0.10879282120482,0.00265876571215962,
-0.00137744992107526));
#54189=CARTESIAN_POINT('Ctrl Pts',(-0.109155327766085,0.00261238743571347,
-2.5655201442127E-5));
#54190=CARTESIAN_POINT('Ctrl Pts',(-0.109190650203713,0.00243978444592529,
-2.85609443698138E-5));
#54191=CARTESIAN_POINT('Ctrl Pts',(-0.109378050332955,0.00242414178609796,
-3.0306692153495E-5));
#54192=CARTESIAN_POINT('Ctrl Pts',(-0.108676003572727,0.00279905892909026,
0.00113193946402899));
#54193=CARTESIAN_POINT('Ctrl Pts',(-0.108647225777398,0.0026177065043696,
0.00122160652879808));
#54194=CARTESIAN_POINT('Ctrl Pts',(-0.108834689484669,0.00264495997721766,
0.00133750508047803));
#54195=CARTESIAN_POINT('Ctrl Pts',(-0.107908008885461,0.00292602173206305,
0.00143215583134956));
#54196=CARTESIAN_POINT('Ctrl Pts',(-0.107914748354504,0.00272099921368888,
0.00149278542731809));
#54197=CARTESIAN_POINT('Ctrl Pts',(-0.107962875152517,0.00279528411067133,
0.00169267787348776));
#54198=CARTESIAN_POINT('Ctrl Pts',(-0.107521969753009,0.00292791234232008,
0.0014375007351075));
#54199=CARTESIAN_POINT('Ctrl Pts',(-0.107521790582252,0.00272283848633961,
0.00149851530284679));
#54200=CARTESIAN_POINT('Ctrl Pts',(-0.107524929244986,0.00279751942631421,
0.00169899223914127));
#54201=CARTESIAN_POINT('Ctrl Pts',(-0.087521969753009,0.00292791234232007,
0.0014375007351075));
#54202=CARTESIAN_POINT('Ctrl Pts',(-0.0875217905822522,0.00272283848633951,
0.00149851530284683));
#54203=CARTESIAN_POINT('Ctrl Pts',(-0.0875249292449862,0.00279751942631424,
0.00169899223914137));
#54204=CARTESIAN_POINT('Ctrl Pts',(-0.0871359306861318,0.00292980295225596,
0.00144284563795755));
#54205=CARTESIAN_POINT('Ctrl Pts',(-0.087128303332053,0.00272468023725732,
0.00150425289890676));
#54206=CARTESIAN_POINT('Ctrl Pts',(-0.0870869890419856,0.0027997547128407,
0.00170530652254619));
#54207=CARTESIAN_POINT('Ctrl Pts',(-0.0863597555989418,0.00281040271795959,
0.00116400921661838));
#54208=CARTESIAN_POINT('Ctrl Pts',(-0.0863911712050714,0.00262787967136625,
0.00125349479954789));
#54209=CARTESIAN_POINT('Ctrl Pts',(-0.0862058670420218,0.0026583834282292,
0.00137542120560275));
#54210=CARTESIAN_POINT('Ctrl Pts',(-0.0858448108046749,0.00261243102946704,
2.73686784603756E-5));
#54211=CARTESIAN_POINT('Ctrl Pts',(-0.0858094820998151,0.00243981891809831,
3.02504277462256E-5));
#54212=CARTESIAN_POINT('Ctrl Pts',(-0.0856221070083461,0.00242419343546418,
3.23331464451119E-5));
#54213=CARTESIAN_POINT('Ctrl Pts',(-0.0863246614268507,0.00279922894991229,
-0.00113315917795547));
#54214=CARTESIAN_POINT('Ctrl Pts',(-0.0863534248332843,0.00261785874660288,
-0.00122287857653878));
#54215=CARTESIAN_POINT('Ctrl Pts',(-0.0861660653383145,0.00264516117224188,
-0.00133894667362542));
#54216=CARTESIAN_POINT('Ctrl Pts',(-0.0874756675609659,0.00298937709191257,
-0.00158152248003427));
#54217=CARTESIAN_POINT('Ctrl Pts',(-0.0874776982153359,0.00277625525457783,
-0.00163733766341943));
#54218=CARTESIAN_POINT('Ctrl Pts',(-0.0874723735075982,0.00287024649410694,
-0.00186926883315248));
#54219=CARTESIAN_POINT('Ctrl Pts',(-0.0886390883124264,0.00281072577948571,
-0.00116572585728214));
#54220=CARTESIAN_POINT('Ctrl Pts',(-0.088607647449207,0.00262816948297619,
-0.00125530022942588));
#54221=CARTESIAN_POINT('Ctrl Pts',(-0.0887928212048197,0.00265876571215967,
-0.00137744992107541));
#54222=CARTESIAN_POINT('Ctrl Pts',(-0.0891553277660854,0.00261238743571347,
-2.56552014422575E-5));
#54223=CARTESIAN_POINT('Ctrl Pts',(-0.0891906502037131,0.00243978444592521,
-2.85609443699477E-5));
#54224=CARTESIAN_POINT('Ctrl Pts',(-0.0893780503329556,0.00242414178609795,
-3.030669215365E-5));
#54225=CARTESIAN_POINT('Ctrl Pts',(-0.0886760035727276,0.00279905892909023,
0.0011319394640289));
#54226=CARTESIAN_POINT('Ctrl Pts',(-0.0886472257773982,0.0026177065043695,
0.00122160652879803));
#54227=CARTESIAN_POINT('Ctrl Pts',(-0.0888346894846697,0.00264495997721763,
0.00133750508047797));
#54228=CARTESIAN_POINT('Ctrl Pts',(-0.0879080088854605,0.00292602173206304,
0.00143215583134954));
#54229=CARTESIAN_POINT('Ctrl Pts',(-0.0879147483545036,0.00272099921368876,
0.00149278542731808));
#54230=CARTESIAN_POINT('Ctrl Pts',(-0.0879628751525175,0.00279528411067136,
0.00169267787348782));
#54231=CARTESIAN_POINT('Ctrl Pts',(-0.087521969753009,0.00292791234232007,
0.0014375007351075));
#54232=CARTESIAN_POINT('Ctrl Pts',(-0.0875217905822522,0.00272283848633951,
0.00149851530284683));
#54233=CARTESIAN_POINT('Ctrl Pts',(-0.0875249292449862,0.00279751942631424,
0.00169899223914137));
#54234=CARTESIAN_POINT('Ctrl Pts',(-0.0675219697530089,0.00292791234232007,
0.0014375007351075));
#54235=CARTESIAN_POINT('Ctrl Pts',(-0.0675217905822521,0.00272283848633946,
0.00149851530284684));
#54236=CARTESIAN_POINT('Ctrl Pts',(-0.0675249292449862,0.00279751942631426,
0.00169899223914141));
#54237=CARTESIAN_POINT('Ctrl Pts',(-0.0671359306861318,0.00292980295225596,
0.00144284563795754));
#54238=CARTESIAN_POINT('Ctrl Pts',(-0.0671283033320531,0.00272468023725727,
0.00150425289890677));
#54239=CARTESIAN_POINT('Ctrl Pts',(-0.0670869890419856,0.00279975471284072,
0.00170530652254623));
#54240=CARTESIAN_POINT('Ctrl Pts',(-0.0663597555989418,0.00281040271795959,
0.00116400921661836));
#54241=CARTESIAN_POINT('Ctrl Pts',(-0.0663911712050714,0.00262787967136621,
0.00125349479954789));
#54242=CARTESIAN_POINT('Ctrl Pts',(-0.0662058670420217,0.0026583834282292,
0.00137542120560276));
#54243=CARTESIAN_POINT('Ctrl Pts',(-0.065844810804675,0.00261243102946704,
2.73686784603625E-5));
#54244=CARTESIAN_POINT('Ctrl Pts',(-0.0658094820998151,0.00243981891809827,
3.02504277462119E-5));
#54245=CARTESIAN_POINT('Ctrl Pts',(-0.0656221070083461,0.00242419343546418,
3.23331464450973E-5));
#54246=CARTESIAN_POINT('Ctrl Pts',(-0.0663246614268507,0.00279922894991229,
-0.00113315917795546));
#54247=CARTESIAN_POINT('Ctrl Pts',(-0.0663534248332843,0.00261785874660285,
-0.00122287857653879));
#54248=CARTESIAN_POINT('Ctrl Pts',(-0.0661660653383145,0.00264516117224189,
-0.00133894667362545));
#54249=CARTESIAN_POINT('Ctrl Pts',(-0.067475667560966,0.00298937709191257,
-0.00158152248003427));
#54250=CARTESIAN_POINT('Ctrl Pts',(-0.0674776982153359,0.00277625525457778,
-0.00163733766341944));
#54251=CARTESIAN_POINT('Ctrl Pts',(-0.0674723735075983,0.00287024649410697,
-0.00186926883315253));
#54252=CARTESIAN_POINT('Ctrl Pts',(-0.0686390883124264,0.00281072577948571,
-0.00116572585728214));
#54253=CARTESIAN_POINT('Ctrl Pts',(-0.068607647449207,0.00262816948297615,
-0.0012553002294259));
#54254=CARTESIAN_POINT('Ctrl Pts',(-0.0687928212048197,0.00265876571215968,
-0.00137744992107544));
#54255=CARTESIAN_POINT('Ctrl Pts',(-0.0691553277660854,0.00261238743571347,
-2.56552014422452E-5));
#54256=CARTESIAN_POINT('Ctrl Pts',(-0.0691906502037132,0.00243978444592516,
-2.85609443699341E-5));
#54257=CARTESIAN_POINT('Ctrl Pts',(-0.0693780503329557,0.00242414178609795,
-3.03066921536361E-5));
#54258=CARTESIAN_POINT('Ctrl Pts',(-0.0686760035727276,0.00279905892909023,
0.00113193946402892));
#54259=CARTESIAN_POINT('Ctrl Pts',(-0.0686472257773982,0.00261770650436945,
0.00122160652879807));
#54260=CARTESIAN_POINT('Ctrl Pts',(-0.0688346894846698,0.00264495997721765,
0.00133750508047802));
#54261=CARTESIAN_POINT('Ctrl Pts',(-0.0679080088854605,0.00292602173206304,
0.00143215583134953));
#54262=CARTESIAN_POINT('Ctrl Pts',(-0.0679147483545036,0.00272099921368871,
0.0014927854273181));
#54263=CARTESIAN_POINT('Ctrl Pts',(-0.0679628751525174,0.00279528411067137,
0.00169267787348788));
#54264=CARTESIAN_POINT('Ctrl Pts',(-0.0675219697530089,0.00292791234232007,
0.0014375007351075));
#54265=CARTESIAN_POINT('Ctrl Pts',(-0.0675217905822521,0.00272283848633946,
0.00149851530284684));
#54266=CARTESIAN_POINT('Ctrl Pts',(-0.0675249292449862,0.00279751942631426,
0.00169899223914141));
#54267=CARTESIAN_POINT('Ctrl Pts',(-0.047521969753009,0.00292791234232007,
0.0014375007351075));
#54268=CARTESIAN_POINT('Ctrl Pts',(-0.0475217905822521,0.00272283848633948,
0.00149851530284684));
#54269=CARTESIAN_POINT('Ctrl Pts',(-0.0475249292449862,0.00279751942631425,
0.00169899223914139));
#54270=CARTESIAN_POINT('Ctrl Pts',(-0.0471359306861318,0.00292980295225596,
0.00144284563795755));
#54271=CARTESIAN_POINT('Ctrl Pts',(-0.0471283033320531,0.0027246802372573,
0.00150425289890676));
#54272=CARTESIAN_POINT('Ctrl Pts',(-0.0470869890419856,0.00279975471284071,
0.00170530652254621));
#54273=CARTESIAN_POINT('Ctrl Pts',(-0.0463597555989418,0.00281040271795959,
0.00116400921661837));
#54274=CARTESIAN_POINT('Ctrl Pts',(-0.0463911712050714,0.00262787967136623,
0.00125349479954789));
#54275=CARTESIAN_POINT('Ctrl Pts',(-0.0462058670420217,0.0026583834282292,
0.00137542120560276));
#54276=CARTESIAN_POINT('Ctrl Pts',(-0.0458448108046749,0.00261243102946703,
2.73686784603569E-5));
#54277=CARTESIAN_POINT('Ctrl Pts',(-0.0458094820998151,0.00243981891809829,
3.02504277461982E-5));
#54278=CARTESIAN_POINT('Ctrl Pts',(-0.0456221070083461,0.00242419343546418,
3.23331464450899E-5));
#54279=CARTESIAN_POINT('Ctrl Pts',(-0.0463246614268507,0.00279922894991229,
-0.00113315917795547));
#54280=CARTESIAN_POINT('Ctrl Pts',(-0.0463534248332843,0.00261785874660286,
-0.00122287857653879));
#54281=CARTESIAN_POINT('Ctrl Pts',(-0.0461660653383145,0.00264516117224189,
-0.00133894667362545));
#54282=CARTESIAN_POINT('Ctrl Pts',(-0.047475667560966,0.00298937709191257,
-0.00158152248003427));
#54283=CARTESIAN_POINT('Ctrl Pts',(-0.0474776982153359,0.0027762552545778,
-0.00163733766341943));
#54284=CARTESIAN_POINT('Ctrl Pts',(-0.0474723735075983,0.00287024649410696,
-0.00186926883315251));
#54285=CARTESIAN_POINT('Ctrl Pts',(-0.0486390883124264,0.00281072577948571,
-0.00116572585728214));
#54286=CARTESIAN_POINT('Ctrl Pts',(-0.048607647449207,0.00262816948297617,
-0.00125530022942588));
#54287=CARTESIAN_POINT('Ctrl Pts',(-0.0487928212048197,0.00265876571215968,
-0.00137744992107542));
#54288=CARTESIAN_POINT('Ctrl Pts',(-0.0491553277660853,0.00261238743571346,
-2.56552014422379E-5));
#54289=CARTESIAN_POINT('Ctrl Pts',(-0.0491906502037132,0.00243978444592517,
-2.85609443699274E-5));
#54290=CARTESIAN_POINT('Ctrl Pts',(-0.0493780503329557,0.00242414178609795,
-3.03066921536269E-5));
#54291=CARTESIAN_POINT('Ctrl Pts',(-0.0486760035727277,0.00279905892909024,
0.00113193946402892));
#54292=CARTESIAN_POINT('Ctrl Pts',(-0.0486472257773982,0.00261770650436948,
0.00122160652879805));
#54293=CARTESIAN_POINT('Ctrl Pts',(-0.0488346894846697,0.00264495997721764,
0.00133750508047801));
#54294=CARTESIAN_POINT('Ctrl Pts',(-0.0479080088854605,0.00292602173206304,
0.00143215583134954));
#54295=CARTESIAN_POINT('Ctrl Pts',(-0.0479147483545036,0.00272099921368874,
0.00149278542731809));
#54296=CARTESIAN_POINT('Ctrl Pts',(-0.0479628751525174,0.00279528411067136,
0.00169267787348785));
#54297=CARTESIAN_POINT('Ctrl Pts',(-0.047521969753009,0.00292791234232007,
0.0014375007351075));
#54298=CARTESIAN_POINT('Ctrl Pts',(-0.0475217905822521,0.00272283848633948,
0.00149851530284684));
#54299=CARTESIAN_POINT('Ctrl Pts',(-0.0475249292449862,0.00279751942631425,
0.00169899223914139));
#54300=CARTESIAN_POINT('Origin',(-0.0183187040774608,0.000201195130235789,
0.0081064157789351));
#54301=CARTESIAN_POINT('Origin',(-0.0192596558562786,-0.000820619857582921,
0.00981391272232187));
#54302=CARTESIAN_POINT('Ctrl Pts',(-0.0167335787825944,0.000199999999999998,
0.0092755050776766));
#54303=CARTESIAN_POINT('Ctrl Pts',(-0.0167989534819831,0.000445675548177814,
0.00923685991535881));
#54304=CARTESIAN_POINT('Ctrl Pts',(-0.0168953032845749,0.000683360688027424,
0.00925546810437307));
#54305=CARTESIAN_POINT('Ctrl Pts',(-0.0168884171052221,0.000194945401620732,
0.00918397498779601));
#54306=CARTESIAN_POINT('Ctrl Pts',(-0.0169566045154461,0.000427726110919411,
0.00915087413831594));
#54307=CARTESIAN_POINT('Ctrl Pts',(-0.0170529779122477,0.000652022804612772,
0.00916927738948391));
#54308=CARTESIAN_POINT('Ctrl Pts',(-0.0171958663208298,0.000184166395058654,
0.00900179253952732));
#54309=CARTESIAN_POINT('Ctrl Pts',(-0.0172687191497198,0.000389409848041071,
0.00897906560874024));
#54310=CARTESIAN_POINT('Ctrl Pts',(-0.0173642546158974,0.000585686088741027,
0.00899657312123159));
#54311=CARTESIAN_POINT('Ctrl Pts',(-0.0176463723131326,0.000165442575407028,
0.00873284458653405));
#54312=CARTESIAN_POINT('Ctrl Pts',(-0.0177222065528446,0.000322469294492184,
0.00872197465762366));
#54313=CARTESIAN_POINT('Ctrl Pts',(-0.0178122797421618,0.000471566164156617,
0.00873578171227763));
#54314=CARTESIAN_POINT('Ctrl Pts',(-0.0180089482080531,0.00014654221914008,
0.00851355328316542));
#54315=CARTESIAN_POINT('Ctrl Pts',(-0.0180815789893364,0.00025422082507978,
0.00850731258360253));
#54316=CARTESIAN_POINT('Ctrl Pts',(-0.0181617121620799,0.000356444186374595,
0.00851412153872697));
#54317=CARTESIAN_POINT('Ctrl Pts',(-0.0182653366435107,0.000127597262669883,
0.00835462058997495));
#54318=CARTESIAN_POINT('Ctrl Pts',(-0.0183286217321492,0.000184709407290683,
0.00834469986689284));
#54319=CARTESIAN_POINT('Ctrl Pts',(-0.0183949042260683,0.000239045421227612,
0.00834000019373098));
#54320=CARTESIAN_POINT('Ctrl Pts',(-0.0183638281572847,0.000113747397695859,
0.00828933270869108));
#54321=CARTESIAN_POINT('Ctrl Pts',(-0.018416358529888,0.000132790739820186,
0.00827019203209158));
#54322=CARTESIAN_POINT('Ctrl Pts',(-0.0184701394209955,0.000150558685463742,
0.00825332284927026));
#54323=CARTESIAN_POINT('Ctrl Pts',(-0.0183575213134859,0.000106149127372226,
0.00828837051540356));
#54324=CARTESIAN_POINT('Ctrl Pts',(-0.0184024414311689,0.000103709091286823,
0.00826031051413278));
#54325=CARTESIAN_POINT('Ctrl Pts',(-0.0184485607971002,9.99542717525335E-5,
0.00823442538642541));
#54326=CARTESIAN_POINT('Origin',(-0.0177513235169945,0.000199999999999973,
0.0109971890369446));
#54327=CARTESIAN_POINT('Ctrl Pts',(-0.0151447495921968,0.00165220181413017,
0.0102147149330532));
#54328=CARTESIAN_POINT('Ctrl Pts',(-0.0152060889391142,0.00159854195139627,
0.0101784552021597));
#54329=CARTESIAN_POINT('Ctrl Pts',(-0.0152709311364255,0.00154471125155936,
0.0101488045799563));
#54330=CARTESIAN_POINT('Ctrl Pts',(-0.0149661476183632,0.00131323993358782,
0.0103202925086844));
#54331=CARTESIAN_POINT('Ctrl Pts',(-0.015026744798365,0.00132849279769074,
0.0102844714970778));
#54332=CARTESIAN_POINT('Ctrl Pts',(-0.0150879954762257,0.00134387673222698,
0.0102498911921733));
#54333=CARTESIAN_POINT('Ctrl Pts',(-0.0152846624930786,0.000915866669368474,
0.0101320077571046));
#54334=CARTESIAN_POINT('Ctrl Pts',(-0.0153480148170758,0.00101115245864742,
0.0100945580882847));
#54335=CARTESIAN_POINT('Ctrl Pts',(-0.0154164122352271,0.00110671945758542,
0.010068445155131));
#54336=CARTESIAN_POINT('Ctrl Pts',(-0.0157806659000851,0.00060625922996491,
0.00983880362227603));
#54337=CARTESIAN_POINT('Ctrl Pts',(-0.0158458549228214,0.000765968566367971,
0.00980026821960143));
#54338=CARTESIAN_POINT('Ctrl Pts',(-0.0159248091463299,0.000923634413820413,
0.00978867700564263));
#54339=CARTESIAN_POINT('Ctrl Pts',(-0.0163137554251612,0.000352348673268969,
0.00952367664778722));
#54340=CARTESIAN_POINT('Ctrl Pts',(-0.0163805746329843,0.000566476009334006,
0.00948417758842814));
#54341=CARTESIAN_POINT('Ctrl Pts',(-0.0164702186466373,0.000775802287379282,
0.00948955553669219));
#54342=CARTESIAN_POINT('Ctrl Pts',(-0.0167006112850335,0.000209372126995855,
0.00929499326357058));
#54343=CARTESIAN_POINT('Ctrl Pts',(-0.0167673355456445,0.000456254808588579,
0.00925555033064982));
#54344=CARTESIAN_POINT('Ctrl Pts',(-0.0168647148508793,0.000695249121534255,
0.00927416129940651));
#54345=CARTESIAN_POINT('Ctrl Pts',(-0.0169280464492866,0.00013215739489152,
0.0091605487625401));
#54346=CARTESIAN_POINT('Ctrl Pts',(-0.0169943093597287,0.000397467558198914,
0.00912137854910013));
#54347=CARTESIAN_POINT('Ctrl Pts',(-0.0170961872877718,0.000652854831667682,
0.00914812433229151));
#54348=CARTESIAN_POINT('Origin',(-0.0160885892837263,0.00138685515994303,
0.0119750415244209));
#54349=CARTESIAN_POINT('Origin',(-0.0160872238541987,0.00194341959324476,
0.0119756128465044));
#54350=CARTESIAN_POINT('Origin',(-0.0160859565839347,0.00250003209534414,
0.0119763645202741));
#54351=CARTESIAN_POINT('Origin',(-0.0159726371414409,0.00698837807496495,
0.0117686012574936));
#54352=CARTESIAN_POINT('Origin',(-0.0159723098794419,0.0114765413480154,
0.0117691396498924));
#54353=CARTESIAN_POINT('Ctrl Pts',(-0.0177441069319941,0.0132668179233314,
0.00867814822976128));
#54354=CARTESIAN_POINT('Ctrl Pts',(-0.0178357661804268,0.0129212136767161,
0.00862396539501086));
#54355=CARTESIAN_POINT('Ctrl Pts',(-0.0179860636964262,0.0125974920464792,
0.0086822238418441));
#54356=CARTESIAN_POINT('Ctrl Pts',(-0.0174438743220729,0.013159204780945,
0.00885562572567315));
#54357=CARTESIAN_POINT('Ctrl Pts',(-0.0175359527092885,0.012837517340567,
0.00880119512403525));
#54358=CARTESIAN_POINT('Ctrl Pts',(-0.0176783448733239,0.0125332124555831,
0.0088462220838624));
#54359=CARTESIAN_POINT('Ctrl Pts',(-0.0169089556228614,0.012949243145523,
0.0091718339859198));
#54360=CARTESIAN_POINT('Ctrl Pts',(-0.0169998667382091,0.0126714308781741,
0.00911809339755667));
#54361=CARTESIAN_POINT('Ctrl Pts',(-0.0171277195811297,0.012404131932755,
0.00914119593583115));
#54362=CARTESIAN_POINT('Ctrl Pts',(-0.0161568173119193,0.012587525687478,
0.00961644799383991));
#54363=CARTESIAN_POINT('Ctrl Pts',(-0.0162421507775504,0.0123793205558015,
0.00956600454000768));
#54364=CARTESIAN_POINT('Ctrl Pts',(-0.0163495719378372,0.0121753390197973,
0.0095617513260173));
#54365=CARTESIAN_POINT('Ctrl Pts',(-0.0156006461865971,0.0122442363754161,
0.00994521927103916));
#54366=CARTESIAN_POINT('Ctrl Pts',(-0.015679742844943,0.0120991303276778,
0.00989846260172805));
#54367=CARTESIAN_POINT('Ctrl Pts',(-0.0157711425114264,0.0119553567280747,
0.00987670168726923));
#54368=CARTESIAN_POINT('Ctrl Pts',(-0.0151605030169284,0.0118388471177341,
0.0102054025589772));
#54369=CARTESIAN_POINT('Ctrl Pts',(-0.0152322413348173,0.0117684582609837,
0.0101629956498054));
#54370=CARTESIAN_POINT('Ctrl Pts',(-0.0153083644911994,0.0116978452664201,
0.0101297128986875));
#54371=CARTESIAN_POINT('Ctrl Pts',(-0.0149980581487341,0.0114857175403946,
0.0103014291313018));
#54372=CARTESIAN_POINT('Ctrl Pts',(-0.015063582233244,0.011482507293876,
0.0102626956624571));
#54373=CARTESIAN_POINT('Ctrl Pts',(-0.0151307389308278,0.0114792190702809,
0.0102268871915435));
#54374=CARTESIAN_POINT('Ctrl Pts',(-0.0151300208199999,0.0112383215488602,
0.0102234216008868));
#54375=CARTESIAN_POINT('Ctrl Pts',(-0.0151931734358564,0.011286730281564,
0.0101860899861687));
#54376=CARTESIAN_POINT('Ctrl Pts',(-0.0152598713370855,0.0113352008367595,
0.0101554707885479));
#54377=CARTESIAN_POINT('Origin',(-0.0185790388714426,0.0132,0.010507898921278));
#54378=CARTESIAN_POINT('Ctrl Pts',(-0.0194832368868348,0.0133370288977843,
0.0075874409832765));
#54379=CARTESIAN_POINT('Ctrl Pts',(-0.0195033028657649,0.0134070877928086,
0.00749672395384876));
#54380=CARTESIAN_POINT('Ctrl Pts',(-0.0195278886848258,0.013483568243638,
0.00741351892276558));
#54381=CARTESIAN_POINT('Ctrl Pts',(-0.0197507818214645,0.0133230133512749,
0.00744372563506592));
#54382=CARTESIAN_POINT('Ctrl Pts',(-0.0198087010863357,0.0133342024701371,
0.00741111088576182));
#54383=CARTESIAN_POINT('Ctrl Pts',(-0.0198664298167596,0.0133454743880182,
0.00737820542396837));
#54384=CARTESIAN_POINT('Ctrl Pts',(-0.0195727782976753,0.013304973067155,
0.00756333620365235));
#54385=CARTESIAN_POINT('Ctrl Pts',(-0.0196609338252826,0.0132429781941271,
0.00755714489238573));
#54386=CARTESIAN_POINT('Ctrl Pts',(-0.0197531840062628,0.0131867131153442,
0.00755729857743586));
#54387=CARTESIAN_POINT('Ctrl Pts',(-0.0191783091553242,0.0132841167698863,
0.00780994181632697));
#54388=CARTESIAN_POINT('Ctrl Pts',(-0.019287093290927,0.0131399142662646,
0.00781104542072873));
#54389=CARTESIAN_POINT('Ctrl Pts',(-0.0194095336013034,0.0130093728973814,
0.00783616050338385));
#54390=CARTESIAN_POINT('Ctrl Pts',(-0.018716108312103,0.0132659245783802,
0.00809240117807621));
#54391=CARTESIAN_POINT('Ctrl Pts',(-0.0188305568961298,0.0130510820638524,
0.00808446146002699));
#54392=CARTESIAN_POINT('Ctrl Pts',(-0.0189716132786577,0.0128562445176172,
0.00812308749445927));
#54393=CARTESIAN_POINT('Ctrl Pts',(-0.0180691343143712,0.0132449233701698,
0.00848290936225995));
#54394=CARTESIAN_POINT('Ctrl Pts',(-0.018175922042617,0.0129492634754963,
0.0084494961400988));
#54395=CARTESIAN_POINT('Ctrl Pts',(-0.0183289512107979,0.0126768011770632,
0.00849786999827214));
#54396=CARTESIAN_POINT('Ctrl Pts',(-0.0175928450092797,0.0132323460363387,
0.00876779160005616));
#54397=CARTESIAN_POINT('Ctrl Pts',(-0.0176865783709503,0.012888524988684,
0.00870884960536136));
#54398=CARTESIAN_POINT('Ctrl Pts',(-0.0178402497241257,0.0125657338012786,
0.00876073459359184));
#54399=CARTESIAN_POINT('Ctrl Pts',(-0.0173143432412806,0.0132257325396149,
0.00893390798783256));
#54400=CARTESIAN_POINT('Ctrl Pts',(-0.0173993515205757,0.0128564725832721,
0.00885895734423144));
#54401=CARTESIAN_POINT('Ctrl Pts',(-0.0175519300652605,0.0125057034540625,
0.00891265565385289));
#54402=CARTESIAN_POINT('Origin',(-0.0204666233347745,0.0145154811894642,
0.00888488367021892));
#54403=CARTESIAN_POINT('Origin',(-0.0197053153855647,0.013197642208147,
0.00729146575043895));
#54404=CARTESIAN_POINT('Origin',(-0.0197429273583666,0.0131963056902179,
-0.00726122969914678));
#54405=CARTESIAN_POINT('Origin',(-0.0206317819659218,0.0145314876015483,
-0.00877324474953166));
#54406=CARTESIAN_POINT('Ctrl Pts',(-0.0174781162006161,0.013194947177096,
-0.0088353455161641));
#54407=CARTESIAN_POINT('Ctrl Pts',(-0.0175651094419168,0.0128357627682235,
-0.00876647747827708));
#54408=CARTESIAN_POINT('Ctrl Pts',(-0.0177156087422018,0.0124953957683154,
-0.00881967683902286));
#54409=CARTESIAN_POINT('Ctrl Pts',(-0.0177606237719999,0.0132038679035857,
-0.00866858423663555));
#54410=CARTESIAN_POINT('Ctrl Pts',(-0.0178559242864338,0.0128699235417939,
-0.00861502263776792));
#54411=CARTESIAN_POINT('Ctrl Pts',(-0.0180074828014301,0.0125570715094477,
-0.00866647111554646));
#54412=CARTESIAN_POINT('Ctrl Pts',(-0.0182385379182696,0.0132206414165277,
-0.00838543393250545));
#54413=CARTESIAN_POINT('Ctrl Pts',(-0.0183460042794801,0.0129337933037081,
-0.00835600790222576));
#54414=CARTESIAN_POINT('Ctrl Pts',(-0.0184968930862299,0.0126698469468547,
-0.00840408638510566));
#54415=CARTESIAN_POINT('Ctrl Pts',(-0.0188888690299216,0.0132487916607732,
-0.00799516388057441));
#54416=CARTESIAN_POINT('Ctrl Pts',(-0.0190027510573474,0.013040834514991,
-0.00798953516750174));
#54417=CARTESIAN_POINT('Ctrl Pts',(-0.0191416149041577,0.0128523958496762,
-0.00802801969736298));
#54418=CARTESIAN_POINT('Ctrl Pts',(-0.0193515121113206,0.0132730699882502,
-0.00771267516059409));
#54419=CARTESIAN_POINT('Ctrl Pts',(-0.0194591200995059,0.0131333169586524,
-0.00771518874178041));
#54420=CARTESIAN_POINT('Ctrl Pts',(-0.0195796088335704,0.0130068717409757,
-0.00774050347429506));
#54421=CARTESIAN_POINT('Ctrl Pts',(-0.0197520638492665,0.0133014617255382,
-0.00746014347801861));
#54422=CARTESIAN_POINT('Ctrl Pts',(-0.0198383763909096,0.0132421977052975,
-0.00745470174054145));
#54423=CARTESIAN_POINT('Ctrl Pts',(-0.0199284951832807,0.0131884258500566,
-0.00745514727070188));
#54424=CARTESIAN_POINT('Ctrl Pts',(-0.0199259467555682,0.013325645265776,
-0.00733877763912789));
#54425=CARTESIAN_POINT('Ctrl Pts',(-0.0199821693467795,0.0133364139738675,
-0.0073070177250494));
#54426=CARTESIAN_POINT('Ctrl Pts',(-0.0200382272496652,0.0133472837983618,
-0.00727504149123732));
#54427=CARTESIAN_POINT('Ctrl Pts',(-0.0196560990591099,0.0133445491409245,
-0.00747672950133648));
#54428=CARTESIAN_POINT('Ctrl Pts',(-0.0196754866009051,0.0134118597671077,
-0.00738859481309351));
#54429=CARTESIAN_POINT('Ctrl Pts',(-0.0196990588301704,0.0134852524349443,
-0.00730742671988614));
#54430=CARTESIAN_POINT('Origin',(-0.018737818639568,0.0132,-0.0104140389116816));
#54431=CARTESIAN_POINT('Ctrl Pts',(-0.0154071766236069,0.0110829233457151,
-0.0100595855738323));
#54432=CARTESIAN_POINT('Ctrl Pts',(-0.0154721194094679,0.0111605951364923,
-0.0100211957298243));
#54433=CARTESIAN_POINT('Ctrl Pts',(-0.0155420327037426,0.0112386794535643,
-0.00999279989496569));
#54434=CARTESIAN_POINT('Ctrl Pts',(-0.0151569212422682,0.0113984171585124,
-0.0102075198652812));
#54435=CARTESIAN_POINT('Ctrl Pts',(-0.0152241770747978,0.0114088953369853,
-0.0101677627025652));
#54436=CARTESIAN_POINT('Ctrl Pts',(-0.0152926460101778,0.0114192048693264,
-0.0101300478717502));
#54437=CARTESIAN_POINT('Ctrl Pts',(-0.0153264432539109,0.0118064921096535,
-0.0101073097577375));
#54438=CARTESIAN_POINT('Ctrl Pts',(-0.0154009334344641,0.0117391296807366,
-0.0100632761308695));
#54439=CARTESIAN_POINT('Ctrl Pts',(-0.0154795359860423,0.0116713561529081,
-0.0100281788720059));
#54440=CARTESIAN_POINT('Ctrl Pts',(-0.0157884970821157,0.0122415169423427,
-0.00983417434973566));
#54441=CARTESIAN_POINT('Ctrl Pts',(-0.0158707293602409,0.0120936580781721,
-0.00978556411113859));
#54442=CARTESIAN_POINT('Ctrl Pts',(-0.0159658709218911,0.0119472439393342,
-0.00976324159438402));
#54443=CARTESIAN_POINT('Ctrl Pts',(-0.0163381224989415,0.0125871909279286,
-0.00950927245885394));
#54444=CARTESIAN_POINT('Ctrl Pts',(-0.0164265291225076,0.0123754678951022,
-0.00945701235900225));
#54445=CARTESIAN_POINT('Ctrl Pts',(-0.0165379212236351,0.0121682558124033,
-0.00945287823563186));
#54446=CARTESIAN_POINT('Ctrl Pts',(-0.0171083583317725,0.0129643053446502,
-0.00905396040295069));
#54447=CARTESIAN_POINT('Ctrl Pts',(-0.0172023924942094,0.0126795827432054,
-0.00899837367743349));
#54448=CARTESIAN_POINT('Ctrl Pts',(-0.0173348713317463,0.0124060676027306,
-0.00902366736927392));
#54449=CARTESIAN_POINT('Ctrl Pts',(-0.0176718370399433,0.0131859419718071,
-0.00872086937012763));
#54450=CARTESIAN_POINT('Ctrl Pts',(-0.0177670254041465,0.0128543108135448,
-0.00866460035749818));
#54451=CARTESIAN_POINT('Ctrl Pts',(-0.0179151371065852,0.0125415931621198,
-0.00871408984852256));
#54452=CARTESIAN_POINT('Ctrl Pts',(-0.0180036152858858,0.0133040947810426,
-0.00852474419803732));
#54453=CARTESIAN_POINT('Ctrl Pts',(-0.0180979273332784,0.0129456079522531,
-0.00846899320546831));
#54454=CARTESIAN_POINT('Ctrl Pts',(-0.0182549193196156,0.0126114534322405,
-0.00853386516266261));
#54455=CARTESIAN_POINT('Origin',(-0.0162718437026251,0.0114710202288522,
-0.0118595262637278));
#54456=CARTESIAN_POINT('Origin',(-0.0162272231559581,0.00948761256098469,
-0.0118855941465154));
#54457=CARTESIAN_POINT('Origin',(-0.0161828706141249,0.00750421019125213,
-0.0119121602717604));
#54458=CARTESIAN_POINT('Origin',(-0.0161265096054001,0.00500296106758063,
-0.0119313862398486));
#54459=CARTESIAN_POINT('Origin',(-0.0160755784276552,0.00250198330561054,
-0.0119617588041365));
#54460=CARTESIAN_POINT('Origin',(-0.0160741128491222,0.00194984566933334,
-0.0119837251183046));
#54461=CARTESIAN_POINT('Origin',(-0.0160636006313385,0.00139786661560786,
-0.0119901847128056));
#54462=CARTESIAN_POINT('Ctrl Pts',(-0.0168869404495504,0.000131743490843849,
-0.00918484788814817));
#54463=CARTESIAN_POINT('Ctrl Pts',(-0.0169535428340631,0.000396774408641604,
-0.00914547700026949));
#54464=CARTESIAN_POINT('Ctrl Pts',(-0.0170557052878066,0.000651905064219303,
-0.00917195430490026));
#54465=CARTESIAN_POINT('Ctrl Pts',(-0.0166593636290833,0.00020954577683886,
-0.00931937612688517));
#54466=CARTESIAN_POINT('Ctrl Pts',(-0.016726481573608,0.000456067210326956,
-0.0092797004742975));
#54467=CARTESIAN_POINT('Ctrl Pts',(-0.0168241943715066,0.000694725277275201,
-0.00929799565007616));
#54468=CARTESIAN_POINT('Ctrl Pts',(-0.0162745718659412,0.00035276616733443,
-0.0095468393547733));
#54469=CARTESIAN_POINT('Ctrl Pts',(-0.0163418806587457,0.000566569318729898,
-0.00950705088541729));
#54470=CARTESIAN_POINT('Ctrl Pts',(-0.0164319860313115,0.000775586085644678,
-0.00951209192699112));
#54471=CARTESIAN_POINT('Ctrl Pts',(-0.0157435500891547,0.000608559233710922,
-0.0098607440143753));
#54472=CARTESIAN_POINT('Ctrl Pts',(-0.0158093864852093,0.000767682664406866,
-0.00982182592778197));
#54473=CARTESIAN_POINT('Ctrl Pts',(-0.015888931254929,0.000924786987284052,
-0.00980979525072753));
#54474=CARTESIAN_POINT('Ctrl Pts',(-0.0152455191726649,0.000923698582799106,
-0.010155146677592));
#54475=CARTESIAN_POINT('Ctrl Pts',(-0.0153096498691124,0.00101745849940029,
-0.010117236886838));
#54476=CARTESIAN_POINT('Ctrl Pts',(-0.0153787082737323,0.00111153674305079,
-0.0100904302645169));
#54477=CARTESIAN_POINT('Ctrl Pts',(-0.0149409532646179,0.00132777528918322,
-0.01033518573036));
#54478=CARTESIAN_POINT('Ctrl Pts',(-0.0150024908282406,0.00134044710896269,
-0.0102988088268328));
#54479=CARTESIAN_POINT('Ctrl Pts',(-0.0150647545613132,0.00135322574523389,
-0.0102637678926917));
#54480=CARTESIAN_POINT('Ctrl Pts',(-0.0151243477084147,0.00165934770139,
-0.0102267751661056));
#54481=CARTESIAN_POINT('Ctrl Pts',(-0.0151867329811164,0.00160490768149151,
-0.0101898971534335));
#54482=CARTESIAN_POINT('Ctrl Pts',(-0.0152527703332342,0.00155031493930287,
-0.0101599578778916));
#54483=CARTESIAN_POINT('Origin',(-0.0177103885174519,0.000199999999999706,
-0.0110213870786426));
#54484=CARTESIAN_POINT('Ctrl Pts',(-0.018188824141858,8.75761564631602E-5,
-0.00837526872861006));
#54485=CARTESIAN_POINT('Ctrl Pts',(-0.0182113137141289,2.81913691597068E-5,
-0.00831630569299398));
#54486=CARTESIAN_POINT('Ctrl Pts',(-0.018236699754074,-3.41387128105288E-5,
-0.00826219897804721));
#54487=CARTESIAN_POINT('Ctrl Pts',(-0.0183955259428276,0.000103496198700443,
-0.00826521856849081));
#54488=CARTESIAN_POINT('Ctrl Pts',(-0.0184407613226512,9.46547266629223E-5,
-0.00823908285623541));
#54489=CARTESIAN_POINT('Ctrl Pts',(-0.0184860062356923,8.56578675476874E-5,
-0.00821299960804708));
#54490=CARTESIAN_POINT('Ctrl Pts',(-0.0182637622124833,0.000123294745978778,
-0.00835373521604812));
#54491=CARTESIAN_POINT('Ctrl Pts',(-0.0183265003447473,0.000173132371671092,
-0.0083432161596789));
#54492=CARTESIAN_POINT('Ctrl Pts',(-0.0183917093640185,0.000220491112436847,
-0.00833666232475801));
#54493=CARTESIAN_POINT('Ctrl Pts',(-0.0179561164070983,0.000144582042478119,
-0.0085441203472953));
#54494=CARTESIAN_POINT('Ctrl Pts',(-0.0180300450051964,0.000255262336695479,
-0.00853765036489813));
#54495=CARTESIAN_POINT('Ctrl Pts',(-0.0181118555578645,0.000360244421417436,
-0.0085449097825926));
#54496=CARTESIAN_POINT('Ctrl Pts',(-0.0175954738379551,0.000162245221859694,
-0.00876223422164232));
#54497=CARTESIAN_POINT('Ctrl Pts',(-0.0176724428971705,0.000322226944647927,
-0.00875072027092373));
#54498=CARTESIAN_POINT('Ctrl Pts',(-0.0177641850167143,0.000474023149858585,
-0.0087648460645389));
#54499=CARTESIAN_POINT('Ctrl Pts',(-0.0170914446330123,0.000182147225220522,
-0.00906348091051716));
#54500=CARTESIAN_POINT('Ctrl Pts',(-0.0171648487823219,0.000396867148245165,
-0.00903827421404887));
#54501=CARTESIAN_POINT('Ctrl Pts',(-0.0172630627038743,0.000602206025906414,
-0.00905647265972752));
#54502=CARTESIAN_POINT('Ctrl Pts',(-0.0167222986437901,0.000194047757030763,
-0.00928226818221012));
#54503=CARTESIAN_POINT('Ctrl Pts',(-0.0167893016430662,0.000441086163684428,
-0.00924365209871741));
#54504=CARTESIAN_POINT('Ctrl Pts',(-0.0168880399669533,0.000679646241829306,
-0.00926246702800065));
#54505=CARTESIAN_POINT('Ctrl Pts',(-0.0165064972234746,0.000200406501257873,
-0.00940983971047381));
#54506=CARTESIAN_POINT('Ctrl Pts',(-0.0165691023857454,0.000464672578914787,
-0.00936285258941367));
#54507=CARTESIAN_POINT('Ctrl Pts',(-0.01666733255564,0.000721498782670844,
-0.0093817265379391));
#54508=CARTESIAN_POINT('Origin',(-0.0192180740146401,-0.000823943018947793,
-0.00983819116336607));
#54509=CARTESIAN_POINT('Origin',(-0.0183316304034729,0.000200986509768273,
-0.00810139479829735));
#54510=CARTESIAN_POINT('Origin',(-0.00926982557395217,0.0172006855706717,
0.003));
#54511=CARTESIAN_POINT('',(-0.00926982557395217,0.0172006855706717,0.0035));
#54512=CARTESIAN_POINT('Origin',(-0.00926982557395217,0.0172006855706717,
-0.003));
#54513=CARTESIAN_POINT('',(-0.00926982557395217,0.0172006855706717,-0.0025));
#54514=CARTESIAN_POINT('Origin',(0.,0.0254,-0.011));
#54515=CARTESIAN_POINT('',(-6.12323399573677E-20,0.0254,-0.0105));
#54516=CARTESIAN_POINT('Origin',(0.,0.0254,0.011));
#54517=CARTESIAN_POINT('',(-6.12323399573677E-20,0.0254,0.0115));
#54518=CARTESIAN_POINT('Origin',(-0.139,0.0075,0.));
#54519=CARTESIAN_POINT('Origin',(-0.139,0.0075,-0.004));
#54520=CARTESIAN_POINT('',(0.,0.,0.));
#54521=CARTESIAN_POINT('Origin',(0.,0.,-0.00102870127000254));
#54522=CARTESIAN_POINT('',(0.001,0.,-0.0007874));
#54523=CARTESIAN_POINT('Origin',(0.,0.,-0.0007874));
#54524=CARTESIAN_POINT('',(6.29897858793714E-20,7.71402396561493E-36,0.));
#54525=CARTESIAN_POINT('Origin',(0.,0.,-0.00102870127000254));
#54526=CARTESIAN_POINT('Origin',(0.,0.,-0.0157874));
#54527=CARTESIAN_POINT('',(-0.0005,-6.12323399573677E-20,-0.0157874));
#54528=CARTESIAN_POINT('Origin',(0.,0.,-0.0157874));
#54529=CARTESIAN_POINT('Origin',(0.,0.,0.));
#54530=CARTESIAN_POINT('',(-0.0005,-6.12323399573677E-20,-0.0007874));
#54531=CARTESIAN_POINT('Origin',(0.,0.,-0.0007874));
#54532=CARTESIAN_POINT('',(-0.0005,-6.12323399573677E-20,0.));
#54533=CARTESIAN_POINT('Origin',(-0.001,0.,-0.0007874));
#54534=CARTESIAN_POINT('',(0.0126263809963694,0.00117758716122178,-0.0117308013308241));
#54535=CARTESIAN_POINT('',(0.,0.00110364159388398,0.00110364159388398));
#54536=CARTESIAN_POINT('',(0.0125059043198824,0.00107758716122178,0.00110364259453365));
#54537=CARTESIAN_POINT('',(0.,0.00110364159388398,0.00110364159388398));
#54538=CARTESIAN_POINT('',(0.0125059043198824,0.00107758716122178,0.00110364259453365));
#54539=CARTESIAN_POINT('',(0.,0.00110364159388398,0.00110364159388398));
#54540=CARTESIAN_POINT('',(0.,0.00110364159388398,0.00110364159388398));
#54541=CARTESIAN_POINT('',(-0.00927229144405574,-0.00190388426238738,-0.0151798864198938));
#54542=CARTESIAN_POINT('',(-0.00490823837246786,0.00110235630477852,0.000403641593883979));
#54543=CARTESIAN_POINT('',(0.0125059043198824,0.00107758716122178,0.00110364259453365));
#54544=CARTESIAN_POINT('',(-0.0050436401688439,0.00110832426718934,0.000250146449614664));
#54545=CARTESIAN_POINT('',(0.,0.00110364159388398,0.00110364159388398));
#54546=CARTESIAN_POINT('',(-0.0049930882441788,0.000918756290079796,-9.63584061160216E-5));
#54547=CARTESIAN_POINT('',(0.,0.00110364159388398,0.00110364159388398));
#54548=CARTESIAN_POINT('',(-0.00927229144405573,0.0041111674501554,-0.0151798864198938));
#54549=UNCERTAINTY_MEASURE_WITH_UNIT(LENGTH_MEASURE(1.E-5),#54581,
'DISTANCE_ACCURACY_VALUE',
'Maximum model space distance between geometric entities at asserted c
onnectivities');
#54550=UNCERTAINTY_MEASURE_WITH_UNIT(LENGTH_MEASURE(1.E-5),#54581,
'DISTANCE_ACCURACY_VALUE',
'Maximum model space distance between geometric entities at asserted c
onnectivities');
#54551=UNCERTAINTY_MEASURE_WITH_UNIT(LENGTH_MEASURE(1.E-5),#54581,
'DISTANCE_ACCURACY_VALUE',
'Maximum model space distance between geometric entities at asserted c
onnectivities');
#54552=UNCERTAINTY_MEASURE_WITH_UNIT(LENGTH_MEASURE(1.E-5),#54581,
'DISTANCE_ACCURACY_VALUE',
'Maximum model space distance between geometric entities at asserted c
onnectivities');
#54553=UNCERTAINTY_MEASURE_WITH_UNIT(LENGTH_MEASURE(1.E-5),#54581,
'DISTANCE_ACCURACY_VALUE',
'Maximum model space distance between geometric entities at asserted c
onnectivities');
#54554=UNCERTAINTY_MEASURE_WITH_UNIT(LENGTH_MEASURE(1.E-5),#54581,
'DISTANCE_ACCURACY_VALUE',
'Maximum model space distance between geometric entities at asserted c
onnectivities');
#54555=UNCERTAINTY_MEASURE_WITH_UNIT(LENGTH_MEASURE(1.E-5),#54581,
'DISTANCE_ACCURACY_VALUE',
'Maximum model space distance between geometric entities at asserted c
onnectivities');
#54556=UNCERTAINTY_MEASURE_WITH_UNIT(LENGTH_MEASURE(1.E-5),#54581,
'DISTANCE_ACCURACY_VALUE',
'Maximum model space distance between geometric entities at asserted c
onnectivities');
#54557=UNCERTAINTY_MEASURE_WITH_UNIT(LENGTH_MEASURE(1.E-5),#54581,
'DISTANCE_ACCURACY_VALUE',
'Maximum model space distance between geometric entities at asserted c
onnectivities');
#54558=UNCERTAINTY_MEASURE_WITH_UNIT(LENGTH_MEASURE(1.E-5),#54581,
'DISTANCE_ACCURACY_VALUE',
'Maximum model space distance between geometric entities at asserted c
onnectivities');
#54559=UNCERTAINTY_MEASURE_WITH_UNIT(LENGTH_MEASURE(1.E-5),#54581,
'DISTANCE_ACCURACY_VALUE',
'Maximum model space distance between geometric entities at asserted c
onnectivities');
#54560=UNCERTAINTY_MEASURE_WITH_UNIT(LENGTH_MEASURE(1.E-5),#54581,
'DISTANCE_ACCURACY_VALUE',
'Maximum model space distance between geometric entities at asserted c
onnectivities');
#54561=UNCERTAINTY_MEASURE_WITH_UNIT(LENGTH_MEASURE(1.E-5),#54581,
'DISTANCE_ACCURACY_VALUE',
'Maximum model space distance between geometric entities at asserted c
onnectivities');
#54562=UNCERTAINTY_MEASURE_WITH_UNIT(LENGTH_MEASURE(1.E-5),#54581,
'DISTANCE_ACCURACY_VALUE',
'Maximum model space distance between geometric entities at asserted c
onnectivities');
#54563=UNCERTAINTY_MEASURE_WITH_UNIT(LENGTH_MEASURE(1.E-5),#54581,
'DISTANCE_ACCURACY_VALUE',
'Maximum model space distance between geometric entities at asserted c
onnectivities');
#54564=UNCERTAINTY_MEASURE_WITH_UNIT(LENGTH_MEASURE(1.E-5),#54581,
'DISTANCE_ACCURACY_VALUE',
'Maximum model space distance between geometric entities at asserted c
onnectivities');
#54565=(
GEOMETRIC_REPRESENTATION_CONTEXT(3)
GLOBAL_UNCERTAINTY_ASSIGNED_CONTEXT((#54549))
GLOBAL_UNIT_ASSIGNED_CONTEXT((#54581,#54582,#54583))
REPRESENTATION_CONTEXT('','3D')
);
#54566=(
GEOMETRIC_REPRESENTATION_CONTEXT(3)
GLOBAL_UNCERTAINTY_ASSIGNED_CONTEXT((#54550))
GLOBAL_UNIT_ASSIGNED_CONTEXT((#54581,#54582,#54583))
REPRESENTATION_CONTEXT('','3D')
);
#54567=(
GEOMETRIC_REPRESENTATION_CONTEXT(3)
GLOBAL_UNCERTAINTY_ASSIGNED_CONTEXT((#54551))
GLOBAL_UNIT_ASSIGNED_CONTEXT((#54581,#54582,#54583))
REPRESENTATION_CONTEXT('','3D')
);
#54568=(
GEOMETRIC_REPRESENTATION_CONTEXT(3)
GLOBAL_UNCERTAINTY_ASSIGNED_CONTEXT((#54552))
GLOBAL_UNIT_ASSIGNED_CONTEXT((#54581,#54582,#54583))
REPRESENTATION_CONTEXT('','3D')
);
#54569=(
GEOMETRIC_REPRESENTATION_CONTEXT(3)
GLOBAL_UNCERTAINTY_ASSIGNED_CONTEXT((#54553))
GLOBAL_UNIT_ASSIGNED_CONTEXT((#54581,#54582,#54583))
REPRESENTATION_CONTEXT('','3D')
);
#54570=(
GEOMETRIC_REPRESENTATION_CONTEXT(3)
GLOBAL_UNCERTAINTY_ASSIGNED_CONTEXT((#54554))
GLOBAL_UNIT_ASSIGNED_CONTEXT((#54581,#54582,#54583))
REPRESENTATION_CONTEXT('','3D')
);
#54571=(
GEOMETRIC_REPRESENTATION_CONTEXT(3)
GLOBAL_UNCERTAINTY_ASSIGNED_CONTEXT((#54555))
GLOBAL_UNIT_ASSIGNED_CONTEXT((#54581,#54582,#54583))
REPRESENTATION_CONTEXT('','3D')
);
#54572=(
GEOMETRIC_REPRESENTATION_CONTEXT(3)
GLOBAL_UNCERTAINTY_ASSIGNED_CONTEXT((#54556))
GLOBAL_UNIT_ASSIGNED_CONTEXT((#54581,#54582,#54583))
REPRESENTATION_CONTEXT('','3D')
);
#54573=(
GEOMETRIC_REPRESENTATION_CONTEXT(3)
GLOBAL_UNCERTAINTY_ASSIGNED_CONTEXT((#54557))
GLOBAL_UNIT_ASSIGNED_CONTEXT((#54581,#54582,#54583))
REPRESENTATION_CONTEXT('','3D')
);
#54574=(
GEOMETRIC_REPRESENTATION_CONTEXT(3)
GLOBAL_UNCERTAINTY_ASSIGNED_CONTEXT((#54558))
GLOBAL_UNIT_ASSIGNED_CONTEXT((#54581,#54582,#54583))
REPRESENTATION_CONTEXT('','3D')
);
#54575=(
GEOMETRIC_REPRESENTATION_CONTEXT(3)
GLOBAL_UNCERTAINTY_ASSIGNED_CONTEXT((#54559))
GLOBAL_UNIT_ASSIGNED_CONTEXT((#54581,#54582,#54583))
REPRESENTATION_CONTEXT('','3D')
);
#54576=(
GEOMETRIC_REPRESENTATION_CONTEXT(3)
GLOBAL_UNCERTAINTY_ASSIGNED_CONTEXT((#54560))
GLOBAL_UNIT_ASSIGNED_CONTEXT((#54581,#54582,#54583))
REPRESENTATION_CONTEXT('','3D')
);
#54577=(
GEOMETRIC_REPRESENTATION_CONTEXT(3)
GLOBAL_UNCERTAINTY_ASSIGNED_CONTEXT((#54561))
GLOBAL_UNIT_ASSIGNED_CONTEXT((#54581,#54582,#54583))
REPRESENTATION_CONTEXT('','3D')
);
#54578=(
GEOMETRIC_REPRESENTATION_CONTEXT(3)
GLOBAL_UNCERTAINTY_ASSIGNED_CONTEXT((#54562))
GLOBAL_UNIT_ASSIGNED_CONTEXT((#54581,#54582,#54583))
REPRESENTATION_CONTEXT('','3D')
);
#54579=(
GEOMETRIC_REPRESENTATION_CONTEXT(3)
GLOBAL_UNCERTAINTY_ASSIGNED_CONTEXT((#54563))
GLOBAL_UNIT_ASSIGNED_CONTEXT((#54581,#54582,#54583))
REPRESENTATION_CONTEXT('','3D')
);
#54580=(
GEOMETRIC_REPRESENTATION_CONTEXT(3)
GLOBAL_UNCERTAINTY_ASSIGNED_CONTEXT((#54564))
GLOBAL_UNIT_ASSIGNED_CONTEXT((#54581,#54582,#54583))
REPRESENTATION_CONTEXT('','3D')
);
#54581=(
LENGTH_UNIT()
NAMED_UNIT(*)
SI_UNIT($,.METRE.)
);
#54582=(
NAMED_UNIT(*)
PLANE_ANGLE_UNIT()
SI_UNIT($,.RADIAN.)
);
#54583=(
NAMED_UNIT(*)
SI_UNIT($,.STERADIAN.)
SOLID_ANGLE_UNIT()
);
#54584=SHAPE_DEFINITION_REPRESENTATION(#54599,#54629);
#54585=SHAPE_DEFINITION_REPRESENTATION(#54600,#54630);
#54586=SHAPE_DEFINITION_REPRESENTATION(#54601,#54631);
#54587=SHAPE_DEFINITION_REPRESENTATION(#54602,#54632);
#54588=SHAPE_DEFINITION_REPRESENTATION(#54603,#54633);
#54589=SHAPE_DEFINITION_REPRESENTATION(#54604,#54634);
#54590=SHAPE_DEFINITION_REPRESENTATION(#54605,#54635);
#54591=SHAPE_DEFINITION_REPRESENTATION(#54606,#54636);
#54592=SHAPE_DEFINITION_REPRESENTATION(#54607,#54637);
#54593=SHAPE_DEFINITION_REPRESENTATION(#54608,#54638);
#54594=SHAPE_DEFINITION_REPRESENTATION(#54609,#54639);
#54595=SHAPE_DEFINITION_REPRESENTATION(#54610,#54640);
#54596=SHAPE_DEFINITION_REPRESENTATION(#54611,#54641);
#54597=SHAPE_DEFINITION_REPRESENTATION(#54612,#54642);
#54598=SHAPE_DEFINITION_REPRESENTATION(#54613,#54643);
#54599=PRODUCT_DEFINITION_SHAPE('',$,#54645);
#54600=PRODUCT_DEFINITION_SHAPE('',$,#54646);
#54601=PRODUCT_DEFINITION_SHAPE('',$,#54647);
#54602=PRODUCT_DEFINITION_SHAPE('',$,#54648);
#54603=PRODUCT_DEFINITION_SHAPE('',$,#54649);
#54604=PRODUCT_DEFINITION_SHAPE('',$,#54650);
#54605=PRODUCT_DEFINITION_SHAPE('',$,#54651);
#54606=PRODUCT_DEFINITION_SHAPE('',$,#54652);
#54607=PRODUCT_DEFINITION_SHAPE('',$,#54653);
#54608=PRODUCT_DEFINITION_SHAPE('',$,#54654);
#54609=PRODUCT_DEFINITION_SHAPE('',$,#54655);
#54610=PRODUCT_DEFINITION_SHAPE('',$,#54656);
#54611=PRODUCT_DEFINITION_SHAPE('',$,#54657);
#54612=PRODUCT_DEFINITION_SHAPE('',$,#54658);
#54613=PRODUCT_DEFINITION_SHAPE('',$,#54659);
#54614=PRODUCT_DEFINITION_SHAPE($,$,#56);
#54615=PRODUCT_DEFINITION_SHAPE($,$,#57);
#54616=PRODUCT_DEFINITION_SHAPE($,$,#58);
#54617=PRODUCT_DEFINITION_SHAPE($,$,#59);
#54618=PRODUCT_DEFINITION_SHAPE($,$,#60);
#54619=PRODUCT_DEFINITION_SHAPE($,$,#61);
#54620=PRODUCT_DEFINITION_SHAPE($,$,#62);
#54621=PRODUCT_DEFINITION_SHAPE($,$,#63);
#54622=PRODUCT_DEFINITION_SHAPE($,$,#64);
#54623=PRODUCT_DEFINITION_SHAPE($,$,#65);
#54624=PRODUCT_DEFINITION_SHAPE($,$,#66);
#54625=PRODUCT_DEFINITION_SHAPE($,$,#67);
#54626=PRODUCT_DEFINITION_SHAPE($,$,#68);
#54627=PRODUCT_DEFINITION_SHAPE($,$,#69);
#54628=PRODUCT_DEFINITION_SHAPE($,$,#70);
#54629=SHAPE_REPRESENTATION('',(#17835,#19586,#19587,#19588,#19589,#19590,
#19591,#19592,#19593,#19594,#19595,#19596,#19597,#19598,#19599,#19600),
#54565);
#54630=SHAPE_REPRESENTATION('',(#17836),#54566);
#54631=SHAPE_REPRESENTATION('',(#18394),#54567);
#54632=SHAPE_REPRESENTATION('',(#18517),#54568);
#54633=SHAPE_REPRESENTATION('',(#18520),#54569);
#54634=SHAPE_REPRESENTATION('',(#18747),#54570);
#54635=SHAPE_REPRESENTATION('',(#18812),#54571);
#54636=SHAPE_REPRESENTATION('',(#18922),#54572);
#54637=SHAPE_REPRESENTATION('',(#19048),#54573);
#54638=SHAPE_REPRESENTATION('',(#19063),#54574);
#54639=SHAPE_REPRESENTATION('',(#19079),#54575);
#54640=SHAPE_REPRESENTATION('',(#19138),#54576);
#54641=SHAPE_REPRESENTATION('',(#19199),#54577);
#54642=SHAPE_REPRESENTATION('',(#19293),#54578);
#54643=SHAPE_REPRESENTATION('',(#19577),#54579);
#54644=PRODUCT_DEFINITION_CONTEXT('part definition',#54691,'design');
#54645=PRODUCT_DEFINITION('Assembly 1','MAS-615',#54660,#54644);
#54646=PRODUCT_DEFINITION('Part_7','Part_7',#54661,#54644);
#54647=PRODUCT_DEFINITION('Part_8','Part_8',#54662,#54644);
#54648=PRODUCT_DEFINITION('Part_12','Part_12',#54663,#54644);
#54649=PRODUCT_DEFINITION('Part_10','Part_10',#54664,#54644);
#54650=PRODUCT_DEFINITION('sockethead','Sockethead',#54665,#54644);
#54651=PRODUCT_DEFINITION('Part_4','Part_4',#54666,#54644);
#54652=PRODUCT_DEFINITION('Part_6','Part_6',#54667,#54644);
#54653=PRODUCT_DEFINITION('Part_11','Part_11',#54668,#54644);
#54654=PRODUCT_DEFINITION('gearhub','Gearhub',#54669,#54644);
#54655=PRODUCT_DEFINITION('Part_3','Part_3',#54670,#54644);
#54656=PRODUCT_DEFINITION('Part_5','Part_5',#54671,#54644);
#54657=PRODUCT_DEFINITION('Part_2','Part_2',#54672,#54644);
#54658=PRODUCT_DEFINITION('Part_9','Part_9',#54673,#54644);
#54659=PRODUCT_DEFINITION('Part_1','Part_1',#54674,#54644);
#54660=PRODUCT_DEFINITION_FORMATION('',$,#54693);
#54661=PRODUCT_DEFINITION_FORMATION('',$,#54694);
#54662=PRODUCT_DEFINITION_FORMATION('',$,#54695);
#54663=PRODUCT_DEFINITION_FORMATION('',$,#54696);
#54664=PRODUCT_DEFINITION_FORMATION('',$,#54697);
#54665=PRODUCT_DEFINITION_FORMATION('',$,#54698);
#54666=PRODUCT_DEFINITION_FORMATION('',$,#54699);
#54667=PRODUCT_DEFINITION_FORMATION('',$,#54700);
#54668=PRODUCT_DEFINITION_FORMATION('',$,#54701);
#54669=PRODUCT_DEFINITION_FORMATION('',$,#54702);
#54670=PRODUCT_DEFINITION_FORMATION('',$,#54703);
#54671=PRODUCT_DEFINITION_FORMATION('',$,#54704);
#54672=PRODUCT_DEFINITION_FORMATION('',$,#54705);
#54673=PRODUCT_DEFINITION_FORMATION('',$,#54706);
#54674=PRODUCT_DEFINITION_FORMATION('',$,#54707);
#54675=PRODUCT_RELATED_PRODUCT_CATEGORY('MAS-615','MAS-615',(#54693));
#54676=PRODUCT_RELATED_PRODUCT_CATEGORY('Part_7','Part_7',(#54694));
#54677=PRODUCT_RELATED_PRODUCT_CATEGORY('Part_8','Part_8',(#54695));
#54678=PRODUCT_RELATED_PRODUCT_CATEGORY('Part_12','Part_12',(#54696));
#54679=PRODUCT_RELATED_PRODUCT_CATEGORY('Part_10','Part_10',(#54697));
#54680=PRODUCT_RELATED_PRODUCT_CATEGORY('Sockethead','Sockethead',(#54698));
#54681=PRODUCT_RELATED_PRODUCT_CATEGORY('Part_4','Part_4',(#54699));
#54682=PRODUCT_RELATED_PRODUCT_CATEGORY('Part_6','Part_6',(#54700));
#54683=PRODUCT_RELATED_PRODUCT_CATEGORY('Part_11','Part_11',(#54701));
#54684=PRODUCT_RELATED_PRODUCT_CATEGORY('Gearhub','Gearhub',(#54702));
#54685=PRODUCT_RELATED_PRODUCT_CATEGORY('Part_3','Part_3',(#54703));
#54686=PRODUCT_RELATED_PRODUCT_CATEGORY('Part_5','Part_5',(#54704));
#54687=PRODUCT_RELATED_PRODUCT_CATEGORY('Part_2','Part_2',(#54705));
#54688=PRODUCT_RELATED_PRODUCT_CATEGORY('Part_9','Part_9',(#54706));
#54689=PRODUCT_RELATED_PRODUCT_CATEGORY('Part_1','Part_1',(#54707));
#54690=APPLICATION_PROTOCOL_DEFINITION('international standard',
'automotive_design',2009,#54691);
#54691=APPLICATION_CONTEXT(
'Core Data for Automotive Mechanical Design Process');
#54692=PRODUCT_CONTEXT('part definition',#54691,'mechanical');
#54693=PRODUCT('Assembly 1','MAS-615','STEP AP242 Edition 2',(#54692));
#54694=PRODUCT('Part_7','Part_7','Part 1',(#54692));
#54695=PRODUCT('Part_8','Part_8','Part 1',(#54692));
#54696=PRODUCT('Part_12','Part_12','Part 1',(#54692));
#54697=PRODUCT('Part_10','Part_10','Part 1',(#54692));
#54698=PRODUCT('sockethead','Sockethead','sockethead',(#54692));
#54699=PRODUCT('Part_4','Part_4','Part 1',(#54692));
#54700=PRODUCT('Part_6','Part_6','Part 1',(#54692));
#54701=PRODUCT('Part_11','Part_11','Part 1',(#54692));
#54702=PRODUCT('gearhub','Gearhub','gearhub',(#54692));
#54703=PRODUCT('Part_3','Part_3','Part 1',(#54692));
#54704=PRODUCT('Part_5','Part_5','Part 1',(#54692));
#54705=PRODUCT('Part_2','Part_2','Part 2',(#54692));
#54706=PRODUCT('Part_9','Part_9','Part 1',(#54692));
#54707=PRODUCT('Part_1','Part_1','Part 1',(#54692));
#54708=PRESENTATION_STYLE_ASSIGNMENT((#54718));
#54709=PRESENTATION_STYLE_ASSIGNMENT((#54719));
#54710=PRESENTATION_STYLE_ASSIGNMENT((#54720));
#54711=PRESENTATION_STYLE_ASSIGNMENT((#54721));
#54712=PRESENTATION_STYLE_ASSIGNMENT((#54722));
#54713=PRESENTATION_STYLE_ASSIGNMENT((#54723));
#54714=PRESENTATION_STYLE_ASSIGNMENT((#54724));
#54715=PRESENTATION_STYLE_ASSIGNMENT((#54725));
#54716=PRESENTATION_STYLE_ASSIGNMENT((#54726));
#54717=PRESENTATION_STYLE_ASSIGNMENT((#54727));
#54718=SURFACE_STYLE_USAGE(.BOTH.,#54728);
#54719=SURFACE_STYLE_USAGE(.BOTH.,#54729);
#54720=SURFACE_STYLE_USAGE(.BOTH.,#54730);
#54721=SURFACE_STYLE_USAGE(.BOTH.,#54731);
#54722=SURFACE_STYLE_USAGE(.BOTH.,#54732);
#54723=SURFACE_STYLE_USAGE(.BOTH.,#54733);
#54724=SURFACE_STYLE_USAGE(.BOTH.,#54734);
#54725=SURFACE_STYLE_USAGE(.BOTH.,#54735);
#54726=SURFACE_STYLE_USAGE(.BOTH.,#54736);
#54727=SURFACE_STYLE_USAGE(.BOTH.,#54737);
#54728=SURFACE_SIDE_STYLE('',(#54738));
#54729=SURFACE_SIDE_STYLE('',(#54739));
#54730=SURFACE_SIDE_STYLE('',(#54740));
#54731=SURFACE_SIDE_STYLE('',(#54741));
#54732=SURFACE_SIDE_STYLE('',(#54742));
#54733=SURFACE_SIDE_STYLE('',(#54743));
#54734=SURFACE_SIDE_STYLE('',(#54744));
#54735=SURFACE_SIDE_STYLE('',(#54745));
#54736=SURFACE_SIDE_STYLE('',(#54746));
#54737=SURFACE_SIDE_STYLE('',(#54747));
#54738=SURFACE_STYLE_FILL_AREA(#54748);
#54739=SURFACE_STYLE_FILL_AREA(#54749);
#54740=SURFACE_STYLE_FILL_AREA(#54750);
#54741=SURFACE_STYLE_FILL_AREA(#54751);
#54742=SURFACE_STYLE_FILL_AREA(#54752);
#54743=SURFACE_STYLE_FILL_AREA(#54753);
#54744=SURFACE_STYLE_FILL_AREA(#54754);
#54745=SURFACE_STYLE_FILL_AREA(#54755);
#54746=SURFACE_STYLE_FILL_AREA(#54756);
#54747=SURFACE_STYLE_FILL_AREA(#54757);
#54748=FILL_AREA_STYLE('Steel - Satin',(#54758));
#54749=FILL_AREA_STYLE('Opaque(153,153,153)',(#54759));
#54750=FILL_AREA_STYLE('Opaque(170,178,196)',(#54760));
#54751=FILL_AREA_STYLE('Opaque(229,234,237)',(#54761));
#54752=FILL_AREA_STYLE('Opaque(26,26,26)',(#54762));
#54753=FILL_AREA_STYLE('Opaque(163,170,173)',(#54763));
#54754=FILL_AREA_STYLE('Opaque(73,169,84)',(#54764));
#54755=FILL_AREA_STYLE('Opaque(15,15,15)',(#54765));
#54756=FILL_AREA_STYLE('Opaque(76,76,76)',(#54766));
#54757=FILL_AREA_STYLE('Opaque(202,209,238)',(#54767));
#54758=FILL_AREA_STYLE_COLOUR('Steel - Satin',#54768);
#54759=FILL_AREA_STYLE_COLOUR('Opaque(153,153,153)',#54769);
#54760=FILL_AREA_STYLE_COLOUR('Opaque(170,178,196)',#54770);
#54761=FILL_AREA_STYLE_COLOUR('Opaque(229,234,237)',#54771);
#54762=FILL_AREA_STYLE_COLOUR('Opaque(26,26,26)',#54772);
#54763=FILL_AREA_STYLE_COLOUR('Opaque(163,170,173)',#54773);
#54764=FILL_AREA_STYLE_COLOUR('Opaque(73,169,84)',#54774);
#54765=FILL_AREA_STYLE_COLOUR('Opaque(15,15,15)',#54775);
#54766=FILL_AREA_STYLE_COLOUR('Opaque(76,76,76)',#54776);
#54767=FILL_AREA_STYLE_COLOUR('Opaque(202,209,238)',#54777);
#54768=COLOUR_RGB('Steel - Satin', 0.09019608, 0.27058824, 0.51372549);
#54769=COLOUR_RGB('Opaque(153,153,153)', 0.09019608, 0.27058824, 0.51372549);
#54770=COLOUR_RGB('Opaque(170,178,196)', 0.66274510, 0.83137255, 0.94901961);
#54771=COLOUR_RGB('Opaque(229,234,237)', 0.40784314, 0.44705882, 0.49803922);
#54772=COLOUR_RGB('Opaque(26,26,26)', 0.66274510, 0.83137255, 0.94901961);
#54773=COLOUR_RGB('Opaque(163,170,173)', 0.31764706, 0.68627451, 0.89019608);
#54774=COLOUR_RGB('Opaque(73,169,84)', 0.40784314, 0.44705882, 0.49803922);
#54775=COLOUR_RGB('Opaque(15,15,15)', 0.72549020, 0.75294118, 0.79215686);
#54776=COLOUR_RGB('Opaque(76,76,76)', 0.08235294, 0.09019608, 0.10196078);
#54777=COLOUR_RGB('Opaque(202,209,238)', 0.09019608, 0.27058824, 0.51372549);
ENDSEC;
END-ISO-10303-21;
